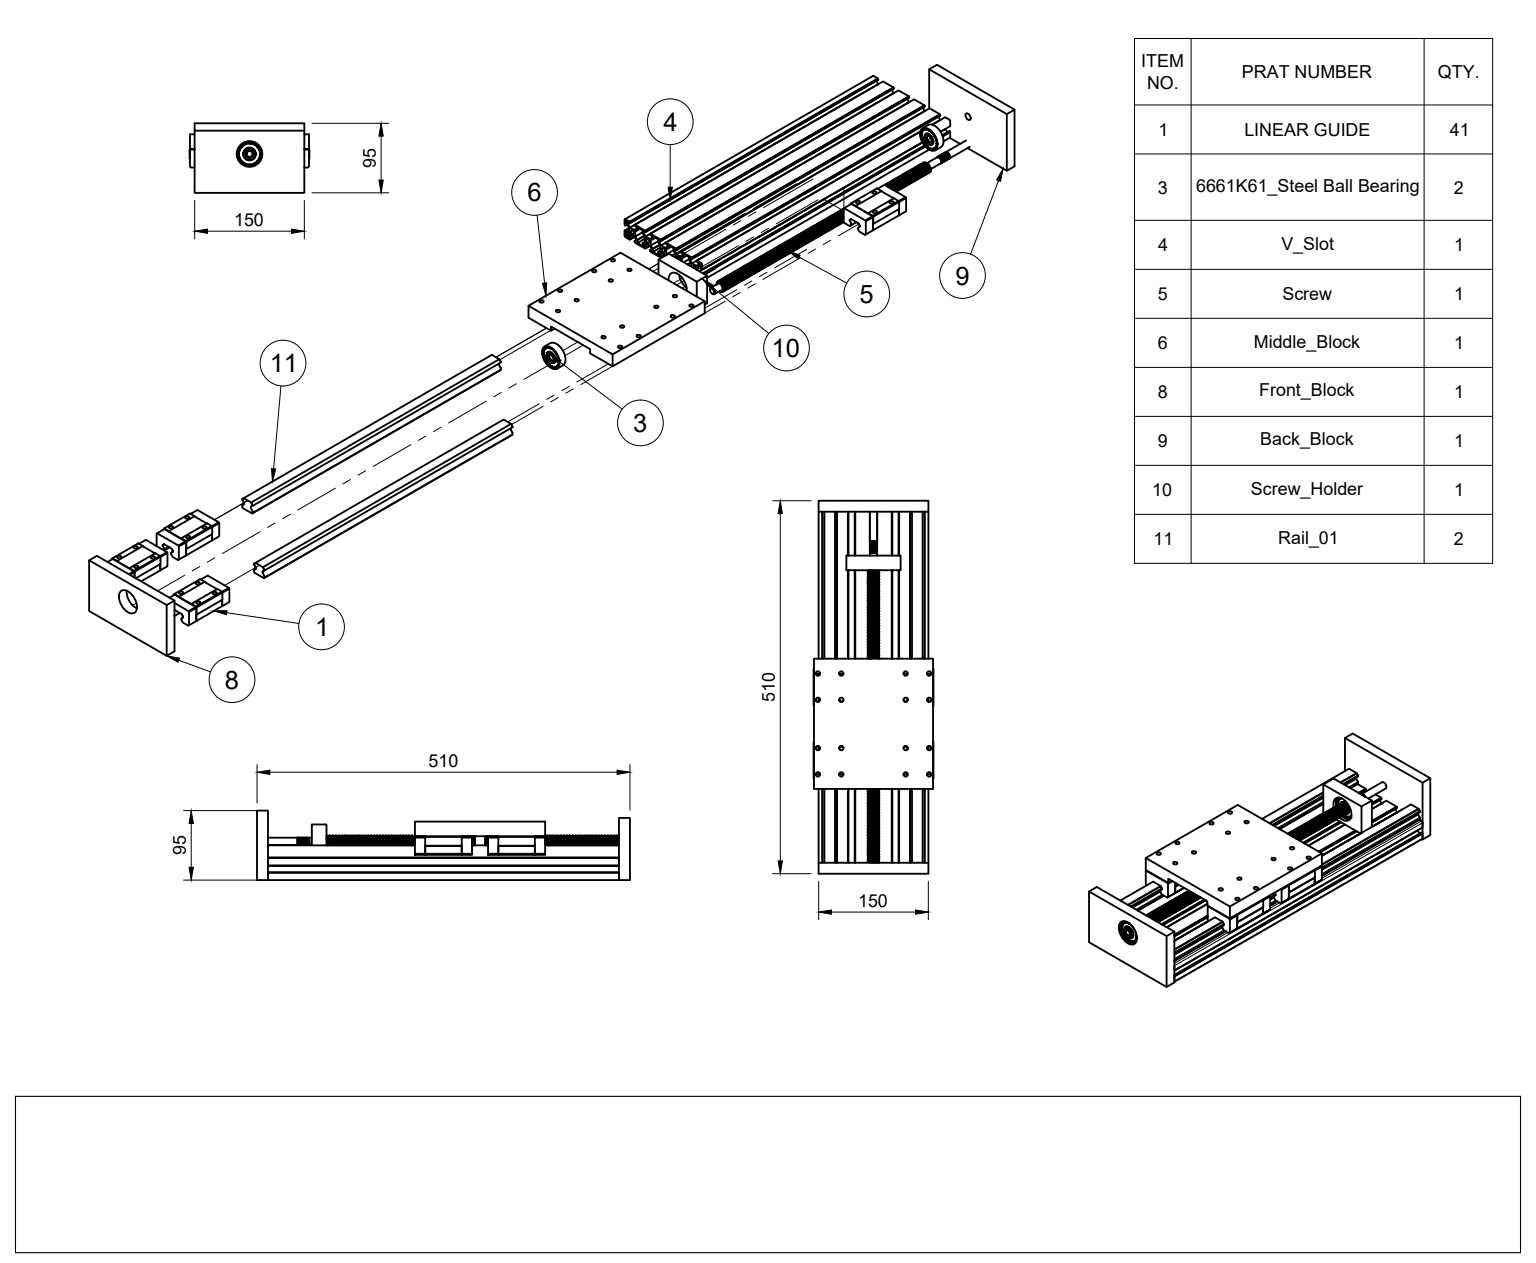
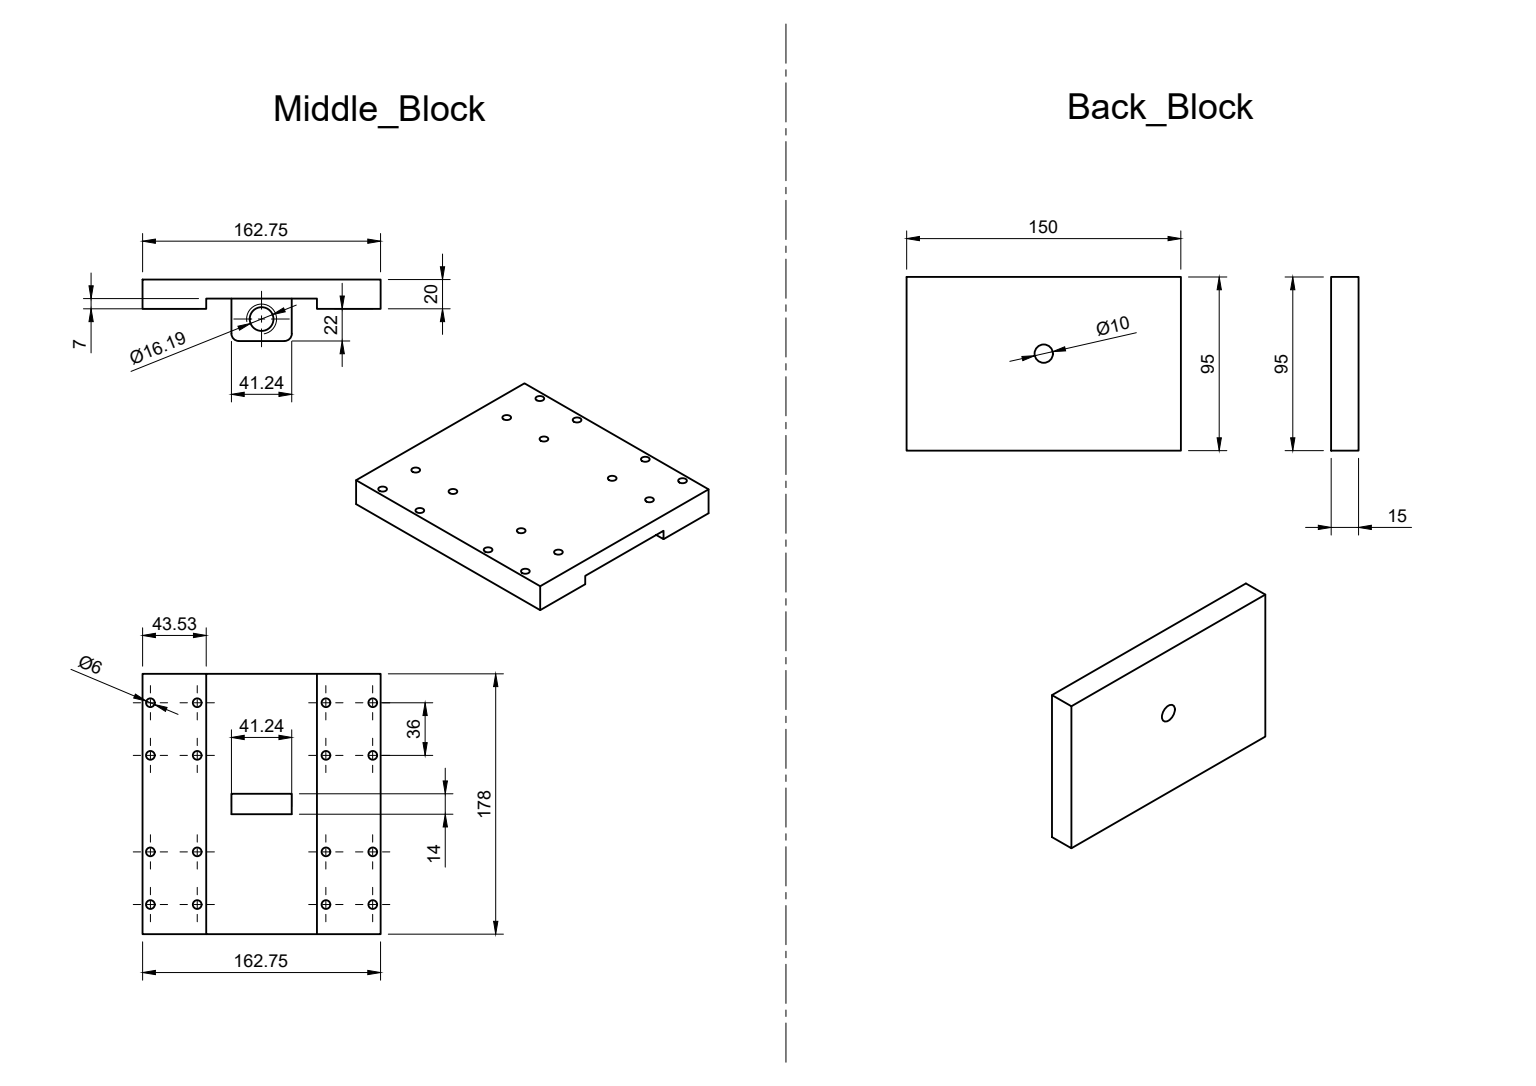
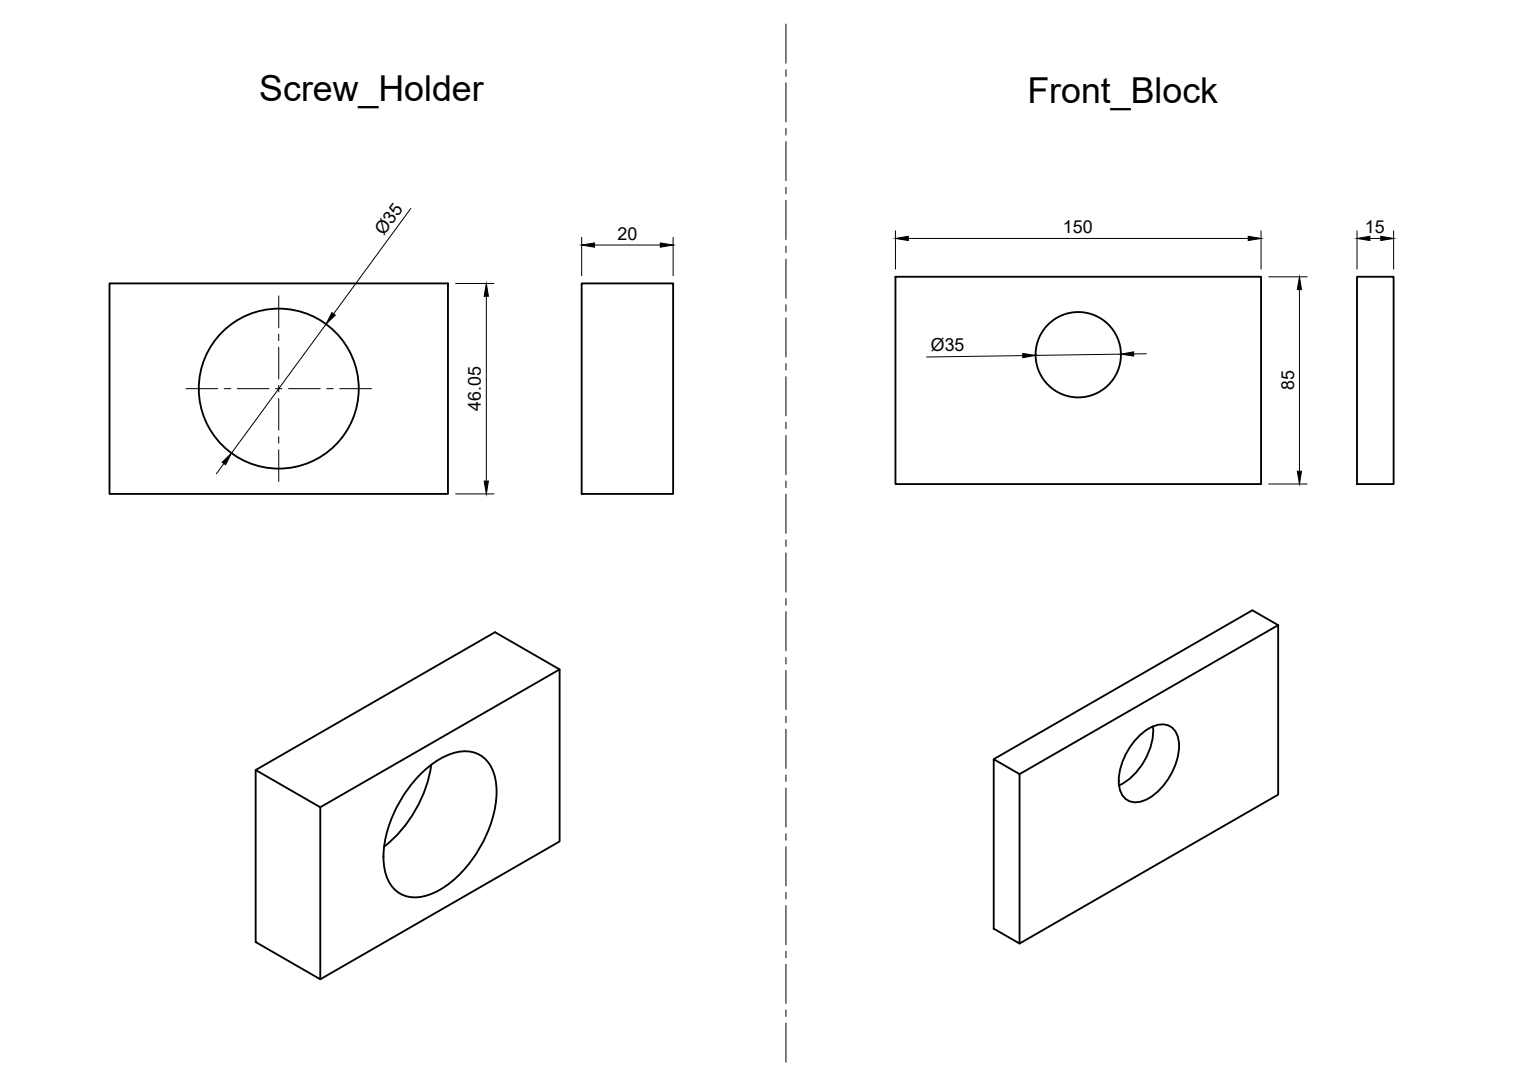
ISO-10303-21;
HEADER;
/* Generated by software containing ST-Developer
 * from STEP Tools, Inc. (www.steptools.com) 
 */

FILE_DESCRIPTION(
/* description */ (''),
/* implementation_level */ '2;1');

FILE_NAME(
/* name */ 'MAS-268',
/* time_stamp */ '2026-10-19T01:17:59+06:00',
/* author */ (''),
/* organization */ (''),
/* preprocessor_version */ 'ST-DEVELOPER v20.2',
/* originating_system */ 'Autodesk Translation Framework v15.15.0.0',
/* authorisation */ '');

FILE_SCHEMA (('AUTOMOTIVE_DESIGN { 1 0 10303 214 3 1 1 }'));
ENDSEC;

DATA;
#10=MECHANICAL_DESIGN_GEOMETRIC_PRESENTATION_REPRESENTATION('',(#729,#730,
#731,#732,#733,#734,#735,#736,#737,#738,#739,#740,#741,#742,#743,#744,#745,
#746,#747,#748,#749,#750,#751,#752,#753,#754),#48369);
#11=ITEM_DEFINED_TRANSFORMATION($,$,#20492,#21912);
#12=ITEM_DEFINED_TRANSFORMATION($,$,#20727,#21913);
#13=ITEM_DEFINED_TRANSFORMATION($,$,#20257,#21914);
#14=ITEM_DEFINED_TRANSFORMATION($,$,#20257,#21915);
#15=ITEM_DEFINED_TRANSFORMATION($,$,#20492,#21916);
#16=ITEM_DEFINED_TRANSFORMATION($,$,#20727,#21917);
#17=ITEM_DEFINED_TRANSFORMATION($,$,#21080,#21918);
#18=ITEM_DEFINED_TRANSFORMATION($,$,#21410,#21919);
#19=ITEM_DEFINED_TRANSFORMATION($,$,#21663,#21920);
#20=ITEM_DEFINED_TRANSFORMATION($,$,#21736,#21921);
#21=ITEM_DEFINED_TRANSFORMATION($,$,#21809,#21922);
#22=ITEM_DEFINED_TRANSFORMATION($,$,#21819,#21923);
#23=ITEM_DEFINED_TRANSFORMATION($,$,#21829,#21924);
#24=ITEM_DEFINED_TRANSFORMATION($,$,#21839,#21925);
#25=(
REPRESENTATION_RELATIONSHIP($,$,#48414,#48412)
REPRESENTATION_RELATIONSHIP_WITH_TRANSFORMATION(#11)
SHAPE_REPRESENTATION_RELATIONSHIP()
);
#26=(
REPRESENTATION_RELATIONSHIP($,$,#48415,#48412)
REPRESENTATION_RELATIONSHIP_WITH_TRANSFORMATION(#12)
SHAPE_REPRESENTATION_RELATIONSHIP()
);
#27=(
REPRESENTATION_RELATIONSHIP($,$,#48413,#48412)
REPRESENTATION_RELATIONSHIP_WITH_TRANSFORMATION(#13)
SHAPE_REPRESENTATION_RELATIONSHIP()
);
#28=(
REPRESENTATION_RELATIONSHIP($,$,#48413,#48412)
REPRESENTATION_RELATIONSHIP_WITH_TRANSFORMATION(#14)
SHAPE_REPRESENTATION_RELATIONSHIP()
);
#29=(
REPRESENTATION_RELATIONSHIP($,$,#48414,#48412)
REPRESENTATION_RELATIONSHIP_WITH_TRANSFORMATION(#15)
SHAPE_REPRESENTATION_RELATIONSHIP()
);
#30=(
REPRESENTATION_RELATIONSHIP($,$,#48415,#48412)
REPRESENTATION_RELATIONSHIP_WITH_TRANSFORMATION(#16)
SHAPE_REPRESENTATION_RELATIONSHIP()
);
#31=(
REPRESENTATION_RELATIONSHIP($,$,#48416,#48412)
REPRESENTATION_RELATIONSHIP_WITH_TRANSFORMATION(#17)
SHAPE_REPRESENTATION_RELATIONSHIP()
);
#32=(
REPRESENTATION_RELATIONSHIP($,$,#48417,#48412)
REPRESENTATION_RELATIONSHIP_WITH_TRANSFORMATION(#18)
SHAPE_REPRESENTATION_RELATIONSHIP()
);
#33=(
REPRESENTATION_RELATIONSHIP($,$,#48418,#48412)
REPRESENTATION_RELATIONSHIP_WITH_TRANSFORMATION(#19)
SHAPE_REPRESENTATION_RELATIONSHIP()
);
#34=(
REPRESENTATION_RELATIONSHIP($,$,#48419,#48412)
REPRESENTATION_RELATIONSHIP_WITH_TRANSFORMATION(#20)
SHAPE_REPRESENTATION_RELATIONSHIP()
);
#35=(
REPRESENTATION_RELATIONSHIP($,$,#48420,#48412)
REPRESENTATION_RELATIONSHIP_WITH_TRANSFORMATION(#21)
SHAPE_REPRESENTATION_RELATIONSHIP()
);
#36=(
REPRESENTATION_RELATIONSHIP($,$,#48421,#48412)
REPRESENTATION_RELATIONSHIP_WITH_TRANSFORMATION(#22)
SHAPE_REPRESENTATION_RELATIONSHIP()
);
#37=(
REPRESENTATION_RELATIONSHIP($,$,#48422,#48412)
REPRESENTATION_RELATIONSHIP_WITH_TRANSFORMATION(#23)
SHAPE_REPRESENTATION_RELATIONSHIP()
);
#38=(
REPRESENTATION_RELATIONSHIP($,$,#48423,#48412)
REPRESENTATION_RELATIONSHIP_WITH_TRANSFORMATION(#24)
SHAPE_REPRESENTATION_RELATIONSHIP()
);
#39=CONTEXT_DEPENDENT_SHAPE_REPRESENTATION(#25,#48398);
#40=CONTEXT_DEPENDENT_SHAPE_REPRESENTATION(#26,#48399);
#41=CONTEXT_DEPENDENT_SHAPE_REPRESENTATION(#27,#48400);
#42=CONTEXT_DEPENDENT_SHAPE_REPRESENTATION(#28,#48401);
#43=CONTEXT_DEPENDENT_SHAPE_REPRESENTATION(#29,#48402);
#44=CONTEXT_DEPENDENT_SHAPE_REPRESENTATION(#30,#48403);
#45=CONTEXT_DEPENDENT_SHAPE_REPRESENTATION(#31,#48404);
#46=CONTEXT_DEPENDENT_SHAPE_REPRESENTATION(#32,#48405);
#47=CONTEXT_DEPENDENT_SHAPE_REPRESENTATION(#33,#48406);
#48=CONTEXT_DEPENDENT_SHAPE_REPRESENTATION(#34,#48407);
#49=CONTEXT_DEPENDENT_SHAPE_REPRESENTATION(#35,#48408);
#50=CONTEXT_DEPENDENT_SHAPE_REPRESENTATION(#36,#48409);
#51=CONTEXT_DEPENDENT_SHAPE_REPRESENTATION(#37,#48410);
#52=CONTEXT_DEPENDENT_SHAPE_REPRESENTATION(#38,#48411);
#53=NEXT_ASSEMBLY_USAGE_OCCURRENCE('LINEAR GUIDE:1','LINEAR GUIDE:1',
'LINEAR GUIDE:1',#48425,#48427,'LINEAR GUIDE:1');
#54=NEXT_ASSEMBLY_USAGE_OCCURRENCE('6661K61_Steel Ball Bearing:1',
'6661K61_Steel Ball Bearing:1','6661K61_Steel Ball Bearing:1',#48425,#48428,
'6661K61_Steel Ball Bearing:1');
#55=NEXT_ASSEMBLY_USAGE_OCCURRENCE('LINEAR GUIDE(Mirror):1',
'LINEAR GUIDE(Mirror):1','LINEAR GUIDE(Mirror):1',#48425,#48426,
'LINEAR GUIDE(Mirror):1');
#56=NEXT_ASSEMBLY_USAGE_OCCURRENCE('LINEAR GUIDE(Mirror):2',
'LINEAR GUIDE(Mirror):2','LINEAR GUIDE(Mirror):2',#48425,#48426,
'LINEAR GUIDE(Mirror):2');
#57=NEXT_ASSEMBLY_USAGE_OCCURRENCE('LINEAR GUIDE:2','LINEAR GUIDE:2',
'LINEAR GUIDE:2',#48425,#48427,'LINEAR GUIDE:2');
#58=NEXT_ASSEMBLY_USAGE_OCCURRENCE('6661K61_Steel Ball Bearing:2',
'6661K61_Steel Ball Bearing:2','6661K61_Steel Ball Bearing:2',#48425,#48428,
'6661K61_Steel Ball Bearing:2');
#59=NEXT_ASSEMBLY_USAGE_OCCURRENCE('V_Slot:1','V_Slot:1','V_Slot:1',#48425,
#48429,'V_Slot:1');
#60=NEXT_ASSEMBLY_USAGE_OCCURRENCE('Screw:1','Screw:1','Screw:1',#48425,
#48430,'Screw:1');
#61=NEXT_ASSEMBLY_USAGE_OCCURRENCE('Middle_Block:1','Middle_Block:1',
'Middle_Block:1',#48425,#48431,'Middle_Block:1');
#62=NEXT_ASSEMBLY_USAGE_OCCURRENCE('Rail_02:1','Rail_02:1','Rail_02:1',
#48425,#48432,'Rail_02:1');
#63=NEXT_ASSEMBLY_USAGE_OCCURRENCE('Front_Block:1','Front_Block:1',
'Front_Block:1',#48425,#48433,'Front_Block:1');
#64=NEXT_ASSEMBLY_USAGE_OCCURRENCE('Back_Block:1','Back_Block:1',
'Back_Block:1',#48425,#48434,'Back_Block:1');
#65=NEXT_ASSEMBLY_USAGE_OCCURRENCE('Screw_Holder:1','Screw_Holder:1',
'Screw_Holder:1',#48425,#48435,'Screw_Holder:1');
#66=NEXT_ASSEMBLY_USAGE_OCCURRENCE('Rail_01:1','Rail_01:1','Rail_01:1',
#48425,#48436,'Rail_01:1');
#67=B_SPLINE_SURFACE_WITH_KNOTS('',3,3,((#40580,#40581,#40582,#40583,#40584,
#40585,#40586,#40587,#40588,#40589,#40590,#40591,#40592,#40593,#40594,#40595,
#40596,#40597,#40598,#40599,#40600,#40601,#40602,#40603,#40604,#40605,#40606,
#40607,#40608,#40609,#40610,#40611,#40612,#40613,#40614,#40615,#40616,#40617,
#40618,#40619,#40620,#40621,#40622,#40623,#40624,#40625,#40626,#40627,#40628,
#40629,#40630,#40631,#40632,#40633,#40634,#40635,#40636,#40637,#40638,#40639,
#40640,#40641,#40642,#40643,#40644,#40645,#40646,#40647,#40648,#40649,#40650,
#40651,#40652,#40653,#40654,#40655,#40656,#40657,#40658,#40659,#40660,#40661,
#40662,#40663,#40664,#40665,#40666,#40667,#40668,#40669,#40670,#40671,#40672,
#40673,#40674,#40675,#40676,#40677,#40678,#40679,#40680,#40681,#40682,#40683,
#40684,#40685,#40686,#40687,#40688,#40689,#40690,#40691,#40692,#40693,#40694,
#40695,#40696,#40697,#40698,#40699,#40700,#40701,#40702,#40703,#40704,#40705,
#40706,#40707,#40708,#40709,#40710,#40711,#40712,#40713,#40714,#40715,#40716,
#40717,#40718,#40719,#40720,#40721,#40722,#40723,#40724,#40725,#40726,#40727,
#40728,#40729,#40730,#40731,#40732,#40733,#40734,#40735,#40736,#40737,#40738,
#40739,#40740,#40741,#40742,#40743,#40744,#40745,#40746,#40747,#40748,#40749,
#40750,#40751,#40752,#40753,#40754,#40755,#40756,#40757,#40758,#40759,#40760,
#40761,#40762,#40763,#40764,#40765,#40766,#40767,#40768,#40769,#40770,#40771,
#40772,#40773,#40774,#40775,#40776,#40777,#40778,#40779,#40780,#40781,#40782,
#40783,#40784,#40785,#40786,#40787,#40788,#40789,#40790,#40791,#40792,#40793,
#40794,#40795,#40796,#40797,#40798,#40799,#40800,#40801,#40802,#40803,#40804,
#40805,#40806,#40807,#40808,#40809,#40810,#40811,#40812,#40813,#40814,#40815,
#40816,#40817,#40818,#40819,#40820,#40821,#40822,#40823,#40824,#40825,#40826,
#40827,#40828,#40829,#40830,#40831,#40832,#40833,#40834,#40835,#40836,#40837,
#40838,#40839,#40840,#40841,#40842,#40843,#40844,#40845,#40846,#40847,#40848,
#40849,#40850,#40851,#40852,#40853,#40854,#40855,#40856,#40857,#40858,#40859,
#40860,#40861,#40862,#40863,#40864,#40865,#40866,#40867,#40868,#40869,#40870,
#40871,#40872,#40873,#40874,#40875,#40876,#40877,#40878,#40879,#40880,#40881,
#40882,#40883,#40884,#40885,#40886,#40887,#40888,#40889,#40890,#40891,#40892,
#40893,#40894,#40895,#40896,#40897,#40898,#40899,#40900,#40901,#40902,#40903,
#40904,#40905,#40906,#40907,#40908,#40909,#40910,#40911,#40912,#40913,#40914,
#40915,#40916,#40917,#40918,#40919,#40920,#40921,#40922,#40923,#40924,#40925,
#40926,#40927,#40928,#40929,#40930,#40931,#40932,#40933,#40934,#40935,#40936,
#40937,#40938,#40939,#40940,#40941,#40942,#40943,#40944,#40945,#40946,#40947,
#40948,#40949,#40950,#40951,#40952,#40953,#40954,#40955,#40956,#40957,#40958,
#40959,#40960,#40961,#40962,#40963,#40964,#40965,#40966,#40967,#40968,#40969,
#40970,#40971,#40972,#40973,#40974,#40975,#40976,#40977,#40978,#40979,#40980,
#40981,#40982,#40983,#40984,#40985,#40986,#40987,#40988,#40989,#40990,#40991,
#40992,#40993,#40994,#40995,#40996,#40997,#40998,#40999,#41000,#41001,#41002,
#41003,#41004,#41005,#41006,#41007,#41008,#41009,#41010,#41011,#41012,#41013,
#41014,#41015,#41016,#41017,#41018,#41019,#41020,#41021,#41022,#41023,#41024,
#41025,#41026,#41027,#41028,#41029,#41030,#41031,#41032,#41033,#41034,#41035,
#41036,#41037,#41038,#41039,#41040,#41041,#41042,#41043,#41044,#41045,#41046,
#41047,#41048,#41049,#41050,#41051,#41052,#41053,#41054,#41055,#41056,#41057,
#41058,#41059,#41060,#41061,#41062,#41063,#41064,#41065,#41066,#41067,#41068,
#41069,#41070,#41071,#41072,#41073,#41074,#41075,#41076,#41077,#41078,#41079,
#41080,#41081,#41082,#41083,#41084,#41085,#41086,#41087,#41088,#41089,#41090,
#41091,#41092,#41093,#41094,#41095,#41096,#41097,#41098,#41099,#41100,#41101,
#41102,#41103,#41104,#41105,#41106,#41107,#41108,#41109,#41110,#41111,#41112,
#41113,#41114,#41115,#41116,#41117,#41118,#41119,#41120,#41121,#41122,#41123,
#41124,#41125,#41126,#41127,#41128,#41129,#41130,#41131,#41132,#41133,#41134,
#41135,#41136,#41137,#41138,#41139,#41140,#41141,#41142,#41143,#41144,#41145,
#41146,#41147,#41148,#41149,#41150,#41151,#41152,#41153,#41154,#41155,#41156,
#41157,#41158,#41159,#41160,#41161,#41162,#41163,#41164,#41165,#41166,#41167,
#41168,#41169,#41170,#41171,#41172,#41173,#41174,#41175,#41176,#41177,#41178,
#41179,#41180,#41181,#41182,#41183,#41184,#41185,#41186,#41187,#41188,#41189,
#41190,#41191,#41192,#41193,#41194,#41195,#41196,#41197,#41198,#41199,#41200,
#41201,#41202,#41203,#41204,#41205,#41206,#41207,#41208,#41209,#41210,#41211,
#41212,#41213,#41214,#41215,#41216,#41217,#41218,#41219,#41220,#41221,#41222,
#41223,#41224,#41225,#41226,#41227,#41228,#41229,#41230,#41231,#41232,#41233,
#41234,#41235,#41236,#41237,#41238,#41239,#41240,#41241,#41242,#41243,#41244,
#41245,#41246,#41247,#41248,#41249,#41250,#41251,#41252,#41253,#41254,#41255,
#41256,#41257,#41258,#41259,#41260,#41261,#41262,#41263,#41264,#41265,#41266,
#41267,#41268,#41269,#41270,#41271,#41272,#41273,#41274,#41275,#41276,#41277,
#41278,#41279,#41280,#41281,#41282,#41283,#41284,#41285,#41286,#41287,#41288,
#41289,#41290,#41291,#41292,#41293,#41294,#41295,#41296,#41297,#41298,#41299,
#41300,#41301,#41302,#41303,#41304),(#41305,#41306,#41307,#41308,#41309,
#41310,#41311,#41312,#41313,#41314,#41315,#41316,#41317,#41318,#41319,#41320,
#41321,#41322,#41323,#41324,#41325,#41326,#41327,#41328,#41329,#41330,#41331,
#41332,#41333,#41334,#41335,#41336,#41337,#41338,#41339,#41340,#41341,#41342,
#41343,#41344,#41345,#41346,#41347,#41348,#41349,#41350,#41351,#41352,#41353,
#41354,#41355,#41356,#41357,#41358,#41359,#41360,#41361,#41362,#41363,#41364,
#41365,#41366,#41367,#41368,#41369,#41370,#41371,#41372,#41373,#41374,#41375,
#41376,#41377,#41378,#41379,#41380,#41381,#41382,#41383,#41384,#41385,#41386,
#41387,#41388,#41389,#41390,#41391,#41392,#41393,#41394,#41395,#41396,#41397,
#41398,#41399,#41400,#41401,#41402,#41403,#41404,#41405,#41406,#41407,#41408,
#41409,#41410,#41411,#41412,#41413,#41414,#41415,#41416,#41417,#41418,#41419,
#41420,#41421,#41422,#41423,#41424,#41425,#41426,#41427,#41428,#41429,#41430,
#41431,#41432,#41433,#41434,#41435,#41436,#41437,#41438,#41439,#41440,#41441,
#41442,#41443,#41444,#41445,#41446,#41447,#41448,#41449,#41450,#41451,#41452,
#41453,#41454,#41455,#41456,#41457,#41458,#41459,#41460,#41461,#41462,#41463,
#41464,#41465,#41466,#41467,#41468,#41469,#41470,#41471,#41472,#41473,#41474,
#41475,#41476,#41477,#41478,#41479,#41480,#41481,#41482,#41483,#41484,#41485,
#41486,#41487,#41488,#41489,#41490,#41491,#41492,#41493,#41494,#41495,#41496,
#41497,#41498,#41499,#41500,#41501,#41502,#41503,#41504,#41505,#41506,#41507,
#41508,#41509,#41510,#41511,#41512,#41513,#41514,#41515,#41516,#41517,#41518,
#41519,#41520,#41521,#41522,#41523,#41524,#41525,#41526,#41527,#41528,#41529,
#41530,#41531,#41532,#41533,#41534,#41535,#41536,#41537,#41538,#41539,#41540,
#41541,#41542,#41543,#41544,#41545,#41546,#41547,#41548,#41549,#41550,#41551,
#41552,#41553,#41554,#41555,#41556,#41557,#41558,#41559,#41560,#41561,#41562,
#41563,#41564,#41565,#41566,#41567,#41568,#41569,#41570,#41571,#41572,#41573,
#41574,#41575,#41576,#41577,#41578,#41579,#41580,#41581,#41582,#41583,#41584,
#41585,#41586,#41587,#41588,#41589,#41590,#41591,#41592,#41593,#41594,#41595,
#41596,#41597,#41598,#41599,#41600,#41601,#41602,#41603,#41604,#41605,#41606,
#41607,#41608,#41609,#41610,#41611,#41612,#41613,#41614,#41615,#41616,#41617,
#41618,#41619,#41620,#41621,#41622,#41623,#41624,#41625,#41626,#41627,#41628,
#41629,#41630,#41631,#41632,#41633,#41634,#41635,#41636,#41637,#41638,#41639,
#41640,#41641,#41642,#41643,#41644,#41645,#41646,#41647,#41648,#41649,#41650,
#41651,#41652,#41653,#41654,#41655,#41656,#41657,#41658,#41659,#41660,#41661,
#41662,#41663,#41664,#41665,#41666,#41667,#41668,#41669,#41670,#41671,#41672,
#41673,#41674,#41675,#41676,#41677,#41678,#41679,#41680,#41681,#41682,#41683,
#41684,#41685,#41686,#41687,#41688,#41689,#41690,#41691,#41692,#41693,#41694,
#41695,#41696,#41697,#41698,#41699,#41700,#41701,#41702,#41703,#41704,#41705,
#41706,#41707,#41708,#41709,#41710,#41711,#41712,#41713,#41714,#41715,#41716,
#41717,#41718,#41719,#41720,#41721,#41722,#41723,#41724,#41725,#41726,#41727,
#41728,#41729,#41730,#41731,#41732,#41733,#41734,#41735,#41736,#41737,#41738,
#41739,#41740,#41741,#41742,#41743,#41744,#41745,#41746,#41747,#41748,#41749,
#41750,#41751,#41752,#41753,#41754,#41755,#41756,#41757,#41758,#41759,#41760,
#41761,#41762,#41763,#41764,#41765,#41766,#41767,#41768,#41769,#41770,#41771,
#41772,#41773,#41774,#41775,#41776,#41777,#41778,#41779,#41780,#41781,#41782,
#41783,#41784,#41785,#41786,#41787,#41788,#41789,#41790,#41791,#41792,#41793,
#41794,#41795,#41796,#41797,#41798,#41799,#41800,#41801,#41802,#41803,#41804,
#41805,#41806,#41807,#41808,#41809,#41810,#41811,#41812,#41813,#41814,#41815,
#41816,#41817,#41818,#41819,#41820,#41821,#41822,#41823,#41824,#41825,#41826,
#41827,#41828,#41829,#41830,#41831,#41832,#41833,#41834,#41835,#41836,#41837,
#41838,#41839,#41840,#41841,#41842,#41843,#41844,#41845,#41846,#41847,#41848,
#41849,#41850,#41851,#41852,#41853,#41854,#41855,#41856,#41857,#41858,#41859,
#41860,#41861,#41862,#41863,#41864,#41865,#41866,#41867,#41868,#41869,#41870,
#41871,#41872,#41873,#41874,#41875,#41876,#41877,#41878,#41879,#41880,#41881,
#41882,#41883,#41884,#41885,#41886,#41887,#41888,#41889,#41890,#41891,#41892,
#41893,#41894,#41895,#41896,#41897,#41898,#41899,#41900,#41901,#41902,#41903,
#41904,#41905,#41906,#41907,#41908,#41909,#41910,#41911,#41912,#41913,#41914,
#41915,#41916,#41917,#41918,#41919,#41920,#41921,#41922,#41923,#41924,#41925,
#41926,#41927,#41928,#41929,#41930,#41931,#41932,#41933,#41934,#41935,#41936,
#41937,#41938,#41939,#41940,#41941,#41942,#41943,#41944,#41945,#41946,#41947,
#41948,#41949,#41950,#41951,#41952,#41953,#41954,#41955,#41956,#41957,#41958,
#41959,#41960,#41961,#41962,#41963,#41964,#41965,#41966,#41967,#41968,#41969,
#41970,#41971,#41972,#41973,#41974,#41975,#41976,#41977,#41978,#41979,#41980,
#41981,#41982,#41983,#41984,#41985,#41986,#41987,#41988,#41989,#41990,#41991,
#41992,#41993,#41994,#41995,#41996,#41997,#41998,#41999,#42000,#42001,#42002,
#42003,#42004,#42005,#42006,#42007,#42008,#42009,#42010,#42011,#42012,#42013,
#42014,#42015,#42016,#42017,#42018,#42019,#42020,#42021,#42022,#42023,#42024,
#42025,#42026,#42027,#42028,#42029),(#42030,#42031,#42032,#42033,#42034,
#42035,#42036,#42037,#42038,#42039,#42040,#42041,#42042,#42043,#42044,#42045,
#42046,#42047,#42048,#42049,#42050,#42051,#42052,#42053,#42054,#42055,#42056,
#42057,#42058,#42059,#42060,#42061,#42062,#42063,#42064,#42065,#42066,#42067,
#42068,#42069,#42070,#42071,#42072,#42073,#42074,#42075,#42076,#42077,#42078,
#42079,#42080,#42081,#42082,#42083,#42084,#42085,#42086,#42087,#42088,#42089,
#42090,#42091,#42092,#42093,#42094,#42095,#42096,#42097,#42098,#42099,#42100,
#42101,#42102,#42103,#42104,#42105,#42106,#42107,#42108,#42109,#42110,#42111,
#42112,#42113,#42114,#42115,#42116,#42117,#42118,#42119,#42120,#42121,#42122,
#42123,#42124,#42125,#42126,#42127,#42128,#42129,#42130,#42131,#42132,#42133,
#42134,#42135,#42136,#42137,#42138,#42139,#42140,#42141,#42142,#42143,#42144,
#42145,#42146,#42147,#42148,#42149,#42150,#42151,#42152,#42153,#42154,#42155,
#42156,#42157,#42158,#42159,#42160,#42161,#42162,#42163,#42164,#42165,#42166,
#42167,#42168,#42169,#42170,#42171,#42172,#42173,#42174,#42175,#42176,#42177,
#42178,#42179,#42180,#42181,#42182,#42183,#42184,#42185,#42186,#42187,#42188,
#42189,#42190,#42191,#42192,#42193,#42194,#42195,#42196,#42197,#42198,#42199,
#42200,#42201,#42202,#42203,#42204,#42205,#42206,#42207,#42208,#42209,#42210,
#42211,#42212,#42213,#42214,#42215,#42216,#42217,#42218,#42219,#42220,#42221,
#42222,#42223,#42224,#42225,#42226,#42227,#42228,#42229,#42230,#42231,#42232,
#42233,#42234,#42235,#42236,#42237,#42238,#42239,#42240,#42241,#42242,#42243,
#42244,#42245,#42246,#42247,#42248,#42249,#42250,#42251,#42252,#42253,#42254,
#42255,#42256,#42257,#42258,#42259,#42260,#42261,#42262,#42263,#42264,#42265,
#42266,#42267,#42268,#42269,#42270,#42271,#42272,#42273,#42274,#42275,#42276,
#42277,#42278,#42279,#42280,#42281,#42282,#42283,#42284,#42285,#42286,#42287,
#42288,#42289,#42290,#42291,#42292,#42293,#42294,#42295,#42296,#42297,#42298,
#42299,#42300,#42301,#42302,#42303,#42304,#42305,#42306,#42307,#42308,#42309,
#42310,#42311,#42312,#42313,#42314,#42315,#42316,#42317,#42318,#42319,#42320,
#42321,#42322,#42323,#42324,#42325,#42326,#42327,#42328,#42329,#42330,#42331,
#42332,#42333,#42334,#42335,#42336,#42337,#42338,#42339,#42340,#42341,#42342,
#42343,#42344,#42345,#42346,#42347,#42348,#42349,#42350,#42351,#42352,#42353,
#42354,#42355,#42356,#42357,#42358,#42359,#42360,#42361,#42362,#42363,#42364,
#42365,#42366,#42367,#42368,#42369,#42370,#42371,#42372,#42373,#42374,#42375,
#42376,#42377,#42378,#42379,#42380,#42381,#42382,#42383,#42384,#42385,#42386,
#42387,#42388,#42389,#42390,#42391,#42392,#42393,#42394,#42395,#42396,#42397,
#42398,#42399,#42400,#42401,#42402,#42403,#42404,#42405,#42406,#42407,#42408,
#42409,#42410,#42411,#42412,#42413,#42414,#42415,#42416,#42417,#42418,#42419,
#42420,#42421,#42422,#42423,#42424,#42425,#42426,#42427,#42428,#42429,#42430,
#42431,#42432,#42433,#42434,#42435,#42436,#42437,#42438,#42439,#42440,#42441,
#42442,#42443,#42444,#42445,#42446,#42447,#42448,#42449,#42450,#42451,#42452,
#42453,#42454,#42455,#42456,#42457,#42458,#42459,#42460,#42461,#42462,#42463,
#42464,#42465,#42466,#42467,#42468,#42469,#42470,#42471,#42472,#42473,#42474,
#42475,#42476,#42477,#42478,#42479,#42480,#42481,#42482,#42483,#42484,#42485,
#42486,#42487,#42488,#42489,#42490,#42491,#42492,#42493,#42494,#42495,#42496,
#42497,#42498,#42499,#42500,#42501,#42502,#42503,#42504,#42505,#42506,#42507,
#42508,#42509,#42510,#42511,#42512,#42513,#42514,#42515,#42516,#42517,#42518,
#42519,#42520,#42521,#42522,#42523,#42524,#42525,#42526,#42527,#42528,#42529,
#42530,#42531,#42532,#42533,#42534,#42535,#42536,#42537,#42538,#42539,#42540,
#42541,#42542,#42543,#42544,#42545,#42546,#42547,#42548,#42549,#42550,#42551,
#42552,#42553,#42554,#42555,#42556,#42557,#42558,#42559,#42560,#42561,#42562,
#42563,#42564,#42565,#42566,#42567,#42568,#42569,#42570,#42571,#42572,#42573,
#42574,#42575,#42576,#42577,#42578,#42579,#42580,#42581,#42582,#42583,#42584,
#42585,#42586,#42587,#42588,#42589,#42590,#42591,#42592,#42593,#42594,#42595,
#42596,#42597,#42598,#42599,#42600,#42601,#42602,#42603,#42604,#42605,#42606,
#42607,#42608,#42609,#42610,#42611,#42612,#42613,#42614,#42615,#42616,#42617,
#42618,#42619,#42620,#42621,#42622,#42623,#42624,#42625,#42626,#42627,#42628,
#42629,#42630,#42631,#42632,#42633,#42634,#42635,#42636,#42637,#42638,#42639,
#42640,#42641,#42642,#42643,#42644,#42645,#42646,#42647,#42648,#42649,#42650,
#42651,#42652,#42653,#42654,#42655,#42656,#42657,#42658,#42659,#42660,#42661,
#42662,#42663,#42664,#42665,#42666,#42667,#42668,#42669,#42670,#42671,#42672,
#42673,#42674,#42675,#42676,#42677,#42678,#42679,#42680,#42681,#42682,#42683,
#42684,#42685,#42686,#42687,#42688,#42689,#42690,#42691,#42692,#42693,#42694,
#42695,#42696,#42697,#42698,#42699,#42700,#42701,#42702,#42703,#42704,#42705,
#42706,#42707,#42708,#42709,#42710,#42711,#42712,#42713,#42714,#42715,#42716,
#42717,#42718,#42719,#42720,#42721,#42722,#42723,#42724,#42725,#42726,#42727,
#42728,#42729,#42730,#42731,#42732,#42733,#42734,#42735,#42736,#42737,#42738,
#42739,#42740,#42741,#42742,#42743,#42744,#42745,#42746,#42747,#42748,#42749,
#42750,#42751,#42752,#42753,#42754),(#42755,#42756,#42757,#42758,#42759,
#42760,#42761,#42762,#42763,#42764,#42765,#42766,#42767,#42768,#42769,#42770,
#42771,#42772,#42773,#42774,#42775,#42776,#42777,#42778,#42779,#42780,#42781,
#42782,#42783,#42784,#42785,#42786,#42787,#42788,#42789,#42790,#42791,#42792,
#42793,#42794,#42795,#42796,#42797,#42798,#42799,#42800,#42801,#42802,#42803,
#42804,#42805,#42806,#42807,#42808,#42809,#42810,#42811,#42812,#42813,#42814,
#42815,#42816,#42817,#42818,#42819,#42820,#42821,#42822,#42823,#42824,#42825,
#42826,#42827,#42828,#42829,#42830,#42831,#42832,#42833,#42834,#42835,#42836,
#42837,#42838,#42839,#42840,#42841,#42842,#42843,#42844,#42845,#42846,#42847,
#42848,#42849,#42850,#42851,#42852,#42853,#42854,#42855,#42856,#42857,#42858,
#42859,#42860,#42861,#42862,#42863,#42864,#42865,#42866,#42867,#42868,#42869,
#42870,#42871,#42872,#42873,#42874,#42875,#42876,#42877,#42878,#42879,#42880,
#42881,#42882,#42883,#42884,#42885,#42886,#42887,#42888,#42889,#42890,#42891,
#42892,#42893,#42894,#42895,#42896,#42897,#42898,#42899,#42900,#42901,#42902,
#42903,#42904,#42905,#42906,#42907,#42908,#42909,#42910,#42911,#42912,#42913,
#42914,#42915,#42916,#42917,#42918,#42919,#42920,#42921,#42922,#42923,#42924,
#42925,#42926,#42927,#42928,#42929,#42930,#42931,#42932,#42933,#42934,#42935,
#42936,#42937,#42938,#42939,#42940,#42941,#42942,#42943,#42944,#42945,#42946,
#42947,#42948,#42949,#42950,#42951,#42952,#42953,#42954,#42955,#42956,#42957,
#42958,#42959,#42960,#42961,#42962,#42963,#42964,#42965,#42966,#42967,#42968,
#42969,#42970,#42971,#42972,#42973,#42974,#42975,#42976,#42977,#42978,#42979,
#42980,#42981,#42982,#42983,#42984,#42985,#42986,#42987,#42988,#42989,#42990,
#42991,#42992,#42993,#42994,#42995,#42996,#42997,#42998,#42999,#43000,#43001,
#43002,#43003,#43004,#43005,#43006,#43007,#43008,#43009,#43010,#43011,#43012,
#43013,#43014,#43015,#43016,#43017,#43018,#43019,#43020,#43021,#43022,#43023,
#43024,#43025,#43026,#43027,#43028,#43029,#43030,#43031,#43032,#43033,#43034,
#43035,#43036,#43037,#43038,#43039,#43040,#43041,#43042,#43043,#43044,#43045,
#43046,#43047,#43048,#43049,#43050,#43051,#43052,#43053,#43054,#43055,#43056,
#43057,#43058,#43059,#43060,#43061,#43062,#43063,#43064,#43065,#43066,#43067,
#43068,#43069,#43070,#43071,#43072,#43073,#43074,#43075,#43076,#43077,#43078,
#43079,#43080,#43081,#43082,#43083,#43084,#43085,#43086,#43087,#43088,#43089,
#43090,#43091,#43092,#43093,#43094,#43095,#43096,#43097,#43098,#43099,#43100,
#43101,#43102,#43103,#43104,#43105,#43106,#43107,#43108,#43109,#43110,#43111,
#43112,#43113,#43114,#43115,#43116,#43117,#43118,#43119,#43120,#43121,#43122,
#43123,#43124,#43125,#43126,#43127,#43128,#43129,#43130,#43131,#43132,#43133,
#43134,#43135,#43136,#43137,#43138,#43139,#43140,#43141,#43142,#43143,#43144,
#43145,#43146,#43147,#43148,#43149,#43150,#43151,#43152,#43153,#43154,#43155,
#43156,#43157,#43158,#43159,#43160,#43161,#43162,#43163,#43164,#43165,#43166,
#43167,#43168,#43169,#43170,#43171,#43172,#43173,#43174,#43175,#43176,#43177,
#43178,#43179,#43180,#43181,#43182,#43183,#43184,#43185,#43186,#43187,#43188,
#43189,#43190,#43191,#43192,#43193,#43194,#43195,#43196,#43197,#43198,#43199,
#43200,#43201,#43202,#43203,#43204,#43205,#43206,#43207,#43208,#43209,#43210,
#43211,#43212,#43213,#43214,#43215,#43216,#43217,#43218,#43219,#43220,#43221,
#43222,#43223,#43224,#43225,#43226,#43227,#43228,#43229,#43230,#43231,#43232,
#43233,#43234,#43235,#43236,#43237,#43238,#43239,#43240,#43241,#43242,#43243,
#43244,#43245,#43246,#43247,#43248,#43249,#43250,#43251,#43252,#43253,#43254,
#43255,#43256,#43257,#43258,#43259,#43260,#43261,#43262,#43263,#43264,#43265,
#43266,#43267,#43268,#43269,#43270,#43271,#43272,#43273,#43274,#43275,#43276,
#43277,#43278,#43279,#43280,#43281,#43282,#43283,#43284,#43285,#43286,#43287,
#43288,#43289,#43290,#43291,#43292,#43293,#43294,#43295,#43296,#43297,#43298,
#43299,#43300,#43301,#43302,#43303,#43304,#43305,#43306,#43307,#43308,#43309,
#43310,#43311,#43312,#43313,#43314,#43315,#43316,#43317,#43318,#43319,#43320,
#43321,#43322,#43323,#43324,#43325,#43326,#43327,#43328,#43329,#43330,#43331,
#43332,#43333,#43334,#43335,#43336,#43337,#43338,#43339,#43340,#43341,#43342,
#43343,#43344,#43345,#43346,#43347,#43348,#43349,#43350,#43351,#43352,#43353,
#43354,#43355,#43356,#43357,#43358,#43359,#43360,#43361,#43362,#43363,#43364,
#43365,#43366,#43367,#43368,#43369,#43370,#43371,#43372,#43373,#43374,#43375,
#43376,#43377,#43378,#43379,#43380,#43381,#43382,#43383,#43384,#43385,#43386,
#43387,#43388,#43389,#43390,#43391,#43392,#43393,#43394,#43395,#43396,#43397,
#43398,#43399,#43400,#43401,#43402,#43403,#43404,#43405,#43406,#43407,#43408,
#43409,#43410,#43411,#43412,#43413,#43414,#43415,#43416,#43417,#43418,#43419,
#43420,#43421,#43422,#43423,#43424,#43425,#43426,#43427,#43428,#43429,#43430,
#43431,#43432,#43433,#43434,#43435,#43436,#43437,#43438,#43439,#43440,#43441,
#43442,#43443,#43444,#43445,#43446,#43447,#43448,#43449,#43450,#43451,#43452,
#43453,#43454,#43455,#43456,#43457,#43458,#43459,#43460,#43461,#43462,#43463,
#43464,#43465,#43466,#43467,#43468,#43469,#43470,#43471,#43472,#43473,#43474,
#43475,#43476,#43477,#43478,#43479)),.UNSPECIFIED.,.F.,.F.,.F.,(4,4),(4,
1,1,1,1,1,1,1,1,1,1,1,1,1,1,1,1,1,1,1,1,1,1,1,1,1,1,1,1,1,1,1,1,1,1,1,1,
1,1,1,1,1,1,1,1,1,1,1,1,1,1,1,1,1,1,1,1,1,1,1,1,1,1,1,1,1,1,1,1,1,1,1,1,
1,1,1,1,1,1,1,1,1,1,1,1,1,1,1,1,1,1,1,1,1,1,1,1,1,1,1,1,1,1,1,1,1,1,1,1,
1,1,1,1,1,1,1,1,1,1,1,1,1,1,1,1,1,1,1,1,1,1,1,1,1,1,1,1,1,1,1,1,1,1,1,1,
1,1,1,1,1,1,1,1,1,1,1,1,1,1,1,1,1,1,1,1,1,1,1,1,1,1,1,1,1,1,1,1,1,1,1,1,
1,1,1,1,1,1,1,1,1,1,1,1,1,1,1,1,1,1,1,1,1,1,1,1,1,1,1,1,1,1,1,1,1,1,1,1,
1,1,1,1,1,1,1,1,1,1,1,1,1,1,1,1,1,1,1,1,1,1,1,1,1,1,1,1,1,1,1,1,1,1,1,1,
1,1,1,1,1,1,1,1,1,1,1,1,1,1,1,1,1,1,1,1,1,1,1,1,1,1,1,1,1,1,1,1,1,1,1,1,
1,1,1,1,1,1,1,1,1,1,1,1,1,1,1,1,1,1,1,1,1,1,1,1,1,1,1,1,1,1,1,1,1,1,1,1,
1,1,1,1,1,1,1,1,1,1,1,1,1,1,1,1,1,1,1,1,1,1,1,1,1,1,1,1,1,1,1,1,1,1,1,1,
1,1,1,1,1,1,1,1,1,1,1,1,1,1,1,1,1,1,1,1,1,1,1,1,1,1,1,1,1,1,1,1,1,1,1,1,
1,1,1,1,1,1,1,1,1,1,1,1,1,1,1,1,1,1,1,1,1,1,1,1,1,1,1,1,1,1,1,1,1,1,1,1,
1,1,1,1,1,1,1,1,1,1,1,1,1,1,1,1,1,1,1,1,1,1,1,1,1,1,1,1,1,1,1,1,1,1,1,1,
1,1,1,1,1,1,1,1,1,1,1,1,1,1,1,1,1,1,1,1,1,1,1,1,1,1,1,1,1,1,1,1,1,1,1,1,
1,1,1,1,1,1,1,1,1,1,1,1,1,1,1,1,1,1,1,1,1,1,1,1,1,1,1,1,1,1,1,1,1,1,1,1,
1,1,1,1,1,1,1,1,1,1,1,1,1,1,1,1,1,1,1,1,1,1,1,1,1,1,1,1,1,1,1,1,1,1,1,1,
1,1,1,1,1,1,1,1,1,1,1,1,1,1,1,1,1,1,1,1,1,1,1,1,1,1,1,1,1,1,1,1,1,1,1,1,
1,1,1,1,1,1,1,1,1,1,1,1,1,1,1,1,1,1,1,1,1,1,1,1,1,1,1,1,1,1,1,1,1,1,1,1,
1,1,1,1,1,1,1,1,1,1,1,1,1,1,1,1,1,1,1,1,1,1,1,1,1,1,1,1,1,1,1,1,1,1,1,1,
1,1,1,1,1,1,1,1,1,1,1,1,1,1,1,1,1,1,1,1,1,1,1,1,1,1,1,1,1,1,1,1,1,1,1,1,
1,4),(0.,0.23619826056056),(12.0433050839651,12.5431859047334,13.0430667255018,
14.0428283670385,15.0425900085752,16.0423516501119,17.0421132916487,18.0418749331854,
18.5417557539537,19.0416365747221,20.0413982162588,21.0411598577955,22.0409214993322,
23.040683140869,24.0404447824057,25.0402064239424,25.5400872447107,26.0399680654791,
27.0397297070158,28.0394913485525,29.0392529900893,30.039014631626,31.0387762731627,
32.0385379146994,32.5384187354678,33.0382995562361,34.0380611977728,35.0378228393096,
36.0375844808463,37.037346122383,38.0371077639197,39.0368694054564,39.5367502262248,
40.0366310469931,41.0363926885299,42.0361543300666,43.0359159716033,44.03567761314,
45.0354392546767,46.0352008962134,46.5350817169818,47.0349625377502,48.0347241792869,
49.0344858208236,50.0342474623603,51.034009103897,52.0337707454337,53.0335323869705,
53.5334132077388,54.0332940285072,55.0330556700439,56.0328173115806,57.0325789531173,
58.0323405946541,59.0321022361908,60.0318638777275,60.5317446984958,61.0316255192642,
62.0313871608009,63.0311488023376,64.0309104438743,65.0306720854111,66.0304337269478,
67.0301953684845,67.5300761892529,68.0299570100212,69.0297186515579,70.0294802930947,
71.0292419346314,72.0290035761681,73.0287652177048,74.0285268592415,74.5284076800099,
75.0282885007782,76.028050142315,77.0278117838517,78.0275734253884,79.0273350669251,
80.0270967084618,81.0268583499985,81.5267391707669,82.0266199915352,83.026381633072,
84.0261432746087,85.0259049161454,86.0256665576821,87.0254281992188,88.0251898407555,
88.5250706615239,89.0249514822923,90.024713123829,91.0244747653657,92.0242364069024,
93.0239980484391,94.0237596899758,95.0235213315126,95.5234021522809,96.0232829730493,
97.023044614586,98.0228062561227,99.0225678976594,100.022329539196,101.022091180733,
102.02185282227,102.521733643038,103.021614463806,104.021376105343,105.02113774688,
106.020899388416,107.020661029953,108.02042267149,109.020184313027,109.520065133795,
110.019945954563,111.0197075961,112.019469237637,113.019230879173,114.01899252071,
115.018754162247,116.018515803784,116.518396624552,117.01827744532,118.018039086857,
119.017800728394,120.01756236993,121.017324011467,122.017085653004,123.016847294541,
123.516728115309,124.016608936077,125.016370577614,126.016132219151,127.015893860688,
128.015655502224,129.015417143761,130.015178785298,130.515059606066,131.014940426834,
132.014702068371,133.014463709908,134.014225351445,135.013986992981,136.013748634518,
137.013510276055,137.513391096823,138.013271917591,139.013033559128,140.012795200665,
141.012556842202,142.012318483738,143.012080125275,144.011841766812,144.51172258758,
145.011603408348,146.011365049885,147.011126691422,148.010888332959,149.010649974495,
150.010411616032,151.010173257569,151.510054078337,152.009934899105,153.009696540642,
154.009458182179,155.009219823716,156.008981465252,157.008743106789,158.008504748326,
158.508385569094,159.008266389862,160.008028031399,161.007789672936,162.007551314473,
163.007312956009,164.007074597546,165.006836239083,165.506717059851,166.006597880619,
167.006359522156,168.006121163693,169.00588280523,170.005644446766,171.005406088303,
172.00516772984,172.505048550608,173.004929371376,174.004691012913,175.00445265445,
176.004214295987,177.003975937523,178.00373757906,179.003499220597,179.503380041365,
180.003260862133,181.00302250367,182.002784145207,183.002545786744,184.00230742828,
185.002069069817,186.001830711354,186.501711532122,187.001592352891,188.001353994427,
189.001115635964,190.000877277501,191.000638919037,192.000400560574,193.000162202111,
193.500043022879,193.999923843648,194.999685485184,195.999447126721,196.999208768258,
197.998970409794,198.998732051331,199.998493692868,200.498374513636,200.998255334405,
201.998016975941,202.997778617478,203.997540259015,204.997301900551,205.997063542088,
206.996825183625,207.496706004393,207.996586825162,208.996348466698,209.996110108235,
210.995871749772,211.995633391308,212.995395032845,213.995156674382,214.49503749515,
214.994918315919,215.994679957455,216.994441598992,217.994203240529,218.993964882065,
219.993726523602,220.993488165139,221.493368985907,221.993249806676,222.993011448212,
223.992773089749,224.992534731286,225.992296372822,226.992058014359,227.991819655896,
228.491700476664,228.991581297433,229.991342938969,230.991104580506,231.990866222043,
232.99062786358,233.990389505116,234.990151146653,235.490031967421,235.98991278819,
236.989674429726,237.989436071263,238.9891977128,239.988959354337,240.988720995873,
241.98848263741,242.488363458178,242.988244278947,243.988005920483,244.98776756202,
245.987529203557,246.987290845094,247.98705248663,248.986814128167,249.486694948935,
249.986575769704,250.98633741124,251.986099052777,252.985860694314,253.985622335851,
254.985383977387,255.985145618924,256.485026439692,256.984907260461,257.984668901997,
258.984430543534,259.984192185071,260.983953826608,261.983715468144,262.983477109681,
263.483357930449,263.983238751218,264.983000392754,265.982762034291,266.982523675828,
267.982285317365,268.982046958901,269.981808600438,270.481689421206,270.981570241975,
271.981331883511,272.981093525048,273.980855166585,274.980616808122,275.980378449658,
276.980140091195,277.480020911963,277.979901732732,278.979663374269,279.979425015805,
280.979186657342,281.978948298879,282.978709940415,283.978471581952,284.47835240272,
284.978233223489,285.977994865025,286.977756506562,287.977518148099,288.977279789636,
289.977041431172,290.976803072709,291.476683893477,291.976564714246,292.976326355783,
293.976087997319,294.975849638856,295.975611280393,296.975372921929,297.975134563466,
298.475015384234,298.974896205003,299.97465784654,300.974419488076,301.974181129613,
302.97394277115,303.973704412686,304.973466054223,305.473346874992,305.97322769576,
306.972989337297,307.972750978833,308.97251262037,309.972274261907,310.972035903443,
311.97179754498,312.471678365749,312.971559186517,313.971320828054,314.97108246959,
315.970844111127,316.970605752664,317.9703673942,318.970129035737,319.470009856505,
319.969890677274,320.969652318811,321.969413960347,322.969175601884,323.968937243421,
324.968698884957,325.968460526494,326.468341347263,326.968222168031,327.967983809568,
328.967745451104,329.967507092641,330.967268734178,331.967030375715,332.966792017251,
333.966553658788,334.966315300325,335.466196121093,335.966076941861,336.965838583398,
337.965600224935,338.965361866472,339.965123508008,340.964885149545,341.964646791082,
342.46452761185,342.964408432618,343.964170074155,344.963931715692,345.963693357229,
346.963454998765,347.963216640302,348.962978281839,349.462859102607,349.962739923375,
350.962501564912,351.962263206449,352.962024847986,353.961786489522,354.961548131059,
355.961309772596,356.461190593364,356.961071414132,357.960833055669,358.960594697206,
359.960356338743,360.960117980279,361.959879621816,362.959641263353,363.459522084121,
363.959402904889,364.959164546426,365.958926187963,366.9586878295,367.958449471036,
368.958211112573,369.95797275411,370.457853574878,370.957734395646,371.957496037183,
372.95725767872,373.957019320257,374.956780961793,375.95654260333,376.956304244867,
377.456185065635,377.956065886403,378.95582752794,379.955589169477,380.955350811014,
381.95511245255,382.954874094087,383.954635735624,384.454516556392,384.95439737716,
385.954159018697,386.953920660234,387.953682301771,388.953443943307,389.953205584844,
390.952967226381,391.452848047149,391.952728867918,392.952490509454,393.952252150991,
394.952013792528,395.951775434064,396.951537075601,397.951298717138,398.451179537906,
398.951060358675,399.950822000211,400.950583641748,401.950345283285,402.950106924821,
403.949868566358,404.949630207895,405.449511028663,405.949391849432,406.949153490968,
407.948915132505,408.948676774042,409.948438415578,410.948200057115,411.947961698652,
412.44784251942,412.947723340189,413.947484981725,414.947246623262,415.947008264799,
416.946769906335,417.946531547872,418.946293189409,419.446174010177,419.946054830946,
420.945816472482,421.945578114019,422.945339755556,423.945101397092,424.944863038629,
425.944624680166,426.444505500934,426.944386321703,427.944147963239,428.943909604776,
429.943671246313,430.943432887849,431.943194529386,432.942956170923,433.442836991691,
433.94271781246,434.942479453996,435.942241095533,436.94200273707,437.941764378606,
438.941526020143,439.94128766168,440.441168482448,440.941049303217,441.940810944753,
442.94057258629,443.940334227827,444.940095869364,445.9398575109,446.939619152437,
447.439499973205,447.939380793974,448.93914243551,449.938904077047,450.938665718584,
451.93842736012,452.938189001657,453.937950643194,454.437831463962,454.937712284731,
455.937473926267,456.937235567804,457.936997209341,458.936758850878,459.936520492414,
460.936282133951,461.436162954719,461.936043775488,462.935805417024,463.935567058561,
464.935328700098,465.935090341635,466.934851983171,467.934613624708,468.434494445476,
468.934375266245,469.934136907781,470.933898549318,471.933660190855,472.933421832392,
473.933183473928,474.932945115465,475.432825936233,475.932706757002,476.932468398538,
477.932230040075,478.931991681612,479.931753323149,480.931514964685,481.931276606222,
482.43115742699,482.931038247759,483.930799889295,484.930561530832,485.930323172369,
486.930084813906,487.929846455442,488.929608096979,489.429488917747,489.929369738516,
490.929131380052,491.928893021589,492.928654663126,493.928416304663,494.928177946199,
495.927939587736,496.427820408504,496.927701229273,497.92746287081,498.927224512346,
499.926986153883,500.92674779542,501.926509436956,502.926271078493,503.426151899261,
503.92603272003,504.925794361566,505.925556003103,506.92531764464,507.925079286177,
508.924840927713,509.92460256925,510.424483390018,510.924364210787,511.924125852324,
512.92388749386,513.923649135397,514.923410776934,515.92317241847,516.922934060007,
517.422814880775,517.922695701544,518.922457343081,519.922218984617,520.921980626154,
521.921742267691,522.921503909227,523.921265550764,524.421146371532,524.921027192301,
525.920788833837,526.920550475374,527.920312116911,528.920073758448,529.919835399984,
530.919597041521,531.419477862289,531.919358683058,532.919120324594,533.918881966131,
534.918643607668,535.918405249205,536.918166890741,537.917928532278,538.417809353046,
538.917690173815,539.917451815352,540.917213456888,541.916975098425,542.916736739962,
543.916498381498,544.916260023035,545.416140843804,545.916021664572,546.915783306109,
547.915544947645,548.915306589182,549.915068230719,550.914829872255,551.914591513792,
552.414472334561,552.914353155329,553.914114796866,554.913876438402,555.913638079939,
556.913399721476,557.913161363012,558.912923004549,559.412803825317,559.912684646086,
560.912446287623,561.912207929159,562.911969570696,563.911731212233,564.911492853769,
565.911254495306,566.411135316074,566.911016136843,567.91077777838,568.910539419916,
569.910301061453,570.91006270299,571.909824344526,572.909585986063,573.409466806832,
573.9093476276,574.909109269137,575.908870910673,576.90863255221,577.908394193747,
578.908155835284,579.90791747682,580.407798297589,580.907679118357,581.907440759894,
582.90720240143,583.906964042967,584.906725684504,585.906487326041,586.906248967577,
587.406129788346,587.906010609114,588.905772250651,589.905533892187,590.905295533724,
591.905057175261,592.904818816798,593.904580458334,594.404461279103,594.904342099871,
595.904103741408,596.903865382944,597.903627024481,598.903388666018,599.903150307555,
600.902911949091,601.40279276986,601.902673590628,602.902435232165,603.902196873701,
604.901958515238,605.901720156775,606.901481798312,607.901243439848,608.401124260617,
608.901005081385,609.900766722922,610.900528364458,611.900290005995,612.900051647532,
613.899813289069,614.899574930605,615.399455751374,615.899336572142,616.899098213679,
617.898859855216,618.898621496752,619.898383138289,620.898144779826,621.897906421362,
622.397787242131,622.897668062899,623.897429704436,624.897191345972,625.896952987509,
626.896714629046,627.896476270583,628.896237912119,629.396118732888,629.895999553656,
630.895761195193,631.895522836729,632.895284478266,633.895046119803,634.89480776134,
635.894569402876,636.394450223645,636.894331044413,637.89409268595,638.893854327487,
639.893615969023,640.89337761056,641.893139252097,642.393020072865,642.892900893633),
 .UNSPECIFIED.);
#68=B_SPLINE_SURFACE_WITH_KNOTS('',3,3,((#43587,#43588,#43589,#43590,#43591,
#43592,#43593,#43594,#43595,#43596,#43597,#43598,#43599,#43600,#43601,#43602,
#43603,#43604,#43605,#43606,#43607,#43608,#43609,#43610,#43611,#43612,#43613,
#43614,#43615,#43616,#43617,#43618,#43619,#43620,#43621,#43622,#43623,#43624,
#43625,#43626,#43627,#43628,#43629,#43630,#43631,#43632,#43633,#43634,#43635,
#43636,#43637,#43638,#43639,#43640,#43641,#43642,#43643,#43644,#43645,#43646,
#43647,#43648,#43649,#43650,#43651,#43652,#43653,#43654,#43655,#43656,#43657,
#43658,#43659,#43660,#43661,#43662,#43663,#43664,#43665,#43666,#43667,#43668,
#43669,#43670,#43671,#43672,#43673,#43674,#43675,#43676,#43677,#43678,#43679,
#43680,#43681,#43682,#43683,#43684,#43685,#43686,#43687,#43688,#43689,#43690,
#43691,#43692,#43693,#43694,#43695,#43696,#43697,#43698,#43699,#43700,#43701,
#43702,#43703,#43704,#43705,#43706,#43707,#43708,#43709,#43710,#43711,#43712,
#43713),(#43714,#43715,#43716,#43717,#43718,#43719,#43720,#43721,#43722,
#43723,#43724,#43725,#43726,#43727,#43728,#43729,#43730,#43731,#43732,#43733,
#43734,#43735,#43736,#43737,#43738,#43739,#43740,#43741,#43742,#43743,#43744,
#43745,#43746,#43747,#43748,#43749,#43750,#43751,#43752,#43753,#43754,#43755,
#43756,#43757,#43758,#43759,#43760,#43761,#43762,#43763,#43764,#43765,#43766,
#43767,#43768,#43769,#43770,#43771,#43772,#43773,#43774,#43775,#43776,#43777,
#43778,#43779,#43780,#43781,#43782,#43783,#43784,#43785,#43786,#43787,#43788,
#43789,#43790,#43791,#43792,#43793,#43794,#43795,#43796,#43797,#43798,#43799,
#43800,#43801,#43802,#43803,#43804,#43805,#43806,#43807,#43808,#43809,#43810,
#43811,#43812,#43813,#43814,#43815,#43816,#43817,#43818,#43819,#43820,#43821,
#43822,#43823,#43824,#43825,#43826,#43827,#43828,#43829,#43830,#43831,#43832,
#43833,#43834,#43835,#43836,#43837,#43838,#43839,#43840),(#43841,#43842,
#43843,#43844,#43845,#43846,#43847,#43848,#43849,#43850,#43851,#43852,#43853,
#43854,#43855,#43856,#43857,#43858,#43859,#43860,#43861,#43862,#43863,#43864,
#43865,#43866,#43867,#43868,#43869,#43870,#43871,#43872,#43873,#43874,#43875,
#43876,#43877,#43878,#43879,#43880,#43881,#43882,#43883,#43884,#43885,#43886,
#43887,#43888,#43889,#43890,#43891,#43892,#43893,#43894,#43895,#43896,#43897,
#43898,#43899,#43900,#43901,#43902,#43903,#43904,#43905,#43906,#43907,#43908,
#43909,#43910,#43911,#43912,#43913,#43914,#43915,#43916,#43917,#43918,#43919,
#43920,#43921,#43922,#43923,#43924,#43925,#43926,#43927,#43928,#43929,#43930,
#43931,#43932,#43933,#43934,#43935,#43936,#43937,#43938,#43939,#43940,#43941,
#43942,#43943,#43944,#43945,#43946,#43947,#43948,#43949,#43950,#43951,#43952,
#43953,#43954,#43955,#43956,#43957,#43958,#43959,#43960,#43961,#43962,#43963,
#43964,#43965,#43966,#43967),(#43968,#43969,#43970,#43971,#43972,#43973,
#43974,#43975,#43976,#43977,#43978,#43979,#43980,#43981,#43982,#43983,#43984,
#43985,#43986,#43987,#43988,#43989,#43990,#43991,#43992,#43993,#43994,#43995,
#43996,#43997,#43998,#43999,#44000,#44001,#44002,#44003,#44004,#44005,#44006,
#44007,#44008,#44009,#44010,#44011,#44012,#44013,#44014,#44015,#44016,#44017,
#44018,#44019,#44020,#44021,#44022,#44023,#44024,#44025,#44026,#44027,#44028,
#44029,#44030,#44031,#44032,#44033,#44034,#44035,#44036,#44037,#44038,#44039,
#44040,#44041,#44042,#44043,#44044,#44045,#44046,#44047,#44048,#44049,#44050,
#44051,#44052,#44053,#44054,#44055,#44056,#44057,#44058,#44059,#44060,#44061,
#44062,#44063,#44064,#44065,#44066,#44067,#44068,#44069,#44070,#44071,#44072,
#44073,#44074,#44075,#44076,#44077,#44078,#44079,#44080,#44081,#44082,#44083,
#44084,#44085,#44086,#44087,#44088,#44089,#44090,#44091,#44092,#44093,#44094)),
 .UNSPECIFIED.,.F.,.F.,.F.,(4,4),(4,1,1,1,1,1,1,1,1,1,1,1,1,1,1,1,1,1,1,
1,1,1,1,1,1,1,1,1,1,1,1,1,1,1,1,1,1,1,1,1,1,1,1,1,1,1,1,1,1,1,1,1,1,1,1,
1,1,1,1,1,1,1,1,1,1,1,1,1,1,1,1,1,1,1,1,1,1,1,1,1,1,1,1,1,1,1,1,1,1,1,1,
1,1,1,1,1,1,1,1,1,1,1,1,1,1,1,1,1,1,1,1,1,1,1,1,1,1,1,1,1,1,1,1,1,4),(-0.0117202104645729,
2.30765714068266E-14),(13.9661186601203,14.4600465471847,14.9539744342492,
15.4479023213137,15.9418302083782,16.4357580954427,16.9296859825072,17.4236138695716,
17.9175417566361,18.4114696437006,18.9053975307651,19.3993254178296,19.893253304894,
20.3871811919585,20.881109079023,21.3750369660875,21.868964853152,22.3628927402165,
22.8568206272809,23.3507485143454,23.8446764014099,24.3386042884744,24.8325321755389,
25.3264600626033,25.8203879496678,26.3143158367323,26.8082437237968,27.3021716108613,
27.7960994979258,28.2900273849902,28.7839552720547,29.2778831591192,29.7718110461837,
30.2657389332482,30.7596668203126,31.2535947073771,31.7475225944416,32.2414504815061,
32.7353783685706,33.2293062556351,33.7232341426995,34.217162029764,34.7110899168285,
35.205017803893,35.6989456909575,36.1928735780219,36.6868014650864,37.1807293521509,
37.6746572392154,38.1685851262799,38.6625130133444,39.1564409004088,39.6503687874733,
40.1442966745378,40.6382245616023,41.1321524486668,41.6260803357312,42.1200082227957,
42.6139361098602,43.1078639969247,43.6017918839892,44.0957197710537,44.5896476581181,
45.0835755451826,45.5775034322471,46.0714313193116,46.5653592063761,47.0592870934405,
47.553214980505,48.0471428675695,48.541070754634,49.0349986416985,49.528926528763,
50.0228544158274,50.5167823028919,51.0107101899564,51.5046380770209,51.9985659640854,
52.4924938511499,52.9864217382143,53.4803496252788,53.9742775123433,54.4682053994078,
54.9621332864723,55.4560611735367,55.9499890606012,56.4439169476657,56.9378448347302,
57.4317727217947,57.9257006088591,58.4196284959236,58.9135563829881,59.4074842700526,
59.9014121571171,60.3953400441816,60.889267931246,61.3831958183105,61.877123705375,
62.3710515924395,62.864979479504,63.3589073665685,63.8528352536329,64.3467631406974,
64.8406910277619,65.3346189148264,65.8285468018909,66.3224746889554,66.8164025760198,
67.3103304630843,67.8042583501488,68.2981862372133,68.7921141242778,69.2860420113422,
69.7799698984067,70.2738977854712,70.7678256725357,71.2617535596002,71.7556814466647,
72.2496093337291,72.7435372207936,73.2374651078581,73.7313929949226,74.2253208819871,
74.7192487690515,75.213176656116),.UNSPECIFIED.);
#69=B_SPLINE_SURFACE_WITH_KNOTS('',3,3,((#44151,#44152,#44153,#44154,#44155,
#44156,#44157,#44158,#44159,#44160,#44161,#44162,#44163,#44164,#44165,#44166,
#44167,#44168,#44169,#44170,#44171,#44172,#44173,#44174,#44175,#44176,#44177,
#44178,#44179,#44180,#44181,#44182,#44183,#44184,#44185,#44186,#44187,#44188,
#44189,#44190,#44191,#44192,#44193,#44194,#44195,#44196,#44197,#44198,#44199,
#44200,#44201,#44202,#44203,#44204,#44205,#44206,#44207,#44208,#44209,#44210,
#44211,#44212,#44213,#44214,#44215,#44216,#44217,#44218,#44219,#44220,#44221,
#44222,#44223,#44224,#44225,#44226,#44227,#44228,#44229,#44230,#44231,#44232,
#44233,#44234,#44235,#44236,#44237,#44238,#44239,#44240,#44241,#44242,#44243,
#44244,#44245,#44246,#44247,#44248,#44249,#44250,#44251,#44252,#44253,#44254,
#44255,#44256,#44257,#44258,#44259,#44260,#44261,#44262,#44263,#44264,#44265,
#44266,#44267,#44268,#44269,#44270,#44271,#44272,#44273,#44274,#44275,#44276,
#44277),(#44278,#44279,#44280,#44281,#44282,#44283,#44284,#44285,#44286,
#44287,#44288,#44289,#44290,#44291,#44292,#44293,#44294,#44295,#44296,#44297,
#44298,#44299,#44300,#44301,#44302,#44303,#44304,#44305,#44306,#44307,#44308,
#44309,#44310,#44311,#44312,#44313,#44314,#44315,#44316,#44317,#44318,#44319,
#44320,#44321,#44322,#44323,#44324,#44325,#44326,#44327,#44328,#44329,#44330,
#44331,#44332,#44333,#44334,#44335,#44336,#44337,#44338,#44339,#44340,#44341,
#44342,#44343,#44344,#44345,#44346,#44347,#44348,#44349,#44350,#44351,#44352,
#44353,#44354,#44355,#44356,#44357,#44358,#44359,#44360,#44361,#44362,#44363,
#44364,#44365,#44366,#44367,#44368,#44369,#44370,#44371,#44372,#44373,#44374,
#44375,#44376,#44377,#44378,#44379,#44380,#44381,#44382,#44383,#44384,#44385,
#44386,#44387,#44388,#44389,#44390,#44391,#44392,#44393,#44394,#44395,#44396,
#44397,#44398,#44399,#44400,#44401,#44402,#44403,#44404),(#44405,#44406,
#44407,#44408,#44409,#44410,#44411,#44412,#44413,#44414,#44415,#44416,#44417,
#44418,#44419,#44420,#44421,#44422,#44423,#44424,#44425,#44426,#44427,#44428,
#44429,#44430,#44431,#44432,#44433,#44434,#44435,#44436,#44437,#44438,#44439,
#44440,#44441,#44442,#44443,#44444,#44445,#44446,#44447,#44448,#44449,#44450,
#44451,#44452,#44453,#44454,#44455,#44456,#44457,#44458,#44459,#44460,#44461,
#44462,#44463,#44464,#44465,#44466,#44467,#44468,#44469,#44470,#44471,#44472,
#44473,#44474,#44475,#44476,#44477,#44478,#44479,#44480,#44481,#44482,#44483,
#44484,#44485,#44486,#44487,#44488,#44489,#44490,#44491,#44492,#44493,#44494,
#44495,#44496,#44497,#44498,#44499,#44500,#44501,#44502,#44503,#44504,#44505,
#44506,#44507,#44508,#44509,#44510,#44511,#44512,#44513,#44514,#44515,#44516,
#44517,#44518,#44519,#44520,#44521,#44522,#44523,#44524,#44525,#44526,#44527,
#44528,#44529,#44530,#44531),(#44532,#44533,#44534,#44535,#44536,#44537,
#44538,#44539,#44540,#44541,#44542,#44543,#44544,#44545,#44546,#44547,#44548,
#44549,#44550,#44551,#44552,#44553,#44554,#44555,#44556,#44557,#44558,#44559,
#44560,#44561,#44562,#44563,#44564,#44565,#44566,#44567,#44568,#44569,#44570,
#44571,#44572,#44573,#44574,#44575,#44576,#44577,#44578,#44579,#44580,#44581,
#44582,#44583,#44584,#44585,#44586,#44587,#44588,#44589,#44590,#44591,#44592,
#44593,#44594,#44595,#44596,#44597,#44598,#44599,#44600,#44601,#44602,#44603,
#44604,#44605,#44606,#44607,#44608,#44609,#44610,#44611,#44612,#44613,#44614,
#44615,#44616,#44617,#44618,#44619,#44620,#44621,#44622,#44623,#44624,#44625,
#44626,#44627,#44628,#44629,#44630,#44631,#44632,#44633,#44634,#44635,#44636,
#44637,#44638,#44639,#44640,#44641,#44642,#44643,#44644,#44645,#44646,#44647,
#44648,#44649,#44650,#44651,#44652,#44653,#44654,#44655,#44656,#44657,#44658)),
 .UNSPECIFIED.,.F.,.F.,.F.,(4,4),(4,1,1,1,1,1,1,1,1,1,1,1,1,1,1,1,1,1,1,
1,1,1,1,1,1,1,1,1,1,1,1,1,1,1,1,1,1,1,1,1,1,1,1,1,1,1,1,1,1,1,1,1,1,1,1,
1,1,1,1,1,1,1,1,1,1,1,1,1,1,1,1,1,1,1,1,1,1,1,1,1,1,1,1,1,1,1,1,1,1,1,1,
1,1,1,1,1,1,1,1,1,1,1,1,1,1,1,1,1,1,1,1,1,1,1,1,1,1,1,1,1,1,1,1,1,4),(0.115296848757141,
0.127017059221739),(14.9954123969612,15.4893404554446,15.9832685139281,
16.4771965724115,16.9711246308949,17.4650526893783,17.9589807478618,18.4529088063452,
18.9468368648286,19.440764923312,19.9346929817954,20.4286210402789,20.9225490987623,
21.4164771572457,21.9104052157291,22.4043332742125,22.898261332696,23.3921893911794,
23.8861174496628,24.3800455081462,24.8739735666297,25.3679016251131,25.8618296835965,
26.3557577420799,26.8496858005633,27.3436138590468,27.8375419175302,28.3314699760136,
28.825398034497,29.3193260929804,29.8132541514639,30.3071822099473,30.8011102684307,
31.2950383269141,31.7889663853976,32.282894443881,32.7768225023644,33.2707505608478,
33.7646786193312,34.2586066778147,34.7525347362981,35.2464627947815,35.7403908532649,
36.2343189117483,36.7282469702318,37.2221750287152,37.7161030871986,38.210031145682,
38.7039592041655,39.1978872626489,39.6918153211323,40.1857433796157,40.6796714380991,
41.1735994965826,41.667527555066,42.1614556135494,42.6553836720328,43.1493117305162,
43.6432397889997,44.1371678474831,44.6310959059665,45.1250239644499,45.6189520229333,
46.1128800814168,46.6068081399002,47.1007361983836,47.594664256867,48.0885923153505,
48.5825203738339,49.0764484323173,49.5703764908007,50.0643045492841,50.5582326077676,
51.052160666251,51.5460887247344,52.0400167832178,52.5339448417012,53.0278729001847,
53.5218009586681,54.0157290171515,54.5096570756349,55.0035851341184,55.4975131926018,
55.9914412510852,56.4853693095686,56.979297368052,57.4732254265355,57.9671534850189,
58.4610815435023,58.9550096019857,59.4489376604691,59.9428657189526,60.436793777436,
60.9307218359194,61.4246498944028,61.9185779528863,62.4125060113697,62.9064340698531,
63.4003621283365,63.8942901868199,64.3882182453034,64.8821463037868,65.3760743622702,
65.8700024207536,66.363930479237,66.8578585377205,67.3517865962039,67.8457146546873,
68.3396427131707,68.8335707716542,69.3274988301376,69.821426888621,70.3153549471044,
70.8092830055878,71.3032110640713,71.7971391225547,72.2910671810381,72.7849952395215,
73.2789232980049,73.7728513564884,74.2667794149718,74.7607074734552,75.2546355319386,
75.748563590422,76.2424916489055),.UNSPECIFIED.);
#70=B_SPLINE_SURFACE_WITH_KNOTS('',3,3,((#44719,#44720,#44721,#44722,#44723,
#44724,#44725,#44726,#44727,#44728,#44729,#44730,#44731,#44732,#44733,#44734,
#44735,#44736,#44737,#44738,#44739,#44740,#44741,#44742,#44743,#44744,#44745,
#44746,#44747,#44748,#44749,#44750,#44751,#44752,#44753,#44754,#44755,#44756,
#44757,#44758,#44759,#44760,#44761,#44762,#44763,#44764,#44765,#44766,#44767,
#44768,#44769,#44770,#44771,#44772,#44773,#44774,#44775,#44776,#44777,#44778,
#44779,#44780,#44781,#44782,#44783,#44784,#44785,#44786,#44787,#44788,#44789,
#44790,#44791,#44792,#44793,#44794,#44795,#44796,#44797,#44798,#44799,#44800,
#44801,#44802,#44803,#44804,#44805,#44806,#44807,#44808,#44809,#44810,#44811,
#44812,#44813,#44814,#44815,#44816,#44817,#44818,#44819,#44820,#44821,#44822,
#44823,#44824,#44825,#44826,#44827,#44828,#44829,#44830,#44831,#44832,#44833,
#44834,#44835,#44836,#44837,#44838,#44839,#44840,#44841,#44842,#44843,#44844,
#44845,#44846,#44847,#44848,#44849,#44850,#44851,#44852,#44853,#44854,#44855,
#44856,#44857,#44858,#44859,#44860,#44861,#44862,#44863,#44864,#44865,#44866,
#44867,#44868,#44869,#44870,#44871,#44872,#44873,#44874,#44875,#44876,#44877,
#44878,#44879,#44880,#44881,#44882,#44883,#44884,#44885,#44886,#44887,#44888,
#44889,#44890,#44891,#44892,#44893,#44894,#44895,#44896,#44897,#44898,#44899,
#44900,#44901,#44902,#44903,#44904,#44905,#44906,#44907,#44908,#44909,#44910,
#44911,#44912,#44913,#44914,#44915,#44916,#44917,#44918,#44919,#44920,#44921,
#44922,#44923,#44924,#44925,#44926,#44927,#44928,#44929,#44930,#44931,#44932,
#44933,#44934,#44935,#44936,#44937,#44938,#44939,#44940,#44941,#44942,#44943,
#44944,#44945,#44946,#44947,#44948,#44949,#44950,#44951,#44952,#44953,#44954,
#44955,#44956,#44957,#44958,#44959,#44960,#44961,#44962,#44963,#44964,#44965,
#44966,#44967,#44968,#44969,#44970,#44971,#44972,#44973,#44974,#44975,#44976,
#44977,#44978,#44979,#44980,#44981,#44982,#44983,#44984,#44985,#44986,#44987,
#44988,#44989,#44990,#44991,#44992,#44993,#44994,#44995,#44996,#44997,#44998,
#44999,#45000,#45001,#45002,#45003,#45004,#45005,#45006,#45007,#45008,#45009,
#45010,#45011,#45012,#45013,#45014,#45015,#45016,#45017,#45018,#45019,#45020,
#45021,#45022,#45023,#45024,#45025,#45026,#45027,#45028,#45029,#45030,#45031,
#45032,#45033,#45034,#45035,#45036,#45037,#45038,#45039,#45040,#45041,#45042,
#45043,#45044,#45045,#45046,#45047,#45048,#45049,#45050,#45051,#45052,#45053,
#45054,#45055,#45056,#45057,#45058,#45059,#45060,#45061,#45062,#45063,#45064,
#45065,#45066,#45067,#45068,#45069,#45070,#45071,#45072,#45073,#45074,#45075,
#45076,#45077,#45078,#45079,#45080,#45081,#45082,#45083,#45084,#45085,#45086,
#45087,#45088,#45089,#45090,#45091,#45092,#45093,#45094,#45095,#45096,#45097,
#45098,#45099,#45100,#45101,#45102,#45103,#45104,#45105,#45106,#45107,#45108,
#45109,#45110,#45111,#45112,#45113,#45114,#45115,#45116,#45117,#45118,#45119,
#45120,#45121,#45122,#45123,#45124,#45125,#45126,#45127,#45128,#45129,#45130,
#45131,#45132,#45133,#45134,#45135,#45136,#45137,#45138,#45139,#45140,#45141,
#45142,#45143,#45144,#45145,#45146,#45147,#45148,#45149,#45150,#45151,#45152,
#45153,#45154,#45155,#45156,#45157,#45158,#45159,#45160,#45161,#45162,#45163,
#45164,#45165,#45166,#45167,#45168,#45169,#45170,#45171,#45172,#45173,#45174,
#45175,#45176,#45177,#45178,#45179,#45180,#45181,#45182,#45183,#45184,#45185,
#45186,#45187,#45188,#45189,#45190,#45191,#45192,#45193,#45194,#45195,#45196,
#45197,#45198,#45199,#45200,#45201,#45202,#45203,#45204,#45205,#45206,#45207,
#45208,#45209,#45210,#45211,#45212,#45213,#45214,#45215,#45216,#45217,#45218,
#45219,#45220,#45221,#45222,#45223,#45224,#45225,#45226,#45227,#45228,#45229,
#45230,#45231,#45232,#45233,#45234,#45235,#45236,#45237,#45238,#45239,#45240,
#45241,#45242,#45243,#45244,#45245,#45246,#45247,#45248,#45249,#45250,#45251,
#45252,#45253,#45254,#45255,#45256,#45257,#45258,#45259,#45260,#45261,#45262,
#45263,#45264,#45265,#45266,#45267,#45268,#45269,#45270,#45271,#45272,#45273,
#45274,#45275,#45276,#45277,#45278,#45279,#45280,#45281,#45282,#45283,#45284,
#45285,#45286,#45287,#45288,#45289,#45290,#45291,#45292,#45293,#45294,#45295,
#45296,#45297,#45298,#45299,#45300,#45301,#45302,#45303,#45304,#45305,#45306,
#45307,#45308,#45309,#45310,#45311,#45312,#45313,#45314,#45315,#45316,#45317,
#45318,#45319,#45320,#45321,#45322,#45323,#45324,#45325,#45326,#45327,#45328,
#45329,#45330,#45331,#45332,#45333,#45334,#45335,#45336,#45337,#45338,#45339,
#45340,#45341,#45342,#45343,#45344,#45345,#45346,#45347,#45348,#45349,#45350,
#45351,#45352,#45353,#45354,#45355,#45356,#45357,#45358,#45359,#45360,#45361,
#45362,#45363,#45364,#45365,#45366,#45367,#45368,#45369,#45370,#45371,#45372,
#45373,#45374,#45375,#45376,#45377,#45378,#45379,#45380,#45381,#45382,#45383,
#45384,#45385,#45386,#45387,#45388,#45389,#45390,#45391,#45392,#45393,#45394,
#45395,#45396,#45397,#45398,#45399,#45400,#45401,#45402,#45403,#45404,#45405,
#45406,#45407,#45408,#45409,#45410,#45411,#45412,#45413,#45414,#45415,#45416,
#45417,#45418,#45419,#45420,#45421,#45422,#45423,#45424,#45425,#45426,#45427,
#45428,#45429,#45430,#45431,#45432,#45433,#45434,#45435,#45436,#45437,#45438,
#45439,#45440,#45441,#45442,#45443),(#45444,#45445,#45446,#45447,#45448,
#45449,#45450,#45451,#45452,#45453,#45454,#45455,#45456,#45457,#45458,#45459,
#45460,#45461,#45462,#45463,#45464,#45465,#45466,#45467,#45468,#45469,#45470,
#45471,#45472,#45473,#45474,#45475,#45476,#45477,#45478,#45479,#45480,#45481,
#45482,#45483,#45484,#45485,#45486,#45487,#45488,#45489,#45490,#45491,#45492,
#45493,#45494,#45495,#45496,#45497,#45498,#45499,#45500,#45501,#45502,#45503,
#45504,#45505,#45506,#45507,#45508,#45509,#45510,#45511,#45512,#45513,#45514,
#45515,#45516,#45517,#45518,#45519,#45520,#45521,#45522,#45523,#45524,#45525,
#45526,#45527,#45528,#45529,#45530,#45531,#45532,#45533,#45534,#45535,#45536,
#45537,#45538,#45539,#45540,#45541,#45542,#45543,#45544,#45545,#45546,#45547,
#45548,#45549,#45550,#45551,#45552,#45553,#45554,#45555,#45556,#45557,#45558,
#45559,#45560,#45561,#45562,#45563,#45564,#45565,#45566,#45567,#45568,#45569,
#45570,#45571,#45572,#45573,#45574,#45575,#45576,#45577,#45578,#45579,#45580,
#45581,#45582,#45583,#45584,#45585,#45586,#45587,#45588,#45589,#45590,#45591,
#45592,#45593,#45594,#45595,#45596,#45597,#45598,#45599,#45600,#45601,#45602,
#45603,#45604,#45605,#45606,#45607,#45608,#45609,#45610,#45611,#45612,#45613,
#45614,#45615,#45616,#45617,#45618,#45619,#45620,#45621,#45622,#45623,#45624,
#45625,#45626,#45627,#45628,#45629,#45630,#45631,#45632,#45633,#45634,#45635,
#45636,#45637,#45638,#45639,#45640,#45641,#45642,#45643,#45644,#45645,#45646,
#45647,#45648,#45649,#45650,#45651,#45652,#45653,#45654,#45655,#45656,#45657,
#45658,#45659,#45660,#45661,#45662,#45663,#45664,#45665,#45666,#45667,#45668,
#45669,#45670,#45671,#45672,#45673,#45674,#45675,#45676,#45677,#45678,#45679,
#45680,#45681,#45682,#45683,#45684,#45685,#45686,#45687,#45688,#45689,#45690,
#45691,#45692,#45693,#45694,#45695,#45696,#45697,#45698,#45699,#45700,#45701,
#45702,#45703,#45704,#45705,#45706,#45707,#45708,#45709,#45710,#45711,#45712,
#45713,#45714,#45715,#45716,#45717,#45718,#45719,#45720,#45721,#45722,#45723,
#45724,#45725,#45726,#45727,#45728,#45729,#45730,#45731,#45732,#45733,#45734,
#45735,#45736,#45737,#45738,#45739,#45740,#45741,#45742,#45743,#45744,#45745,
#45746,#45747,#45748,#45749,#45750,#45751,#45752,#45753,#45754,#45755,#45756,
#45757,#45758,#45759,#45760,#45761,#45762,#45763,#45764,#45765,#45766,#45767,
#45768,#45769,#45770,#45771,#45772,#45773,#45774,#45775,#45776,#45777,#45778,
#45779,#45780,#45781,#45782,#45783,#45784,#45785,#45786,#45787,#45788,#45789,
#45790,#45791,#45792,#45793,#45794,#45795,#45796,#45797,#45798,#45799,#45800,
#45801,#45802,#45803,#45804,#45805,#45806,#45807,#45808,#45809,#45810,#45811,
#45812,#45813,#45814,#45815,#45816,#45817,#45818,#45819,#45820,#45821,#45822,
#45823,#45824,#45825,#45826,#45827,#45828,#45829,#45830,#45831,#45832,#45833,
#45834,#45835,#45836,#45837,#45838,#45839,#45840,#45841,#45842,#45843,#45844,
#45845,#45846,#45847,#45848,#45849,#45850,#45851,#45852,#45853,#45854,#45855,
#45856,#45857,#45858,#45859,#45860,#45861,#45862,#45863,#45864,#45865,#45866,
#45867,#45868,#45869,#45870,#45871,#45872,#45873,#45874,#45875,#45876,#45877,
#45878,#45879,#45880,#45881,#45882,#45883,#45884,#45885,#45886,#45887,#45888,
#45889,#45890,#45891,#45892,#45893,#45894,#45895,#45896,#45897,#45898,#45899,
#45900,#45901,#45902,#45903,#45904,#45905,#45906,#45907,#45908,#45909,#45910,
#45911,#45912,#45913,#45914,#45915,#45916,#45917,#45918,#45919,#45920,#45921,
#45922,#45923,#45924,#45925,#45926,#45927,#45928,#45929,#45930,#45931,#45932,
#45933,#45934,#45935,#45936,#45937,#45938,#45939,#45940,#45941,#45942,#45943,
#45944,#45945,#45946,#45947,#45948,#45949,#45950,#45951,#45952,#45953,#45954,
#45955,#45956,#45957,#45958,#45959,#45960,#45961,#45962,#45963,#45964,#45965,
#45966,#45967,#45968,#45969,#45970,#45971,#45972,#45973,#45974,#45975,#45976,
#45977,#45978,#45979,#45980,#45981,#45982,#45983,#45984,#45985,#45986,#45987,
#45988,#45989,#45990,#45991,#45992,#45993,#45994,#45995,#45996,#45997,#45998,
#45999,#46000,#46001,#46002,#46003,#46004,#46005,#46006,#46007,#46008,#46009,
#46010,#46011,#46012,#46013,#46014,#46015,#46016,#46017,#46018,#46019,#46020,
#46021,#46022,#46023,#46024,#46025,#46026,#46027,#46028,#46029,#46030,#46031,
#46032,#46033,#46034,#46035,#46036,#46037,#46038,#46039,#46040,#46041,#46042,
#46043,#46044,#46045,#46046,#46047,#46048,#46049,#46050,#46051,#46052,#46053,
#46054,#46055,#46056,#46057,#46058,#46059,#46060,#46061,#46062,#46063,#46064,
#46065,#46066,#46067,#46068,#46069,#46070,#46071,#46072,#46073,#46074,#46075,
#46076,#46077,#46078,#46079,#46080,#46081,#46082,#46083,#46084,#46085,#46086,
#46087,#46088,#46089,#46090,#46091,#46092,#46093,#46094,#46095,#46096,#46097,
#46098,#46099,#46100,#46101,#46102,#46103,#46104,#46105,#46106,#46107,#46108,
#46109,#46110,#46111,#46112,#46113,#46114,#46115,#46116,#46117,#46118,#46119,
#46120,#46121,#46122,#46123,#46124,#46125,#46126,#46127,#46128,#46129,#46130,
#46131,#46132,#46133,#46134,#46135,#46136,#46137,#46138,#46139,#46140,#46141,
#46142,#46143,#46144,#46145,#46146,#46147,#46148,#46149,#46150,#46151,#46152,
#46153,#46154,#46155,#46156,#46157,#46158,#46159,#46160,#46161,#46162,#46163,
#46164,#46165,#46166,#46167,#46168),(#46169,#46170,#46171,#46172,#46173,
#46174,#46175,#46176,#46177,#46178,#46179,#46180,#46181,#46182,#46183,#46184,
#46185,#46186,#46187,#46188,#46189,#46190,#46191,#46192,#46193,#46194,#46195,
#46196,#46197,#46198,#46199,#46200,#46201,#46202,#46203,#46204,#46205,#46206,
#46207,#46208,#46209,#46210,#46211,#46212,#46213,#46214,#46215,#46216,#46217,
#46218,#46219,#46220,#46221,#46222,#46223,#46224,#46225,#46226,#46227,#46228,
#46229,#46230,#46231,#46232,#46233,#46234,#46235,#46236,#46237,#46238,#46239,
#46240,#46241,#46242,#46243,#46244,#46245,#46246,#46247,#46248,#46249,#46250,
#46251,#46252,#46253,#46254,#46255,#46256,#46257,#46258,#46259,#46260,#46261,
#46262,#46263,#46264,#46265,#46266,#46267,#46268,#46269,#46270,#46271,#46272,
#46273,#46274,#46275,#46276,#46277,#46278,#46279,#46280,#46281,#46282,#46283,
#46284,#46285,#46286,#46287,#46288,#46289,#46290,#46291,#46292,#46293,#46294,
#46295,#46296,#46297,#46298,#46299,#46300,#46301,#46302,#46303,#46304,#46305,
#46306,#46307,#46308,#46309,#46310,#46311,#46312,#46313,#46314,#46315,#46316,
#46317,#46318,#46319,#46320,#46321,#46322,#46323,#46324,#46325,#46326,#46327,
#46328,#46329,#46330,#46331,#46332,#46333,#46334,#46335,#46336,#46337,#46338,
#46339,#46340,#46341,#46342,#46343,#46344,#46345,#46346,#46347,#46348,#46349,
#46350,#46351,#46352,#46353,#46354,#46355,#46356,#46357,#46358,#46359,#46360,
#46361,#46362,#46363,#46364,#46365,#46366,#46367,#46368,#46369,#46370,#46371,
#46372,#46373,#46374,#46375,#46376,#46377,#46378,#46379,#46380,#46381,#46382,
#46383,#46384,#46385,#46386,#46387,#46388,#46389,#46390,#46391,#46392,#46393,
#46394,#46395,#46396,#46397,#46398,#46399,#46400,#46401,#46402,#46403,#46404,
#46405,#46406,#46407,#46408,#46409,#46410,#46411,#46412,#46413,#46414,#46415,
#46416,#46417,#46418,#46419,#46420,#46421,#46422,#46423,#46424,#46425,#46426,
#46427,#46428,#46429,#46430,#46431,#46432,#46433,#46434,#46435,#46436,#46437,
#46438,#46439,#46440,#46441,#46442,#46443,#46444,#46445,#46446,#46447,#46448,
#46449,#46450,#46451,#46452,#46453,#46454,#46455,#46456,#46457,#46458,#46459,
#46460,#46461,#46462,#46463,#46464,#46465,#46466,#46467,#46468,#46469,#46470,
#46471,#46472,#46473,#46474,#46475,#46476,#46477,#46478,#46479,#46480,#46481,
#46482,#46483,#46484,#46485,#46486,#46487,#46488,#46489,#46490,#46491,#46492,
#46493,#46494,#46495,#46496,#46497,#46498,#46499,#46500,#46501,#46502,#46503,
#46504,#46505,#46506,#46507,#46508,#46509,#46510,#46511,#46512,#46513,#46514,
#46515,#46516,#46517,#46518,#46519,#46520,#46521,#46522,#46523,#46524,#46525,
#46526,#46527,#46528,#46529,#46530,#46531,#46532,#46533,#46534,#46535,#46536,
#46537,#46538,#46539,#46540,#46541,#46542,#46543,#46544,#46545,#46546,#46547,
#46548,#46549,#46550,#46551,#46552,#46553,#46554,#46555,#46556,#46557,#46558,
#46559,#46560,#46561,#46562,#46563,#46564,#46565,#46566,#46567,#46568,#46569,
#46570,#46571,#46572,#46573,#46574,#46575,#46576,#46577,#46578,#46579,#46580,
#46581,#46582,#46583,#46584,#46585,#46586,#46587,#46588,#46589,#46590,#46591,
#46592,#46593,#46594,#46595,#46596,#46597,#46598,#46599,#46600,#46601,#46602,
#46603,#46604,#46605,#46606,#46607,#46608,#46609,#46610,#46611,#46612,#46613,
#46614,#46615,#46616,#46617,#46618,#46619,#46620,#46621,#46622,#46623,#46624,
#46625,#46626,#46627,#46628,#46629,#46630,#46631,#46632,#46633,#46634,#46635,
#46636,#46637,#46638,#46639,#46640,#46641,#46642,#46643,#46644,#46645,#46646,
#46647,#46648,#46649,#46650,#46651,#46652,#46653,#46654,#46655,#46656,#46657,
#46658,#46659,#46660,#46661,#46662,#46663,#46664,#46665,#46666,#46667,#46668,
#46669,#46670,#46671,#46672,#46673,#46674,#46675,#46676,#46677,#46678,#46679,
#46680,#46681,#46682,#46683,#46684,#46685,#46686,#46687,#46688,#46689,#46690,
#46691,#46692,#46693,#46694,#46695,#46696,#46697,#46698,#46699,#46700,#46701,
#46702,#46703,#46704,#46705,#46706,#46707,#46708,#46709,#46710,#46711,#46712,
#46713,#46714,#46715,#46716,#46717,#46718,#46719,#46720,#46721,#46722,#46723,
#46724,#46725,#46726,#46727,#46728,#46729,#46730,#46731,#46732,#46733,#46734,
#46735,#46736,#46737,#46738,#46739,#46740,#46741,#46742,#46743,#46744,#46745,
#46746,#46747,#46748,#46749,#46750,#46751,#46752,#46753,#46754,#46755,#46756,
#46757,#46758,#46759,#46760,#46761,#46762,#46763,#46764,#46765,#46766,#46767,
#46768,#46769,#46770,#46771,#46772,#46773,#46774,#46775,#46776,#46777,#46778,
#46779,#46780,#46781,#46782,#46783,#46784,#46785,#46786,#46787,#46788,#46789,
#46790,#46791,#46792,#46793,#46794,#46795,#46796,#46797,#46798,#46799,#46800,
#46801,#46802,#46803,#46804,#46805,#46806,#46807,#46808,#46809,#46810,#46811,
#46812,#46813,#46814,#46815,#46816,#46817,#46818,#46819,#46820,#46821,#46822,
#46823,#46824,#46825,#46826,#46827,#46828,#46829,#46830,#46831,#46832,#46833,
#46834,#46835,#46836,#46837,#46838,#46839,#46840,#46841,#46842,#46843,#46844,
#46845,#46846,#46847,#46848,#46849,#46850,#46851,#46852,#46853,#46854,#46855,
#46856,#46857,#46858,#46859,#46860,#46861,#46862,#46863,#46864,#46865,#46866,
#46867,#46868,#46869,#46870,#46871,#46872,#46873,#46874,#46875,#46876,#46877,
#46878,#46879,#46880,#46881,#46882,#46883,#46884,#46885,#46886,#46887,#46888,
#46889,#46890,#46891,#46892,#46893),(#46894,#46895,#46896,#46897,#46898,
#46899,#46900,#46901,#46902,#46903,#46904,#46905,#46906,#46907,#46908,#46909,
#46910,#46911,#46912,#46913,#46914,#46915,#46916,#46917,#46918,#46919,#46920,
#46921,#46922,#46923,#46924,#46925,#46926,#46927,#46928,#46929,#46930,#46931,
#46932,#46933,#46934,#46935,#46936,#46937,#46938,#46939,#46940,#46941,#46942,
#46943,#46944,#46945,#46946,#46947,#46948,#46949,#46950,#46951,#46952,#46953,
#46954,#46955,#46956,#46957,#46958,#46959,#46960,#46961,#46962,#46963,#46964,
#46965,#46966,#46967,#46968,#46969,#46970,#46971,#46972,#46973,#46974,#46975,
#46976,#46977,#46978,#46979,#46980,#46981,#46982,#46983,#46984,#46985,#46986,
#46987,#46988,#46989,#46990,#46991,#46992,#46993,#46994,#46995,#46996,#46997,
#46998,#46999,#47000,#47001,#47002,#47003,#47004,#47005,#47006,#47007,#47008,
#47009,#47010,#47011,#47012,#47013,#47014,#47015,#47016,#47017,#47018,#47019,
#47020,#47021,#47022,#47023,#47024,#47025,#47026,#47027,#47028,#47029,#47030,
#47031,#47032,#47033,#47034,#47035,#47036,#47037,#47038,#47039,#47040,#47041,
#47042,#47043,#47044,#47045,#47046,#47047,#47048,#47049,#47050,#47051,#47052,
#47053,#47054,#47055,#47056,#47057,#47058,#47059,#47060,#47061,#47062,#47063,
#47064,#47065,#47066,#47067,#47068,#47069,#47070,#47071,#47072,#47073,#47074,
#47075,#47076,#47077,#47078,#47079,#47080,#47081,#47082,#47083,#47084,#47085,
#47086,#47087,#47088,#47089,#47090,#47091,#47092,#47093,#47094,#47095,#47096,
#47097,#47098,#47099,#47100,#47101,#47102,#47103,#47104,#47105,#47106,#47107,
#47108,#47109,#47110,#47111,#47112,#47113,#47114,#47115,#47116,#47117,#47118,
#47119,#47120,#47121,#47122,#47123,#47124,#47125,#47126,#47127,#47128,#47129,
#47130,#47131,#47132,#47133,#47134,#47135,#47136,#47137,#47138,#47139,#47140,
#47141,#47142,#47143,#47144,#47145,#47146,#47147,#47148,#47149,#47150,#47151,
#47152,#47153,#47154,#47155,#47156,#47157,#47158,#47159,#47160,#47161,#47162,
#47163,#47164,#47165,#47166,#47167,#47168,#47169,#47170,#47171,#47172,#47173,
#47174,#47175,#47176,#47177,#47178,#47179,#47180,#47181,#47182,#47183,#47184,
#47185,#47186,#47187,#47188,#47189,#47190,#47191,#47192,#47193,#47194,#47195,
#47196,#47197,#47198,#47199,#47200,#47201,#47202,#47203,#47204,#47205,#47206,
#47207,#47208,#47209,#47210,#47211,#47212,#47213,#47214,#47215,#47216,#47217,
#47218,#47219,#47220,#47221,#47222,#47223,#47224,#47225,#47226,#47227,#47228,
#47229,#47230,#47231,#47232,#47233,#47234,#47235,#47236,#47237,#47238,#47239,
#47240,#47241,#47242,#47243,#47244,#47245,#47246,#47247,#47248,#47249,#47250,
#47251,#47252,#47253,#47254,#47255,#47256,#47257,#47258,#47259,#47260,#47261,
#47262,#47263,#47264,#47265,#47266,#47267,#47268,#47269,#47270,#47271,#47272,
#47273,#47274,#47275,#47276,#47277,#47278,#47279,#47280,#47281,#47282,#47283,
#47284,#47285,#47286,#47287,#47288,#47289,#47290,#47291,#47292,#47293,#47294,
#47295,#47296,#47297,#47298,#47299,#47300,#47301,#47302,#47303,#47304,#47305,
#47306,#47307,#47308,#47309,#47310,#47311,#47312,#47313,#47314,#47315,#47316,
#47317,#47318,#47319,#47320,#47321,#47322,#47323,#47324,#47325,#47326,#47327,
#47328,#47329,#47330,#47331,#47332,#47333,#47334,#47335,#47336,#47337,#47338,
#47339,#47340,#47341,#47342,#47343,#47344,#47345,#47346,#47347,#47348,#47349,
#47350,#47351,#47352,#47353,#47354,#47355,#47356,#47357,#47358,#47359,#47360,
#47361,#47362,#47363,#47364,#47365,#47366,#47367,#47368,#47369,#47370,#47371,
#47372,#47373,#47374,#47375,#47376,#47377,#47378,#47379,#47380,#47381,#47382,
#47383,#47384,#47385,#47386,#47387,#47388,#47389,#47390,#47391,#47392,#47393,
#47394,#47395,#47396,#47397,#47398,#47399,#47400,#47401,#47402,#47403,#47404,
#47405,#47406,#47407,#47408,#47409,#47410,#47411,#47412,#47413,#47414,#47415,
#47416,#47417,#47418,#47419,#47420,#47421,#47422,#47423,#47424,#47425,#47426,
#47427,#47428,#47429,#47430,#47431,#47432,#47433,#47434,#47435,#47436,#47437,
#47438,#47439,#47440,#47441,#47442,#47443,#47444,#47445,#47446,#47447,#47448,
#47449,#47450,#47451,#47452,#47453,#47454,#47455,#47456,#47457,#47458,#47459,
#47460,#47461,#47462,#47463,#47464,#47465,#47466,#47467,#47468,#47469,#47470,
#47471,#47472,#47473,#47474,#47475,#47476,#47477,#47478,#47479,#47480,#47481,
#47482,#47483,#47484,#47485,#47486,#47487,#47488,#47489,#47490,#47491,#47492,
#47493,#47494,#47495,#47496,#47497,#47498,#47499,#47500,#47501,#47502,#47503,
#47504,#47505,#47506,#47507,#47508,#47509,#47510,#47511,#47512,#47513,#47514,
#47515,#47516,#47517,#47518,#47519,#47520,#47521,#47522,#47523,#47524,#47525,
#47526,#47527,#47528,#47529,#47530,#47531,#47532,#47533,#47534,#47535,#47536,
#47537,#47538,#47539,#47540,#47541,#47542,#47543,#47544,#47545,#47546,#47547,
#47548,#47549,#47550,#47551,#47552,#47553,#47554,#47555,#47556,#47557,#47558,
#47559,#47560,#47561,#47562,#47563,#47564,#47565,#47566,#47567,#47568,#47569,
#47570,#47571,#47572,#47573,#47574,#47575,#47576,#47577,#47578,#47579,#47580,
#47581,#47582,#47583,#47584,#47585,#47586,#47587,#47588,#47589,#47590,#47591,
#47592,#47593,#47594,#47595,#47596,#47597,#47598,#47599,#47600,#47601,#47602,
#47603,#47604,#47605,#47606,#47607,#47608,#47609,#47610,#47611,#47612,#47613,
#47614,#47615,#47616,#47617,#47618)),.UNSPECIFIED.,.F.,.F.,.F.,(4,4),(4,
1,1,1,1,1,1,1,1,1,1,1,1,1,1,1,1,1,1,1,1,1,1,1,1,1,1,1,1,1,1,1,1,1,1,1,1,
1,1,1,1,1,1,1,1,1,1,1,1,1,1,1,1,1,1,1,1,1,1,1,1,1,1,1,1,1,1,1,1,1,1,1,1,
1,1,1,1,1,1,1,1,1,1,1,1,1,1,1,1,1,1,1,1,1,1,1,1,1,1,1,1,1,1,1,1,1,1,1,1,
1,1,1,1,1,1,1,1,1,1,1,1,1,1,1,1,1,1,1,1,1,1,1,1,1,1,1,1,1,1,1,1,1,1,1,1,
1,1,1,1,1,1,1,1,1,1,1,1,1,1,1,1,1,1,1,1,1,1,1,1,1,1,1,1,1,1,1,1,1,1,1,1,
1,1,1,1,1,1,1,1,1,1,1,1,1,1,1,1,1,1,1,1,1,1,1,1,1,1,1,1,1,1,1,1,1,1,1,1,
1,1,1,1,1,1,1,1,1,1,1,1,1,1,1,1,1,1,1,1,1,1,1,1,1,1,1,1,1,1,1,1,1,1,1,1,
1,1,1,1,1,1,1,1,1,1,1,1,1,1,1,1,1,1,1,1,1,1,1,1,1,1,1,1,1,1,1,1,1,1,1,1,
1,1,1,1,1,1,1,1,1,1,1,1,1,1,1,1,1,1,1,1,1,1,1,1,1,1,1,1,1,1,1,1,1,1,1,1,
1,1,1,1,1,1,1,1,1,1,1,1,1,1,1,1,1,1,1,1,1,1,1,1,1,1,1,1,1,1,1,1,1,1,1,1,
1,1,1,1,1,1,1,1,1,1,1,1,1,1,1,1,1,1,1,1,1,1,1,1,1,1,1,1,1,1,1,1,1,1,1,1,
1,1,1,1,1,1,1,1,1,1,1,1,1,1,1,1,1,1,1,1,1,1,1,1,1,1,1,1,1,1,1,1,1,1,1,1,
1,1,1,1,1,1,1,1,1,1,1,1,1,1,1,1,1,1,1,1,1,1,1,1,1,1,1,1,1,1,1,1,1,1,1,1,
1,1,1,1,1,1,1,1,1,1,1,1,1,1,1,1,1,1,1,1,1,1,1,1,1,1,1,1,1,1,1,1,1,1,1,1,
1,1,1,1,1,1,1,1,1,1,1,1,1,1,1,1,1,1,1,1,1,1,1,1,1,1,1,1,1,1,1,1,1,1,1,1,
1,1,1,1,1,1,1,1,1,1,1,1,1,1,1,1,1,1,1,1,1,1,1,1,1,1,1,1,1,1,1,1,1,1,1,1,
1,1,1,1,1,1,1,1,1,1,1,1,1,1,1,1,1,1,1,1,1,1,1,1,1,1,1,1,1,1,1,1,1,1,1,1,
1,1,1,1,1,1,1,1,1,1,1,1,1,1,1,1,1,1,1,1,1,1,1,1,1,1,1,1,1,1,1,1,1,1,1,1,
1,1,1,1,1,1,1,1,1,1,1,1,1,1,1,1,1,1,1,1,1,1,1,1,1,1,1,1,1,1,1,1,1,1,1,1,
1,1,1,1,1,1,1,1,1,1,1,1,1,1,1,1,1,1,1,1,1,1,1,1,1,1,1,1,1,1,1,1,1,1,1,1,
1,4),(0.,0.23619826056056),(8.98757472625123,9.48745554701959,9.98733636778795,
10.9870980093247,11.9868596508614,12.9866212923981,13.9863829339348,14.9861445754715,
15.4860253962399,15.9859062170083,16.985667858545,17.9854295000817,18.9851911416184,
19.9849527831551,20.9847144246918,21.9844760662286,22.4843568869969,22.9842377077653,
23.983999349302,24.9837609908387,25.9835226323754,26.9832842739122,27.9830459154489,
28.9828075569856,29.4826883777539,29.9825691985223,30.982330840059,31.9820924815957,
32.9818541231325,33.9816157646692,34.9813774062059,35.9811390477426,36.481019868511,
36.9809006892793,37.980662330816,38.9804239723528,39.9801856138895,40.9799472554262,
41.9797088969629,42.9794705384996,43.479351359268,43.9792321800364,44.9789938215731,
45.9787554631098,46.9785171046465,47.9782787461832,48.9780403877199,49.9778020292567,
50.477682850025,50.9775636707934,51.9773253123301,52.9770869538668,53.9768485954035,
54.9766102369402,55.976371878477,56.9761335200137,57.476014340782,57.9758951615504,
58.9756568030871,59.9754184446238,60.9751800861606,61.9749417276973,62.974703369234,
63.9744650107707,64.4743458315391,64.9742266523074,65.9739882938441,66.9737499353809,
67.9735115769176,68.9732732184543,69.973034859991,70.9727965015277,71.4726773222961,
71.9725581430645,72.9723197846012,73.9720814261379,74.9718430676746,75.9716047092113,
76.971366350748,77.9711279922848,78.4710088130531,78.9708896338215,79.9706512753582,
80.9704129168949,81.9701745584316,82.9699361999684,83.9696978415051,84.9694594830418,
85.4693403038102,85.9692211245785,86.9689827661152,87.9687444076519,88.9685060491887,
89.9682676907254,90.9680293322621,91.9677909737988,92.4676717945672,92.9675526153355,
93.9673142568722,94.967075898409,95.9668375399457,96.9665991814824,97.9663608230191,
98.9661224645558,99.4660032853242,99.9658841060926,100.965645747629,101.965407389166,
102.965169030703,103.964930672239,104.964692313776,105.964453955313,106.464334776081,
106.96421559685,107.963977238386,108.963738879923,109.96350052146,110.963262162996,
111.963023804533,112.96278544607,113.462666266838,113.962547087607,114.962308729143,
115.96207037068,116.961832012217,117.961593653753,118.96135529529,119.961116936827,
120.460997757595,120.960878578364,121.9606402199,122.960401861437,123.960163502974,
124.95992514451,125.959686786047,126.959448427584,127.459329248352,127.959210069121,
128.958971710657,129.958733352194,130.958494993731,131.958256635268,132.958018276804,
133.957779918341,134.457660739109,134.957541559878,135.957303201414,136.957064842951,
137.956826484488,138.956588126025,139.956349767561,140.956111409098,141.455992229866,
141.955873050635,142.955634692171,143.955396333708,144.955157975245,145.954919616782,
146.954681258318,147.954442899855,148.454323720623,148.954204541392,149.953966182928,
150.953727824465,151.953489466002,152.953251107539,153.953012749075,154.952774390612,
155.45265521138,155.952536032149,156.952297673685,157.952059315222,158.951820956759,
159.951582598296,160.951344239832,161.951105881369,162.450986702137,162.950867522906,
163.950629164442,164.950390805979,165.950152447516,166.949914089053,167.949675730589,
168.949437372126,169.449318192894,169.949199013663,170.9489606552,171.948722296736,
172.948483938273,173.94824557981,174.948007221346,175.947768862883,176.447649683651,
176.94753050442,177.947292145957,178.947053787493,179.94681542903,180.946577070567,
181.946338712103,182.94610035364,183.445981174408,183.945861995177,184.945623636714,
185.94538527825,186.945146919787,187.944908561324,188.94467020286,189.944431844397,
190.444312665166,190.944193485934,191.943955127471,192.943716769007,193.943478410544,
194.943240052081,195.943001693617,196.942763335154,197.442644155923,197.942524976691,
198.942286618228,199.942048259764,200.941809901301,201.941571542838,202.941333184374,
203.941094825911,204.44097564668,204.940856467448,205.940618108985,206.940379750521,
207.940141392058,208.939903033595,209.939664675131,210.939426316668,211.439307137437,
211.939187958205,212.938949599742,213.938711241278,214.938472882815,215.938234524352,
216.937996165889,217.937757807425,218.437638628194,218.937519448962,219.937281090499,
220.937042732035,221.936804373572,222.936566015109,223.936327656646,224.936089298182,
225.435970118951,225.935850939719,226.935612581256,227.935374222792,228.935135864329,
229.934897505866,230.934659147403,231.934420788939,232.434301609708,232.934182430476,
233.933944072013,234.933705713549,235.933467355086,236.933228996623,237.93299063816,
238.932752279696,239.432633100465,239.932513921233,240.93227556277,241.932037204306,
242.931798845843,243.93156048738,244.931322128917,245.931083770453,246.430964591222,
246.93084541199,247.930607053527,248.930368695063,249.9301303366,250.929891978137,
251.929653619674,252.92941526121,253.429296081979,253.929176902747,254.928938544284,
255.928700185821,256.928461827357,257.928223468894,258.927985110431,259.927746751967,
260.427627572736,260.927508393504,261.927270035041,262.927031676578,263.926793318114,
264.926554959651,265.926316601188,266.926078242724,267.425959063493,267.925839884261,
268.925601525798,269.925363167335,270.925124808871,271.924886450408,272.924648091945,
273.924409733481,274.42429055425,274.924171375018,275.923933016555,276.923694658092,
277.923456299628,278.923217941165,279.922979582702,280.922741224238,281.422622045007,
281.922502865775,282.922264507312,283.922026148849,284.921787790385,285.921549431922,
286.921311073459,287.921072714995,288.420953535764,288.920834356532,289.920595998069,
290.920357639606,291.920119281142,292.919880922679,293.919642564216,294.919404205753,
295.419285026521,295.919165847289,296.918927488826,297.918689130363,298.918450771899,
299.918212413436,300.917974054973,301.91773569651,302.417616517278,302.917497338046,
303.917258979583,304.91702062112,305.916782262656,306.916543904193,307.91630554573,
308.916067187267,309.415948008035,309.915828828803,310.91559047034,311.915352111877,
312.915113753413,313.91487539495,314.914637036487,315.914398678024,316.414279498792,
316.91416031956,317.913921961097,318.913683602634,319.91344524417,320.913206885707,
321.912968527244,322.912730168781,323.412610989549,323.912491810317,324.912253451854,
325.912015093391,326.911776734928,327.911538376464,328.911300018001,329.911061659538,
330.910823301074,331.910584942611,332.410465763379,332.910346584148,333.910108225684,
334.909869867221,335.909631508758,336.909393150295,337.909154791831,338.908916433368,
339.408797254136,339.908678074905,340.908439716442,341.908201357978,342.907962999515,
343.907724641052,344.907486282588,345.907247924125,346.407128744893,346.907009565662,
347.906771207199,348.906532848735,349.906294490272,350.906056131809,351.905817773345,
352.905579414882,353.40546023565,353.905341056419,354.905102697956,355.904864339492,
356.904625981029,357.904387622566,358.904149264102,359.903910905639,360.403791726408,
360.903672547176,361.903434188713,362.903195830249,363.902957471786,364.902719113323,
365.902480754859,366.902242396396,367.402123217165,367.902004037933,368.90176567947,
369.901527321006,370.901288962543,371.90105060408,372.900812245617,373.900573887153,
374.400454707922,374.90033552869,375.900097170227,376.899858811763,377.8996204533,
378.899382094837,379.899143736374,380.89890537791,381.398786198679,381.898667019447,
382.898428660984,383.89819030252,384.897951944057,385.897713585594,386.897475227131,
387.897236868667,388.397117689436,388.896998510204,389.896760151741,390.896521793277,
391.896283434814,392.896045076351,393.895806717888,394.895568359424,395.395449180193,
395.895330000961,396.895091642498,397.894853284034,398.894614925571,399.894376567108,
400.894138208645,401.893899850181,402.39378067095,402.893661491718,403.893423133255,
404.893184774791,405.892946416328,406.892708057865,407.892469699402,408.892231340938,
409.392112161707,409.891992982475,410.891754624012,411.891516265548,412.891277907085,
413.891039548622,414.890801190159,415.890562831695,416.390443652464,416.890324473232,
417.890086114769,418.889847756306,419.889609397842,420.889371039379,421.889132680916,
422.888894322452,423.388775143221,423.888655963989,424.888417605526,425.888179247063,
426.887940888599,427.887702530136,428.887464171673,429.887225813209,430.387106633978,
430.886987454746,431.886749096283,432.88651073782,433.886272379356,434.886034020893,
435.88579566243,436.885557303966,437.385438124735,437.885318945503,438.88508058704,
439.884842228577,440.884603870113,441.88436551165,442.884127153187,443.883888794723,
444.383769615492,444.88365043626,445.883412077797,446.883173719334,447.88293536087,
448.882697002407,449.882458643944,450.882220285481,451.382101106249,451.881981927017,
452.881743568554,453.881505210091,454.881266851627,455.881028493164,456.880790134701,
457.880551776237,458.380432597006,458.880313417774,459.880075059311,460.879836700848,
461.879598342384,462.879359983921,463.879121625458,464.878883266995,465.378764087763,
465.878644908531,466.878406550068,467.878168191605,468.877929833141,469.877691474678,
470.877453116215,471.877214757752,472.37709557852,472.876976399288,473.876738040825,
474.876499682362,475.876261323898,476.876022965435,477.875784606972,478.875546248509,
479.375427069277,479.875307890045,480.875069531582,481.874831173119,482.874592814655,
483.874354456192,484.874116097729,485.873877739266,486.373758560034,486.873639380802,
487.873401022339,488.873162663876,489.872924305412,490.872685946949,491.872447588486,
492.872209230023,493.372090050791,493.871970871559,494.871732513096,495.871494154633,
496.87125579617,497.871017437706,498.870779079243,499.87054072078,500.370421541548,
500.870302362316,501.870064003853,502.86982564539,503.869587286927,504.869348928463,
505.86911057,506.868872211537,507.368753032305,507.868633853073,508.86839549461,
509.868157136147,510.867918777684,511.86768041922,512.867442060757,513.867203702294,
514.367084523062,514.86696534383,515.866726985367,516.866488626904,517.866250268441,
518.866011909977,519.865773551514,520.865535193051,521.365416013819,521.865296834587,
522.865058476124,523.864820117661,524.864581759198,525.864343400734,526.864105042271,
527.863866683808,528.363747504576,528.863628325344,529.863389966881,530.863151608418,
531.862913249955,532.862674891491,533.862436533028,534.862198174565,535.362078995333,
535.861959816101,536.861721457638,537.861483099175,538.861244740712,539.861006382248,
540.860768023785,541.860529665322,542.36041048609,542.860291306858,543.860052948395,
544.859814589932,545.859576231469,546.859337873005,547.859099514542,548.858861156079,
549.358741976847,549.858622797615,550.858384439152,551.858146080689,552.857907722226,
553.857669363762,554.857431005299,555.857192646836,556.357073467604,556.856954288373,
557.856715929909,558.856477571446,559.856239212983,560.856000854519,561.855762496056,
562.855524137593,563.355404958361,563.85528577913,564.855047420666,565.854809062203,
566.85457070374,567.854332345276,568.854093986813,569.85385562835,570.353736449118,
570.853617269887,571.853378911423,572.85314055296,573.852902194497,574.852663836033,
575.85242547757,576.852187119107,577.352067939875,577.851948760644,578.85171040218,
579.851472043717,580.851233685254,581.85099532679,582.850756968327,583.850518609864,
584.350399430632,584.850280251401,585.850041892937,586.849803534474,587.849565176011,
588.849326817548,589.849088459084,590.848850100621,591.348730921389,591.848611742158,
592.848373383694,593.848135025231,594.847896666768,595.847658308305,596.847419949841,
597.847181591378,598.347062412146,598.846943232915,599.846704874451,600.846466515988,
601.846228157525,602.845989799061,603.845751440598,604.845513082135,605.345393902903,
605.845274723672,606.845036365208,607.844798006745,608.844559648282,609.844321289819,
610.844082931355,611.843844572892,612.34372539366,612.843606214429,613.843367855965,
614.843129497502,615.842891139039,616.842652780576,617.842414422112,618.842176063649,
619.342056884417,619.841937705186,620.841699346722,621.841460988259,622.841222629796,
623.840984271333,624.840745912869,625.840507554406,626.340388375174,626.840269195943,
627.84003083748,628.839792479016,629.839554120553,630.83931576209,631.839077403626,
632.838839045163,633.338719865931,633.8386006867,634.838362328236,635.838123969773,
636.83788561131,637.837647252847,638.837408894383,639.337289715152,639.83717053592),
 .UNSPECIFIED.);
#71=B_SPLINE_CURVE_WITH_KNOTS('',3,(#30996,#30997,#30998,#30999,#31000,
#31001,#31002,#31003,#31004,#31005,#31006,#31007,#31008),.UNSPECIFIED.,
 .F.,.F.,(4,3,3,3,4),(-3.66465818398557,-2.83011024963485,-1.99556231528413,
-1.16101438093341,-0.960268764914558),.UNSPECIFIED.);
#72=B_SPLINE_CURVE_WITH_KNOTS('',3,(#31011,#31012,#31013,#31014),
 .UNSPECIFIED.,.F.,.F.,(4,4),(0.,0.437203234522177),.UNSPECIFIED.);
#73=B_SPLINE_CURVE_WITH_KNOTS('',3,(#31019,#31020,#31021,#31022,#31023,
#31024,#31025,#31026,#31027,#31028,#31029,#31030,#31031,#31032,#31033,#31034,
#31035,#31036,#31037,#31038,#31039,#31040,#31041,#31042,#31043),
 .UNSPECIFIED.,.F.,.F.,(4,3,3,3,3,3,3,3,4),(-9.94784349116513,-8.99785477383045,
-7.99809313229373,-6.99833149075702,-6.49845066998866,-5.9985698492203,
-4.99880820768358,-3.99904656614687,-3.66465818398557),.UNSPECIFIED.);
#74=B_SPLINE_CURVE_WITH_KNOTS('',3,(#31044,#31045,#31046,#31047,#31048,
#31049,#31050,#31051,#31052,#31053,#31054,#31055,#31056,#31057,#31058,#31059,
#31060,#31061,#31062,#31063,#31064,#31065,#31066,#31067,#31068),
 .UNSPECIFIED.,.F.,.F.,(4,3,3,3,3,3,3,3,4),(0.437203234522177,1.27175116887288,
2.10629910322359,2.9408470375743,3.775394971925,4.60994290627571,5.44449084062642,
6.27903877497713,6.72038854170174),.UNSPECIFIED.);
#75=B_SPLINE_CURVE_WITH_KNOTS('',3,(#31073,#31074,#31075,#31076,#31077,
#31078,#31079,#31080,#31081,#31082,#31083,#31084,#31085,#31086,#31087,#31088,
#31089,#31090,#31091,#31092,#31093,#31094,#31095,#31096,#31097,#31098,#31099,
#31100),.UNSPECIFIED.,.F.,.F.,(4,3,3,3,3,3,3,3,3,4),(-16.2310287983448,
-15.9961862645875,-14.9964246230508,-13.996662981514,-13.4967821607457,
-12.9969013399773,-11.9971396984406,-10.9973780569039,-9.99761641536717,
-9.94784349116513),.UNSPECIFIED.);
#76=B_SPLINE_CURVE_WITH_KNOTS('',3,(#31101,#31102,#31103,#31104,#31105,
#31106,#31107,#31108,#31109,#31110,#31111,#31112,#31113,#31114,#31115,#31116,
#31117,#31118,#31119,#31120,#31121,#31122,#31123,#31124,#31125),
 .UNSPECIFIED.,.F.,.F.,(4,3,3,3,3,3,3,3,4),(6.72038854170174,6.99833149075699,
7.99809313229371,8.99785477383043,9.99761641536715,10.9973780569039,11.9971396984406,
12.9969013399773,13.0035738488813),.UNSPECIFIED.);
#77=B_SPLINE_CURVE_WITH_KNOTS('',3,(#31130,#31131,#31132,#31133,#31134,
#31135,#31136,#31137,#31138,#31139,#31140,#31141,#31142,#31143,#31144,#31145,
#31146,#31147,#31148,#31149,#31150,#31151,#31152,#31153,#31154),
 .UNSPECIFIED.,.F.,.F.,(4,3,3,3,3,3,3,3,4),(-22.5142141055244,-21.6796661711737,
-20.845118236823,-20.0105703024723,-19.1760223681216,-18.3414744337709,
-17.5069264994202,-16.6723785650695,-16.2310287983448),.UNSPECIFIED.);
#78=B_SPLINE_CURVE_WITH_KNOTS('',3,(#31155,#31156,#31157,#31158,#31159,
#31160,#31161,#31162,#31163,#31164,#31165,#31166,#31167,#31168,#31169,#31170,
#31171,#31172,#31173,#31174,#31175,#31176,#31177,#31178,#31179),
 .UNSPECIFIED.,.F.,.F.,(4,3,3,3,3,3,3,3,4),(13.0035738488813,13.4967821607457,
13.996662981514,14.9964246230507,15.9961862645875,16.9959479061242,17.9957095476609,
18.9954711891976,19.286759156061),.UNSPECIFIED.);
#79=B_SPLINE_CURVE_WITH_KNOTS('',3,(#31184,#31185,#31186,#31187,#31188,
#31189,#31190,#31191,#31192,#31193,#31194,#31195,#31196,#31197,#31198,#31199,
#31200,#31201,#31202,#31203,#31204,#31205,#31206,#31207,#31208),
 .UNSPECIFIED.,.F.,.F.,(4,3,3,3,3,3,3,3,4),(-28.7973994127039,-27.9628514783532,
-27.1283035440025,-26.2937556096518,-25.459207675301,-24.6246597409503,
-23.7901118065996,-22.9555638722489,-22.5142141055244),.UNSPECIFIED.);
#80=B_SPLINE_CURVE_WITH_KNOTS('',3,(#31209,#31210,#31211,#31212,#31213,
#31214,#31215,#31216,#31217,#31218,#31219,#31220,#31221,#31222,#31223,#31224,
#31225,#31226,#31227,#31228,#31229,#31230,#31231,#31232,#31233),
 .UNSPECIFIED.,.F.,.F.,(4,3,3,3,3,3,3,3,4),(19.286759156061,20.1213070904117,
20.9558550247624,21.7904029591131,22.6249508934638,23.4594988278145,24.2940467621652,
25.1285946965159,25.5699444632405),.UNSPECIFIED.);
#81=B_SPLINE_CURVE_WITH_KNOTS('',3,(#31238,#31239,#31240,#31241,#31242,
#31243,#31244,#31245,#31246,#31247,#31248,#31249,#31250,#31251,#31252,#31253,
#31254,#31255,#31256,#31257,#31258,#31259,#31260,#31261,#31262),
 .UNSPECIFIED.,.F.,.F.,(4,3,3,3,3,3,3,3,4),(-35.0805847198835,-34.2460367855328,
-33.4114888511821,-32.5769409168313,-31.7423929824806,-30.9078450481299,
-30.0732971137792,-29.2387491794285,-28.7973994127039),.UNSPECIFIED.);
#82=B_SPLINE_CURVE_WITH_KNOTS('',3,(#31263,#31264,#31265,#31266,#31267,
#31268,#31269,#31270,#31271,#31272,#31273,#31274,#31275,#31276,#31277,#31278,
#31279,#31280,#31281,#31282,#31283,#31284,#31285,#31286,#31287),
 .UNSPECIFIED.,.F.,.F.,(4,3,3,3,3,3,3,3,4),(25.5699444632405,25.9938026799547,
26.9935643214914,27.4934451422597,27.9933259630281,28.9930876045648,29.9928492461015,
30.9926108876382,31.8531297704201),.UNSPECIFIED.);
#83=B_SPLINE_CURVE_WITH_KNOTS('',3,(#31292,#31293,#31294,#31295,#31296,
#31297,#31298,#31299,#31300,#31301,#31302,#31303,#31304,#31305,#31306,#31307,
#31308,#31309,#31310,#31311,#31312,#31313),.UNSPECIFIED.,.F.,.F.,(4,3,3,
3,3,3,3,4),(-41.3637700270631,-40.9902273030054,-39.9904656614687,-38.990704019932,
-37.9909423783952,-36.9911807368585,-35.9914190953218,-35.0805847198835),
 .UNSPECIFIED.);
#84=B_SPLINE_CURVE_WITH_KNOTS('',3,(#31314,#31315,#31316,#31317,#31318,
#31319,#31320,#31321,#31322,#31323,#31324,#31325,#31326,#31327,#31328,#31329,
#31330,#31331,#31332,#31333,#31334,#31335,#31336,#31337,#31338),
 .UNSPECIFIED.,.F.,.F.,(4,3,3,3,3,3,3,3,4),(31.8531297704201,32.6876777047708,
33.5222256391215,34.3567735734723,35.191321507823,36.0258694421737,36.8604173765244,
37.6949653108752,38.1363150775997),.UNSPECIFIED.);
#85=B_SPLINE_CURVE_WITH_KNOTS('',3,(#31343,#31344,#31345,#31346,#31347,
#31348,#31349,#31350,#31351,#31352,#31353,#31354,#31355,#31356,#31357,#31358,
#31359,#31360,#31361,#31362,#31363,#31364,#31365,#31366,#31367),
 .UNSPECIFIED.,.F.,.F.,(4,3,3,3,3,3,3,3,4),(-47.6469553342427,-46.812407399892,
-45.9778594655413,-45.1433115311906,-44.3087635968399,-43.4742156624892,
-42.6396677281384,-41.8051197937877,-41.3637700270631),.UNSPECIFIED.);
#86=B_SPLINE_CURVE_WITH_KNOTS('',3,(#31368,#31369,#31370,#31371,#31372,
#31373,#31374,#31375,#31376,#31377,#31378,#31379,#31380,#31381,#31382,#31383,
#31384,#31385,#31386,#31387,#31388,#31389,#31390,#31391,#31392),
 .UNSPECIFIED.,.F.,.F.,(4,3,3,3,3,3,3,3,4),(38.1363150775997,38.990704019932,
39.9904656614687,40.9902273030054,41.4901081237738,41.9899889445422,42.9897505860789,
43.9895122276156,44.4195003847792),.UNSPECIFIED.);
#87=B_SPLINE_CURVE_WITH_KNOTS('',3,(#31397,#31398,#31399,#31400,#31401,
#31402,#31403,#31404,#31405,#31406,#31407,#31408,#31409,#31410,#31411,#31412,
#31413,#31414,#31415,#31416,#31417,#31418,#31419,#31420,#31421),
 .UNSPECIFIED.,.F.,.F.,(4,3,3,3,3,3,3,3,4),(-53.9301406414223,-52.987367001446,
-51.9876053599093,-50.9878437183726,-49.9880820768358,-48.9883204352991,
-48.4884396145308,-47.9885587937624,-47.6469553342427),.UNSPECIFIED.);
#88=B_SPLINE_CURVE_WITH_KNOTS('',3,(#31422,#31423,#31424,#31425,#31426,
#31427,#31428,#31429,#31430,#31431,#31432,#31433,#31434,#31435,#31436,#31437,
#31438,#31439,#31440,#31441,#31442,#31443,#31444,#31445,#31446),
 .UNSPECIFIED.,.F.,.F.,(4,3,3,3,3,3,3,3,4),(44.4195003847792,45.25404831913,
46.0885962534807,46.9231441878314,47.7576921221821,48.5922400565329,49.4267879908836,
50.2613359252343,50.7026856919589),.UNSPECIFIED.);
#89=B_SPLINE_CURVE_WITH_KNOTS('',3,(#31451,#31452,#31453,#31454,#31455,
#31456,#31457,#31458,#31459,#31460,#31461,#31462,#31463,#31464,#31465,#31466,
#31467,#31468,#31469,#31470,#31471,#31472,#31473,#31474,#31475),
 .UNSPECIFIED.,.F.,.F.,(4,3,3,3,3,3,3,3,4),(-60.2133259486019,-59.3787780142511,
-58.5442300799004,-57.7096821455496,-56.8751342111989,-56.0405862768482,
-55.2060383424974,-54.3714904081467,-53.9301406414223),.UNSPECIFIED.);
#90=B_SPLINE_CURVE_WITH_KNOTS('',3,(#31476,#31477,#31478,#31479,#31480,
#31481,#31482,#31483,#31484,#31485,#31486,#31487,#31488,#31489,#31490,#31491,
#31492,#31493,#31494,#31495,#31496,#31497,#31498,#31499,#31500),
 .UNSPECIFIED.,.F.,.F.,(4,3,3,3,3,3,3,3,4),(50.7026856919589,51.5372336263096,
52.3717815606603,53.206329495011,54.0408774293617,54.8754253637125,55.7099732980632,
56.5445212324139,56.9858709991385),.UNSPECIFIED.);
#91=B_SPLINE_CURVE_WITH_KNOTS('',3,(#31505,#31506,#31507,#31508,#31509,
#31510,#31511,#31512,#31513,#31514,#31515,#31516,#31517,#31518,#31519,#31520,
#31521,#31522,#31523,#31524,#31525,#31526,#31527,#31528,#31529),
 .UNSPECIFIED.,.F.,.F.,(4,3,3,3,3,3,3,3,4),(-66.4965112557814,-65.6619633214307,
-64.82741538708,-63.9928674527293,-63.1583195183786,-62.323771584028,-61.4892236496773,
-60.6546757153266,-60.2133259486019),.UNSPECIFIED.);
#92=B_SPLINE_CURVE_WITH_KNOTS('',3,(#31530,#31531,#31532,#31533,#31534,
#31535,#31536,#31537,#31538,#31539,#31540,#31541,#31542,#31543,#31544,#31545,
#31546,#31547,#31548,#31549,#31550,#31551,#31552,#31553,#31554),
 .UNSPECIFIED.,.F.,.F.,(4,3,3,3,3,3,3,3,4),(56.9858709991385,57.9861752091296,
58.9859368506664,59.9856984922031,60.9854601337398,61.9852217752765,62.4851025960449,
62.9849834168133,63.269056306318),.UNSPECIFIED.);
#93=B_SPLINE_CURVE_WITH_KNOTS('',3,(#31559,#31560,#31561,#31562,#31563,
#31564,#31565,#31566,#31567,#31568,#31569,#31570,#31571,#31572,#31573,#31574,
#31575,#31576,#31577,#31578,#31579,#31580,#31581,#31582,#31583),
 .UNSPECIFIED.,.F.,.F.,(4,3,3,3,3,3,3,3,4),(-72.7796965629611,-71.9828381906436,
-70.9830765491069,-69.9833149075702,-69.4834340868018,-68.9835532660335,
-67.9837916244967,-66.98402998296,-66.4965112557814),.UNSPECIFIED.);
#94=B_SPLINE_CURVE_WITH_KNOTS('',3,(#31584,#31585,#31586,#31587,#31588,
#31589,#31590,#31591,#31592,#31593,#31594,#31595,#31596,#31597,#31598,#31599,
#31600,#31601,#31602,#31603,#31604,#31605,#31606,#31607,#31608),
 .UNSPECIFIED.,.F.,.F.,(4,3,3,3,3,3,3,3,4),(63.269056306318,64.1036042406688,
64.9381521750195,65.7727001093702,66.6072480437209,67.4417959780717,68.2763439124224,
69.1108918467731,69.5522416134976),.UNSPECIFIED.);
#95=B_SPLINE_CURVE_WITH_KNOTS('',3,(#31613,#31614,#31615,#31616,#31617,
#31618,#31619,#31620,#31621,#31622,#31623,#31624,#31625,#31626,#31627,#31628,
#31629,#31630,#31631,#31632,#31633,#31634,#31635,#31636,#31637,#31638,#31639,
#31640),.UNSPECIFIED.,.F.,.F.,(4,3,3,3,3,3,3,3,3,4),(-79.0628818701407,
-78.9811696814006,-77.9814080398639,-76.9816463983272,-76.4817655775588,
-75.9818847567905,-74.9821231152538,-73.982361473717,-72.9825998321803,
-72.7796965629611),.UNSPECIFIED.);
#96=B_SPLINE_CURVE_WITH_KNOTS('',3,(#31641,#31642,#31643,#31644,#31645,
#31646,#31647,#31648,#31649,#31650,#31651,#31652,#31653,#31654,#31655,#31656,
#31657,#31658,#31659,#31660,#31661,#31662),.UNSPECIFIED.,.F.,.F.,(4,3,3,
3,3,3,3,4),(69.5522416134976,69.9833149075702,70.983076549107,71.9828381906437,
72.9825998321804,73.9823614737171,74.9821231152538,75.8354269206773),
 .UNSPECIFIED.);
#97=B_SPLINE_CURVE_WITH_KNOTS('',3,(#31667,#31668,#31669,#31670,#31671,
#31672,#31673,#31674,#31675,#31676,#31677,#31678,#31679,#31680,#31681,#31682,
#31683,#31684,#31685,#31686,#31687,#31688,#31689,#31690,#31691),
 .UNSPECIFIED.,.F.,.F.,(4,3,3,3,3,3,3,3,4),(-85.3460671773202,-84.9797395306209,
-83.9799778890842,-83.4800970683159,-82.9802162475475,-81.9804546060108,
-80.9806929644741,-79.9809313229374,-79.0628818701407),.UNSPECIFIED.);
#98=B_SPLINE_CURVE_WITH_KNOTS('',3,(#31692,#31693,#31694,#31695,#31696,
#31697,#31698,#31699,#31700,#31701,#31702,#31703,#31704,#31705,#31706,#31707,
#31708,#31709,#31710,#31711,#31712,#31713,#31714,#31715,#31716),
 .UNSPECIFIED.,.F.,.F.,(4,3,3,3,3,3,3,3,4),(75.8354269206773,76.669974855028,
77.5045227893787,78.3390707237294,79.1736186580801,80.0081665924308,80.8427145267815,
81.6772624611322,82.1186122278568),.UNSPECIFIED.);
#99=B_SPLINE_CURVE_WITH_KNOTS('',3,(#31721,#31722,#31723,#31724,#31725,
#31726,#31727,#31728,#31729,#31730,#31731,#31732,#31733,#31734,#31735,#31736,
#31737,#31738,#31739,#31740,#31741,#31742,#31743,#31744,#31745),
 .UNSPECIFIED.,.F.,.F.,(4,3,3,3,3,3,3,3,4),(-91.6292524844998,-90.794704550149,
-89.9601566157983,-89.1256086814476,-88.2910607470968,-87.4565128127461,
-86.6219648783954,-85.7874169440446,-85.3460671773202),.UNSPECIFIED.);
#100=B_SPLINE_CURVE_WITH_KNOTS('',3,(#31746,#31747,#31748,#31749,#31750,
#31751,#31752,#31753,#31754,#31755,#31756,#31757,#31758,#31759,#31760,#31761,
#31762,#31763,#31764,#31765,#31766,#31767,#31768,#31769,#31770),
 .UNSPECIFIED.,.F.,.F.,(4,3,3,3,3,3,3,3,4),(82.1186122278568,82.9802162475476,
83.4800970683159,83.9799778890843,84.979739530621,85.9795011721578,86.9792628136945,
87.9790244552312,88.4017975350364),.UNSPECIFIED.);
#101=B_SPLINE_CURVE_WITH_KNOTS('',3,(#31775,#31776,#31777,#31778,#31779,
#31780,#31781,#31782,#31783,#31784,#31785,#31786,#31787,#31788,#31789,#31790,
#31791,#31792,#31793,#31794,#31795,#31796,#31797,#31798,#31799),
 .UNSPECIFIED.,.F.,.F.,(4,3,3,3,3,3,3,3,4),(-97.9124377916795,-97.4767600498299,
-96.9768792290615,-95.9771175875248,-94.9773559459881,-93.9775943044514,
-92.9778326629147,-91.9780710213779,-91.6292524844998),.UNSPECIFIED.);
#102=B_SPLINE_CURVE_WITH_KNOTS('',3,(#31800,#31801,#31802,#31803,#31804,
#31805,#31806,#31807,#31808,#31809,#31810,#31811,#31812,#31813,#31814,#31815,
#31816,#31817,#31818,#31819,#31820,#31821,#31822,#31823,#31824),
 .UNSPECIFIED.,.F.,.F.,(4,3,3,3,3,3,3,3,4),(88.4017975350364,89.2363454693871,
90.0708934037379,90.9054413380886,91.7399892724394,92.5745372067901,93.4090851411408,
94.2436330754916,94.6849828422161),.UNSPECIFIED.);
#103=B_SPLINE_CURVE_WITH_KNOTS('',3,(#31829,#31830,#31831,#31832,#31833,
#31834,#31835,#31836,#31837,#31838,#31839,#31840,#31841,#31842,#31843,#31844,
#31845,#31846,#31847,#31848,#31849,#31850,#31851,#31852,#31853),
 .UNSPECIFIED.,.F.,.F.,(4,3,3,3,3,3,3,3,4),(-104.195623098859,-103.361075164508,
-102.526527230158,-101.691979295807,-100.857431361456,-100.022883427105,
-99.1883354927548,-98.3537875584041,-97.9124377916795),.UNSPECIFIED.);
#104=B_SPLINE_CURVE_WITH_KNOTS('',3,(#31854,#31855,#31856,#31857,#31858,
#31859,#31860,#31861,#31862,#31863,#31864,#31865,#31866,#31867,#31868,#31869,
#31870,#31871,#31872,#31873,#31874,#31875,#31876,#31877,#31878),
 .UNSPECIFIED.,.F.,.F.,(4,3,3,3,3,3,3,3,4),(94.6849828422161,94.9773559459882,
95.9771175875249,96.9768792290616,97.47676004983,97.9766408705983,98.976402512135,
99.9761641536718,100.968168149396),.UNSPECIFIED.);
#105=B_SPLINE_CURVE_WITH_KNOTS('',3,(#31883,#31884,#31885,#31886,#31887,
#31888,#31889,#31890,#31891,#31892,#31893,#31894,#31895,#31896,#31897,#31898,
#31899,#31900,#31901,#31902,#31903,#31904,#31905,#31906,#31907),
 .UNSPECIFIED.,.F.,.F.,(4,3,3,3,3,3,3,3,4),(-110.478808406039,-109.973780569039,
-108.974018927502,-107.974257285965,-106.974495644429,-105.974734002892,
-104.974972361355,-104.475091540587,-104.195623098859),.UNSPECIFIED.);
#106=B_SPLINE_CURVE_WITH_KNOTS('',3,(#31908,#31909,#31910,#31911,#31912,
#31913,#31914,#31915,#31916,#31917,#31918,#31919,#31920,#31921,#31922,#31923,
#31924,#31925,#31926,#31927,#31928,#31929,#31930,#31931,#31932,#31933,#31934,
#31935),.UNSPECIFIED.,.F.,.F.,(4,3,3,3,3,3,3,3,3,4),(100.968168149396,100.975925795209,
101.975687436745,102.975449078282,103.975210719819,104.475091540587,104.974972361355,
105.974734002892,106.974495644429,107.251353456575),.UNSPECIFIED.);
#107=B_SPLINE_CURVE_WITH_KNOTS('',3,(#31940,#31941,#31942,#31943,#31944,
#31945,#31946,#31947,#31948,#31949,#31950,#31951,#31952,#31953,#31954,#31955,
#31956,#31957,#31958,#31959,#31960,#31961,#31962,#31963,#31964),
 .UNSPECIFIED.,.F.,.F.,(4,3,3,3,3,3,3,3,4),(-116.761993713218,-115.927445778868,
-115.092897844517,-114.258349910166,-113.423801975815,-112.589254041465,
-111.754706107114,-110.920158172763,-110.478808406039),.UNSPECIFIED.);
#108=B_SPLINE_CURVE_WITH_KNOTS('',3,(#31965,#31966,#31967,#31968,#31969,
#31970,#31971,#31972,#31973,#31974,#31975,#31976,#31977,#31978,#31979,#31980,
#31981,#31982,#31983,#31984,#31985,#31986,#31987,#31988,#31989),
 .UNSPECIFIED.,.F.,.F.,(4,3,3,3,3,3,3,3,4),(107.251353456575,108.085901390926,
108.920449325277,109.754997259627,110.589545193978,111.424093128329,112.258641062679,
113.09318899703,113.534538763755),.UNSPECIFIED.);
#109=B_SPLINE_CURVE_WITH_KNOTS('',3,(#31994,#31995,#31996,#31997,#31998,
#31999,#32000,#32001,#32002,#32003,#32004,#32005,#32006,#32007,#32008,#32009,
#32010,#32011,#32012,#32013,#32014,#32015,#32016,#32017,#32018),
 .UNSPECIFIED.,.F.,.F.,(4,3,3,3,3,3,3,3,4),(-123.045179020398,-122.210631086047,
-121.376083151696,-120.541535217346,-119.706987282995,-118.872439348644,
-118.037891414293,-117.203343479943,-116.761993713218),.UNSPECIFIED.);
#110=B_SPLINE_CURVE_WITH_KNOTS('',3,(#32019,#32020,#32021,#32022,#32023,
#32024,#32025,#32026,#32027,#32028,#32029,#32030,#32031,#32032,#32033,#32034,
#32035,#32036,#32037,#32038,#32039,#32040,#32041,#32042,#32043),
 .UNSPECIFIED.,.F.,.F.,(4,3,3,3,3,3,3,3,4),(113.534538763755,114.369086698105,
115.203634632456,116.038182566807,116.872730501158,117.707278435508,118.541826369859,
119.37637430421,119.817724070934),.UNSPECIFIED.);
#111=B_SPLINE_CURVE_WITH_KNOTS('',3,(#32048,#32049,#32050,#32051,#32052,
#32053,#32054,#32055,#32056,#32057,#32058,#32059,#32060,#32061,#32062,#32063,
#32064,#32065,#32066,#32067,#32068,#32069,#32070,#32071,#32072),
 .UNSPECIFIED.,.F.,.F.,(4,3,3,3,3,3,3,3,4),(-129.328364327577,-128.969251758236,
-127.9694901167,-126.969728475163,-125.969966833626,-125.470086012858,-124.97020519209,
-123.970443550553,-123.045179020398),.UNSPECIFIED.);
#112=B_SPLINE_CURVE_WITH_KNOTS('',3,(#32073,#32074,#32075,#32076,#32077,
#32078,#32079,#32080,#32081,#32082,#32083,#32084,#32085,#32086,#32087,#32088,
#32089,#32090,#32091,#32092,#32093,#32094,#32095,#32096,#32097),
 .UNSPECIFIED.,.F.,.F.,(4,3,3,3,3,3,3,3,4),(119.817724070934,120.652272005285,
121.486819939636,122.321367873986,123.155915808337,123.990463742688,124.825011677039,
125.659559611389,126.100909378114),.UNSPECIFIED.);
#113=B_SPLINE_CURVE_WITH_KNOTS('',3,(#32102,#32103,#32104,#32105,#32106,
#32107,#32108,#32109,#32110,#32111,#32112,#32113,#32114,#32115,#32116,#32117,
#32118,#32119,#32120,#32121,#32122,#32123,#32124,#32125,#32126),
 .UNSPECIFIED.,.F.,.F.,(4,3,3,3,3,3,3,3,4),(-135.611549634757,-134.967821607457,
-133.96805996592,-132.968298324383,-132.468417503615,-131.968536682847,
-130.96877504131,-129.969013399773,-129.328364327577),.UNSPECIFIED.);
#114=B_SPLINE_CURVE_WITH_KNOTS('',3,(#32127,#32128,#32129,#32130,#32131,
#32132,#32133,#32134,#32135,#32136,#32137,#32138,#32139,#32140,#32141,#32142,
#32143,#32144,#32145,#32146,#32147,#32148),.UNSPECIFIED.,.F.,.F.,(4,3,3,
3,3,3,3,4),(126.100909378114,126.969728475163,127.9694901167,128.969251758237,
129.969013399773,130.96877504131,131.968536682847,132.384094685294),
 .UNSPECIFIED.);
#115=B_SPLINE_CURVE_WITH_KNOTS('',3,(#32153,#32154,#32155,#32156,#32157,
#32158,#32159,#32160,#32161,#32162,#32163,#32164,#32165,#32166,#32167,#32168,
#32169,#32170,#32171,#32172,#32173,#32174,#32175,#32176,#32177),
 .UNSPECIFIED.,.F.,.F.,(4,3,3,3,3,3,3,3,4),(-141.894734941937,-140.966391456677,
-139.96662981514,-139.466748994372,-138.966868173604,-137.967106532067,
-136.96734489053,-135.967583248994,-135.611549634757),.UNSPECIFIED.);
#116=B_SPLINE_CURVE_WITH_KNOTS('',3,(#32178,#32179,#32180,#32181,#32182,
#32183,#32184,#32185,#32186,#32187,#32188,#32189,#32190,#32191,#32192,#32193,
#32194,#32195,#32196,#32197,#32198,#32199,#32200,#32201,#32202),
 .UNSPECIFIED.,.F.,.F.,(4,3,3,3,3,3,3,3,4),(132.384094685294,133.218642619644,
134.053190553995,134.887738488346,135.722286422696,136.556834357047,137.391382291398,
138.225930225748,138.667279992473),.UNSPECIFIED.);
#117=B_SPLINE_CURVE_WITH_KNOTS('',3,(#32207,#32208,#32209,#32210,#32211,
#32212,#32213,#32214,#32215,#32216,#32217,#32218,#32219,#32220,#32221,#32222,
#32223,#32224,#32225,#32226,#32227,#32228,#32229,#32230,#32231),
 .UNSPECIFIED.,.F.,.F.,(4,3,3,3,3,3,3,3,4),(-148.177920249116,-147.343372314765,
-146.508824380415,-145.674276446064,-144.839728511713,-144.005180577363,
-143.170632643012,-142.336084708661,-141.894734941937),.UNSPECIFIED.);
#118=B_SPLINE_CURVE_WITH_KNOTS('',3,(#32232,#32233,#32234,#32235,#32236,
#32237,#32238,#32239,#32240,#32241,#32242,#32243,#32244,#32245,#32246,#32247,
#32248,#32249,#32250,#32251,#32252,#32253,#32254,#32255,#32256),
 .UNSPECIFIED.,.F.,.F.,(4,3,3,3,3,3,3,3,4),(138.667279992473,138.966868173604,
139.466748994372,139.96662981514,140.966391456677,141.966153098214,142.965914739751,
143.965676381287,144.950465299653),.UNSPECIFIED.);
#119=B_SPLINE_CURVE_WITH_KNOTS('',3,(#32261,#32262,#32263,#32264,#32265,
#32266,#32267,#32268,#32269,#32270,#32271,#32272,#32273,#32274,#32275,#32276,
#32277,#32278,#32279,#32280,#32281,#32282,#32283,#32284,#32285),
 .UNSPECIFIED.,.F.,.F.,(4,3,3,3,3,3,3,3,4),(-154.461105556296,-153.626557621945,
-152.792009687594,-151.957461753244,-151.122913818893,-150.288365884542,
-149.453817950192,-148.619270015841,-148.177920249116),.UNSPECIFIED.);
#120=B_SPLINE_CURVE_WITH_KNOTS('',3,(#32286,#32287,#32288,#32289,#32290,
#32291,#32292,#32293,#32294,#32295,#32296,#32297,#32298,#32299,#32300,#32301,
#32302,#32303,#32304,#32305,#32306,#32307,#32308,#32309,#32310),
 .UNSPECIFIED.,.F.,.F.,(4,3,3,3,3,3,3,3,4),(144.950465299653,145.785013234003,
146.619561168354,147.454109102705,148.288657037055,149.123204971406,149.957752905757,
150.792300840108,151.233650606832),.UNSPECIFIED.);
#121=B_SPLINE_CURVE_WITH_KNOTS('',3,(#32315,#32316,#32317,#32318,#32319,
#32320,#32321,#32322,#32323,#32324,#32325,#32326,#32327,#32328,#32329,#32330,
#32331,#32332,#32333,#32334,#32335,#32336,#32337,#32338,#32339),
 .UNSPECIFIED.,.F.,.F.,(4,3,3,3,3,3,3,3,4),(-160.744290863475,-160.461743466643,
-159.961862645875,-158.962101004338,-157.962339362801,-156.962577721265,
-155.962816079728,-154.963054438191,-154.461105556296),.UNSPECIFIED.);
#122=B_SPLINE_CURVE_WITH_KNOTS('',3,(#32340,#32341,#32342,#32343,#32344,
#32345,#32346,#32347,#32348,#32349,#32350,#32351,#32352,#32353,#32354,#32355,
#32356,#32357,#32358,#32359,#32360,#32361,#32362,#32363,#32364),
 .UNSPECIFIED.,.F.,.F.,(4,3,3,3,3,3,3,3,4),(151.233650606832,152.068198541183,
152.902746475534,153.737294409884,154.571842344235,155.406390278586,156.240938212937,
157.075486147287,157.516835914012),.UNSPECIFIED.);
#123=B_SPLINE_CURVE_WITH_KNOTS('',3,(#32369,#32370,#32371,#32372,#32373,
#32374,#32375,#32376,#32377,#32378,#32379,#32380,#32381,#32382,#32383,#32384,
#32385,#32386,#32387,#32388,#32389,#32390,#32391,#32392,#32393),
 .UNSPECIFIED.,.F.,.F.,(4,3,3,3,3,3,3,3,4),(-167.027476170655,-166.192928236304,
-165.358380301953,-164.523832367603,-163.689284433252,-162.854736498901,
-162.02018856455,-161.1856406302,-160.744290863475),.UNSPECIFIED.);
#124=B_SPLINE_CURVE_WITH_KNOTS('',3,(#32394,#32395,#32396,#32397,#32398,
#32399,#32400,#32401,#32402,#32403,#32404,#32405,#32406,#32407,#32408,#32409,
#32410,#32411,#32412,#32413,#32414,#32415,#32416,#32417,#32418),
 .UNSPECIFIED.,.F.,.F.,(4,3,3,3,3,3,3,3,4),(157.516835914012,157.962339362801,
158.962101004338,159.961862645875,160.461743466643,160.961624287412,161.961385928948,
162.961147570485,163.800021221191),.UNSPECIFIED.);
#125=B_SPLINE_CURVE_WITH_KNOTS('',3,(#32423,#32424,#32425,#32426,#32427,
#32428,#32429,#32430,#32431,#32432,#32433,#32434,#32435,#32436,#32437,#32438,
#32439,#32440,#32441,#32442,#32443,#32444,#32445,#32446,#32447),
 .UNSPECIFIED.,.F.,.F.,(4,3,3,3,3,3,3,3,4),(-173.310661477834,-172.958763985852,
-171.959002344315,-170.959240702779,-169.959479061242,-168.959717419705,
-167.959955778168,-167.4600749574,-167.027476170655),.UNSPECIFIED.);
#126=B_SPLINE_CURVE_WITH_KNOTS('',3,(#32448,#32449,#32450,#32451,#32452,
#32453,#32454,#32455,#32456,#32457,#32458,#32459,#32460,#32461,#32462,#32463,
#32464,#32465,#32466,#32467,#32468,#32469,#32470,#32471,#32472,#32473,#32474,
#32475),.UNSPECIFIED.,.F.,.F.,(4,3,3,3,3,3,3,3,3,4),(163.800021221191,163.960909212022,
164.960670853558,165.960432495095,166.960194136632,167.4600749574,167.959955778169,
168.959717419705,169.959479061242,170.083206528371),.UNSPECIFIED.);
#127=B_SPLINE_CURVE_WITH_KNOTS('',3,(#32480,#32481,#32482,#32483,#32484,
#32485,#32486,#32487,#32488,#32489,#32490,#32491,#32492,#32493,#32494,#32495,
#32496,#32497,#32498,#32499,#32500,#32501,#32502,#32503,#32504),
 .UNSPECIFIED.,.F.,.F.,(4,3,3,3,3,3,3,3,4),(-179.593846785014,-178.759298850663,
-177.924750916312,-177.090202981962,-176.255655047611,-175.42110711326,
-174.586559178909,-173.752011244559,-173.310661477834),.UNSPECIFIED.);
#128=B_SPLINE_CURVE_WITH_KNOTS('',3,(#32505,#32506,#32507,#32508,#32509,
#32510,#32511,#32512,#32513,#32514,#32515,#32516,#32517,#32518,#32519,#32520,
#32521,#32522,#32523,#32524,#32525,#32526,#32527,#32528,#32529),
 .UNSPECIFIED.,.F.,.F.,(4,3,3,3,3,3,3,3,4),(170.083206528371,170.959240702779,
171.959002344316,172.958763985852,173.958525627389,174.458406448157,174.958287268926,
175.958048910462,176.366391835551),.UNSPECIFIED.);
#129=B_SPLINE_CURVE_WITH_KNOTS('',3,(#32534,#32535,#32536,#32537,#32538,
#32539,#32540,#32541,#32542,#32543,#32544,#32545,#32546,#32547,#32548,#32549,
#32550,#32551,#32552,#32553,#32554,#32555,#32556,#32557,#32558),
 .UNSPECIFIED.,.F.,.F.,(4,3,3,3,3,3,3,3,4),(-185.877032092193,-184.955903684293,
-183.956142042756,-182.956380401219,-181.956618759682,-181.456737938914,
-180.956857118146,-179.957095476609,-179.593846785014),.UNSPECIFIED.);
#130=B_SPLINE_CURVE_WITH_KNOTS('',3,(#32559,#32560,#32561,#32562,#32563,
#32564,#32565,#32566,#32567,#32568,#32569,#32570,#32571,#32572,#32573,#32574,
#32575,#32576,#32577,#32578,#32579,#32580,#32581,#32582,#32583),
 .UNSPECIFIED.,.F.,.F.,(4,3,3,3,3,3,3,3,4),(176.366391835551,177.200939769901,
178.035487704252,178.870035638603,179.704583572953,180.539131507304,181.373679441655,
182.208227376006,182.64957714273),.UNSPECIFIED.);
#131=B_SPLINE_CURVE_WITH_KNOTS('',3,(#32588,#32589,#32590,#32591,#32592,
#32593,#32594,#32595,#32596,#32597,#32598,#32599,#32600,#32601,#32602,#32603,
#32604,#32605,#32606,#32607,#32608,#32609,#32610,#32611,#32612,#32613,#32614,
#32615),.UNSPECIFIED.,.F.,.F.,(4,3,3,3,3,3,3,3,3,4),(-192.160217399373,
-191.95423517505,-190.954473533513,-189.954711891976,-188.954950250439,
-188.455069429671,-187.955188608903,-186.955426967366,-185.955665325829,
-185.877032092193),.UNSPECIFIED.);
#132=B_SPLINE_CURVE_WITH_KNOTS('',3,(#32616,#32617,#32618,#32619,#32620,
#32621,#32622,#32623,#32624,#32625,#32626,#32627,#32628,#32629,#32630,#32631,
#32632,#32633,#32634,#32635,#32636,#32637,#32638,#32639,#32640),
 .UNSPECIFIED.,.F.,.F.,(4,3,3,3,3,3,3,3,4),(182.64957714273,182.956380401219,
183.956142042756,184.955903684293,185.95566532583,186.955426967366,187.955188608903,
188.455069429671,188.93276244991),.UNSPECIFIED.);
#133=B_SPLINE_CURVE_WITH_KNOTS('',3,(#32645,#32646,#32647,#32648,#32649,
#32650,#32651,#32652,#32653,#32654,#32655,#32656,#32657,#32658,#32659,#32660,
#32661,#32662,#32663,#32664,#32665,#32666,#32667,#32668,#32669),
 .UNSPECIFIED.,.F.,.F.,(4,3,3,3,3,3,3,3,4),(-198.443402706553,-197.95280502427,
-196.953043382733,-195.953281741197,-195.453400920428,-194.95352009966,
-193.953758458123,-192.953996816586,-192.160217399373),.UNSPECIFIED.);
#134=B_SPLINE_CURVE_WITH_KNOTS('',3,(#32670,#32671,#32672,#32673,#32674,
#32675,#32676,#32677,#32678,#32679,#32680,#32681,#32682,#32683,#32684,#32685,
#32686,#32687,#32688,#32689,#32690,#32691,#32692,#32693,#32694),
 .UNSPECIFIED.,.F.,.F.,(4,3,3,3,3,3,3,3,4),(188.93276244991,188.95495025044,
189.954711891976,190.954473533513,191.95423517505,192.953996816587,193.953758458123,
194.95352009966,195.215947757089),.UNSPECIFIED.);
#135=B_SPLINE_CURVE_WITH_KNOTS('',3,(#32699,#32700,#32701,#32702,#32703,
#32704,#32705,#32706,#32707,#32708,#32709,#32710,#32711,#32712,#32713,#32714,
#32715,#32716,#32717,#32718,#32719,#32720,#32721,#32722,#32723),
 .UNSPECIFIED.,.F.,.F.,(4,3,3,3,3,3,3,3,4),(-204.726588013732,-203.892040079381,
-203.057492145031,-202.22294421068,-201.388396276329,-200.553848341979,
-199.719300407628,-198.884752473277,-198.443402706553),.UNSPECIFIED.);
#136=B_SPLINE_CURVE_WITH_KNOTS('',3,(#32724,#32725,#32726,#32727,#32728,
#32729,#32730,#32731,#32732,#32733,#32734,#32735,#32736,#32737,#32738,#32739,
#32740,#32741,#32742,#32743,#32744,#32745,#32746,#32747,#32748),
 .UNSPECIFIED.,.F.,.F.,(4,3,3,3,3,3,3,3,4),(195.215947757089,196.05049569144,
196.885043625791,197.719591560141,198.554139494492,199.388687428843,200.223235363194,
201.057783297544,201.499133064269),.UNSPECIFIED.);
#137=B_SPLINE_CURVE_WITH_KNOTS('',3,(#32753,#32754,#32755,#32756,#32757,
#32758,#32759,#32760,#32761,#32762,#32763,#32764,#32765,#32766,#32767,#32768,
#32769,#32770,#32771,#32772,#32773,#32774,#32775,#32776,#32777),
 .UNSPECIFIED.,.F.,.F.,(4,3,3,3,3,3,3,3,4),(-211.009773320912,-210.175225386561,
-209.34067745221,-208.506129517859,-207.671581583509,-206.837033649158,
-206.002485714807,-205.167937780456,-204.726588013732),.UNSPECIFIED.);
#138=B_SPLINE_CURVE_WITH_KNOTS('',3,(#32778,#32779,#32780,#32781,#32782,
#32783,#32784,#32785,#32786,#32787,#32788,#32789,#32790,#32791,#32792,#32793,
#32794,#32795,#32796,#32797,#32798,#32799,#32800,#32801,#32802),
 .UNSPECIFIED.,.F.,.F.,(4,3,3,3,3,3,3,3,4),(201.499133064269,201.951851590417,
202.451732411185,202.951613231954,203.95137487349,204.951136515027,205.950898156564,
206.950659798101,207.782318371448),.UNSPECIFIED.);
#139=B_SPLINE_CURVE_WITH_KNOTS('',3,(#32807,#32808,#32809,#32810,#32811,
#32812,#32813,#32814,#32815,#32816,#32817,#32818,#32819,#32820,#32821,#32822,
#32823,#32824,#32825,#32826,#32827,#32828,#32829,#32830,#32831),
 .UNSPECIFIED.,.F.,.F.,(4,3,3,3,3,3,3,3,4),(-217.292958628091,-216.948276213468,
-216.448395392699,-215.948514571931,-214.948752930394,-213.948991288857,
-212.949229647321,-211.949468005784,-211.009773320912),.UNSPECIFIED.);
#140=B_SPLINE_CURVE_WITH_KNOTS('',3,(#32832,#32833,#32834,#32835,#32836,
#32837,#32838,#32839,#32840,#32841,#32842,#32843,#32844,#32845,#32846,#32847,
#32848,#32849,#32850,#32851,#32852,#32853,#32854,#32855,#32856),
 .UNSPECIFIED.,.F.,.F.,(4,3,3,3,3,3,3,3,4),(207.782318371448,208.616866305799,
209.45141424015,210.285962174501,211.120510108851,211.955058043202,212.789605977553,
213.624153911904,214.065503678628),.UNSPECIFIED.);
#141=B_SPLINE_CURVE_WITH_KNOTS('',3,(#32861,#32862,#32863,#32864,#32865,
#32866,#32867,#32868,#32869,#32870,#32871,#32872,#32873,#32874,#32875,#32876,
#32877,#32878,#32879,#32880,#32881,#32882,#32883,#32884,#32885),
 .UNSPECIFIED.,.F.,.F.,(4,3,3,3,3,3,3,3,4),(-223.576143935271,-222.74159600092,
-221.907048066569,-221.072500132219,-220.237952197868,-219.403404263517,
-218.568856329166,-217.734308394816,-217.292958628091),.UNSPECIFIED.);
#142=B_SPLINE_CURVE_WITH_KNOTS('',3,(#32886,#32887,#32888,#32889,#32890,
#32891,#32892,#32893,#32894,#32895,#32896,#32897,#32898,#32899,#32900,#32901,
#32902,#32903,#32904,#32905,#32906,#32907,#32908,#32909,#32910),
 .UNSPECIFIED.,.F.,.F.,(4,3,3,3,3,3,3,3,4),(214.065503678628,214.948752930394,
215.948514571931,216.448395392699,216.948276213468,217.948037855004,218.947799496541,
219.947561138078,220.348688985807),.UNSPECIFIED.);
#143=B_SPLINE_CURVE_WITH_KNOTS('',3,(#32915,#32916,#32917,#32918,#32919,
#32920,#32921,#32922,#32923,#32924,#32925,#32926,#32927,#32928,#32929,#32930,
#32931,#32932,#32933,#32934,#32935,#32936),.UNSPECIFIED.,.F.,.F.,(4,3,3,
3,3,3,3,4),(-229.85932924245,-228.945415911908,-227.945654270371,-226.945892628835,
-225.946130987298,-224.946369345761,-223.946607704225,-223.576143935271),
 .UNSPECIFIED.);
#144=B_SPLINE_CURVE_WITH_KNOTS('',3,(#32937,#32938,#32939,#32940,#32941,
#32942,#32943,#32944,#32945,#32946,#32947,#32948,#32949,#32950,#32951,#32952,
#32953,#32954,#32955,#32956,#32957,#32958,#32959,#32960,#32961),
 .UNSPECIFIED.,.F.,.F.,(4,3,3,3,3,3,3,3,4),(220.348688985807,220.947322779615,
221.947084421151,222.946846062688,223.446726883456,223.946607704225,224.946369345762,
225.946130987298,226.631874292987),.UNSPECIFIED.);
#145=B_SPLINE_CURVE_WITH_KNOTS('',3,(#32966,#32967,#32968,#32969,#32970,
#32971,#32972,#32973,#32974,#32975,#32976,#32977,#32978,#32979,#32980,#32981,
#32982,#32983,#32984,#32985,#32986,#32987,#32988,#32989,#32990),
 .UNSPECIFIED.,.F.,.F.,(4,3,3,3,3,3,3,3,4),(-236.14251454963,-235.307966615279,
-234.473418680928,-233.638870746578,-232.804322812227,-231.969774877876,
-231.135226943525,-230.300679009175,-229.85932924245),.UNSPECIFIED.);
#146=B_SPLINE_CURVE_WITH_KNOTS('',3,(#32991,#32992,#32993,#32994,#32995,
#32996,#32997,#32998,#32999,#33000,#33001,#33002,#33003,#33004,#33005,#33006,
#33007,#33008,#33009,#33010,#33011,#33012,#33013,#33014,#33015),
 .UNSPECIFIED.,.F.,.F.,(4,3,3,3,3,3,3,3,4),(226.631874292987,226.945892628835,
227.945654270372,228.945415911908,229.945177553445,230.445058374213,230.944939194982,
231.944700836519,232.915059600167),.UNSPECIFIED.);
#147=B_SPLINE_CURVE_WITH_KNOTS('',3,(#33020,#33021,#33022,#33023,#33024,
#33025,#33026,#33027,#33028,#33029,#33030,#33031,#33032,#33033,#33034,#33035,
#33036,#33037,#33038,#33039,#33040,#33041,#33042,#33043,#33044),
 .UNSPECIFIED.,.F.,.F.,(4,3,3,3,3,3,3,3,4),(-242.42569985681,-241.591151922459,
-240.756603988108,-239.922056053757,-239.087508119407,-238.252960185056,
-237.418412250705,-236.583864316354,-236.14251454963),.UNSPECIFIED.);
#148=B_SPLINE_CURVE_WITH_KNOTS('',3,(#33045,#33046,#33047,#33048,#33049,
#33050,#33051,#33052,#33053,#33054,#33055,#33056,#33057,#33058,#33059,#33060,
#33061,#33062,#33063,#33064,#33065,#33066,#33067,#33068,#33069),
 .UNSPECIFIED.,.F.,.F.,(4,3,3,3,3,3,3,3,4),(232.915059600167,233.749607534517,
234.584155468868,235.418703403219,236.253251337569,237.08779927192,237.922347206271,
238.756895140621,239.198244907346),.UNSPECIFIED.);
#149=B_SPLINE_CURVE_WITH_KNOTS('',3,(#33074,#33075,#33076,#33077,#33078,
#33079,#33080,#33081,#33082,#33083,#33084,#33085,#33086,#33087,#33088,#33089,
#33090,#33091,#33092,#33093,#33094,#33095,#33096,#33097,#33098),
 .UNSPECIFIED.,.F.,.F.,(4,3,3,3,3,3,3,3,4),(-248.708885163989,-247.874337229638,
-247.039789295288,-246.205241360937,-245.370693426586,-244.536145492235,
-243.701597557885,-242.867049623534,-242.42569985681),.UNSPECIFIED.);
#150=B_SPLINE_CURVE_WITH_KNOTS('',3,(#33099,#33100,#33101,#33102,#33103,
#33104,#33105,#33106,#33107,#33108,#33109,#33110,#33111,#33112,#33113,#33114,
#33115,#33116,#33117,#33118,#33119,#33120,#33121,#33122,#33123),
 .UNSPECIFIED.,.F.,.F.,(4,3,3,3,3,3,3,3,4),(239.198244907346,240.032792841697,
240.867340776048,241.701888710398,242.536436644749,243.3709845791,244.20553251345,
245.040080447801,245.481430214526),.UNSPECIFIED.);
#151=B_SPLINE_CURVE_WITH_KNOTS('',3,(#33128,#33129,#33130,#33131,#33132,
#33133,#33134,#33135,#33136,#33137,#33138,#33139,#33140,#33141,#33142,#33143,
#33144,#33145,#33146,#33147,#33148,#33149,#33150,#33151,#33152,#33153,#33154,
#33155),.UNSPECIFIED.,.F.,.F.,(4,3,3,3,3,3,3,3,3,4),(-254.992070471169,
-254.939218591863,-253.939456950326,-252.939695308789,-251.939933667253,
-251.440052846484,-250.940172025716,-249.940410384179,-248.940648742643,
-248.708885163989),.UNSPECIFIED.);
#152=B_SPLINE_CURVE_WITH_KNOTS('',3,(#33156,#33157,#33158,#33159,#33160,
#33161,#33162,#33163,#33164,#33165,#33166,#33167,#33168,#33169,#33170,#33171,
#33172,#33173,#33174,#33175,#33176,#33177,#33178,#33179,#33180),
 .UNSPECIFIED.,.F.,.F.,(4,3,3,3,3,3,3,3,4),(245.481430214526,245.941363818033,
246.941125459569,247.940887101106,248.940648742643,249.940410384179,250.940172025716,
251.440052846485,251.764615521705),.UNSPECIFIED.);
#153=B_SPLINE_CURVE_WITH_KNOTS('',3,(#33185,#33186,#33187,#33188,#33189,
#33190,#33191,#33192,#33193,#33194,#33195,#33196,#33197,#33198,#33199,#33200,
#33201,#33202,#33203,#33204,#33205,#33206,#33207,#33208,#33209),
 .UNSPECIFIED.,.F.,.F.,(4,3,3,3,3,3,3,3,4),(-261.275255778348,-260.937788441083,
-259.938026799546,-258.93826515801,-258.438384337241,-257.938503516473,
-256.938741874936,-255.9389802334,-254.992070471169),.UNSPECIFIED.);
#154=B_SPLINE_CURVE_WITH_KNOTS('',3,(#33210,#33211,#33212,#33213,#33214,
#33215,#33216,#33217,#33218,#33219,#33220,#33221,#33222,#33223,#33224,#33225,
#33226,#33227,#33228,#33229,#33230,#33231,#33232,#33233,#33234),
 .UNSPECIFIED.,.F.,.F.,(4,3,3,3,3,3,3,3,4),(251.764615521705,252.599163456056,
253.433711390407,254.268259324758,255.102807259108,255.937355193459,256.77190312781,
257.606451062161,258.047800828885),.UNSPECIFIED.);
#155=B_SPLINE_CURVE_WITH_KNOTS('',3,(#33239,#33240,#33241,#33242,#33243,
#33244,#33245,#33246,#33247,#33248,#33249,#33250,#33251,#33252,#33253,#33254,
#33255,#33256,#33257,#33258,#33259,#33260,#33261,#33262,#33263),
 .UNSPECIFIED.,.F.,.F.,(4,3,3,3,3,3,3,3,4),(-267.558441085528,-266.723893151177,
-265.889345216826,-265.054797282476,-264.220249348125,-263.385701413774,
-262.551153479423,-261.716605545073,-261.275255778348),.UNSPECIFIED.);
#156=B_SPLINE_CURVE_WITH_KNOTS('',3,(#33264,#33265,#33266,#33267,#33268,
#33269,#33270,#33271,#33272,#33273,#33274,#33275,#33276,#33277,#33278,#33279,
#33280,#33281,#33282,#33283,#33284,#33285,#33286,#33287,#33288),
 .UNSPECIFIED.,.F.,.F.,(4,3,3,3,3,3,3,3,4),(258.047800828885,258.438384337242,
258.93826515801,259.938026799547,260.937788441083,261.93755008262,262.937311724157,
263.937073365694,264.330986136064),.UNSPECIFIED.);
#157=B_SPLINE_CURVE_WITH_KNOTS('',3,(#33293,#33294,#33295,#33296,#33297,
#33298,#33299,#33300,#33301,#33302,#33303,#33304,#33305,#33306,#33307,#33308,
#33309,#33310,#33311,#33312,#33313,#33314,#33315,#33316,#33317),
 .UNSPECIFIED.,.F.,.F.,(4,3,3,3,3,3,3,3,4),(-273.841626392707,-272.934928139524,
-272.435047318755,-271.935166497987,-270.93540485645,-269.935643214914,
-268.935881573377,-267.93611993184,-267.558441085528),.UNSPECIFIED.);
#158=B_SPLINE_CURVE_WITH_KNOTS('',3,(#33318,#33319,#33320,#33321,#33322,
#33323,#33324,#33325,#33326,#33327,#33328,#33329,#33330,#33331,#33332,#33333,
#33334,#33335,#33336,#33337,#33338,#33339,#33340,#33341,#33342),
 .UNSPECIFIED.,.F.,.F.,(4,3,3,3,3,3,3,3,4),(264.330986136064,265.165534070415,
266.000082004766,266.834629939117,267.669177873467,268.503725807818,269.338273742169,
270.17282167652,270.614171443244),.UNSPECIFIED.);
#159=B_SPLINE_CURVE_WITH_KNOTS('',3,(#33347,#33348,#33349,#33350,#33351,
#33352,#33353,#33354,#33355,#33356,#33357,#33358,#33359,#33360,#33361,#33362,
#33363,#33364,#33365,#33366,#33367,#33368,#33369,#33370,#33371),
 .UNSPECIFIED.,.F.,.F.,(4,3,3,3,3,3,3,3,4),(-280.124811699887,-279.290263765536,
-278.455715831186,-277.621167896835,-276.786619962484,-275.952072028133,
-275.117524093783,-274.282976159432,-273.841626392707),.UNSPECIFIED.);
#160=B_SPLINE_CURVE_WITH_KNOTS('',3,(#33372,#33373,#33374,#33375,#33376,
#33377,#33378,#33379,#33380,#33381,#33382,#33383,#33384,#33385,#33386,#33387,
#33388,#33389,#33390,#33391,#33392,#33393,#33394,#33395,#33396),
 .UNSPECIFIED.,.F.,.F.,(4,3,3,3,3,3,3,3,4),(270.614171443244,270.935404856451,
271.935166497987,272.435047318756,272.934928139524,273.934689781061,274.934451422597,
275.934213064134,276.897356750424),.UNSPECIFIED.);
#161=B_SPLINE_CURVE_WITH_KNOTS('',3,(#33401,#33402,#33403,#33404,#33405,
#33406,#33407,#33408,#33409,#33410,#33411,#33412,#33413,#33414,#33415,#33416,
#33417,#33418,#33419,#33420,#33421,#33422),.UNSPECIFIED.,.F.,.F.,(4,3,3,
3,3,3,3,4),(-286.407997007067,-285.931829479501,-284.932067837964,-283.932306196428,
-282.932544554891,-281.932782913354,-280.933021271817,-280.124811699887),
 .UNSPECIFIED.);
#162=B_SPLINE_CURVE_WITH_KNOTS('',3,(#33423,#33424,#33425,#33426,#33427,
#33428,#33429,#33430,#33431,#33432,#33433,#33434,#33435,#33436,#33437,#33438,
#33439,#33440,#33441,#33442,#33443,#33444,#33445,#33446,#33447,#33448,#33449,
#33450),.UNSPECIFIED.,.F.,.F.,(4,3,3,3,3,3,3,3,3,4),(276.897356750424,276.933974705671,
277.933736347208,278.933497988744,279.433378809513,279.933259630281,280.933021271818,
281.932782913354,282.932544554891,283.180542057603),.UNSPECIFIED.);
#163=B_SPLINE_CURVE_WITH_KNOTS('',3,(#33455,#33456,#33457,#33458,#33459,
#33460,#33461,#33462,#33463,#33464,#33465,#33466,#33467,#33468,#33469,#33470,
#33471,#33472,#33473,#33474,#33475,#33476,#33477,#33478,#33479),
 .UNSPECIFIED.,.F.,.F.,(4,3,3,3,3,3,3,3,4),(-292.691182314246,-291.856634379895,
-291.022086445545,-290.187538511194,-289.352990576843,-288.518442642492,
-287.683894708141,-286.849346773791,-286.407997007067),.UNSPECIFIED.);
#164=B_SPLINE_CURVE_WITH_KNOTS('',3,(#33480,#33481,#33482,#33483,#33484,
#33485,#33486,#33487,#33488,#33489,#33490,#33491,#33492,#33493,#33494,#33495,
#33496,#33497,#33498,#33499,#33500,#33501,#33502,#33503,#33504),
 .UNSPECIFIED.,.F.,.F.,(4,3,3,3,3,3,3,3,4),(283.180542057603,283.932306196428,
284.932067837965,285.931829479501,286.43171030027,286.931591121038,287.931352762575,
288.931114404111,289.463727364783),.UNSPECIFIED.);
#165=B_SPLINE_CURVE_WITH_KNOTS('',3,(#33509,#33510,#33511,#33512,#33513,
#33514,#33515,#33516,#33517,#33518,#33519,#33520,#33521,#33522,#33523,#33524,
#33525,#33526,#33527,#33528,#33529,#33530,#33531,#33532,#33533),
 .UNSPECIFIED.,.F.,.F.,(4,3,3,3,3,3,3,3,4),(-298.974367621426,-298.139819687075,
-297.305271752724,-296.470723818374,-295.636175884023,-294.801627949672,
-293.967080015322,-293.132532080971,-292.691182314246),.UNSPECIFIED.);
#166=B_SPLINE_CURVE_WITH_KNOTS('',3,(#33534,#33535,#33536,#33537,#33538,
#33539,#33540,#33541,#33542,#33543,#33544,#33545,#33546,#33547,#33548,#33549,
#33550,#33551,#33552,#33553,#33554,#33555,#33556,#33557,#33558),
 .UNSPECIFIED.,.F.,.F.,(4,3,3,3,3,3,3,3,4),(289.463727364783,290.298275299133,
291.132823233484,291.967371167835,292.801919102186,293.636467036536,294.471014970887,
295.305562905238,295.746912671962),.UNSPECIFIED.);
#167=B_SPLINE_CURVE_WITH_KNOTS('',3,(#33563,#33564,#33565,#33566,#33567,
#33568,#33569,#33570,#33571,#33572,#33573,#33574,#33575,#33576,#33577,#33578,
#33579,#33580,#33581,#33582,#33583,#33584,#33585,#33586,#33587),
 .UNSPECIFIED.,.F.,.F.,(4,3,3,3,3,3,3,3,4),(-305.257552928605,-304.423004994254,
-303.588457059904,-302.753909125553,-301.919361191202,-301.084813256852,
-300.250265322501,-299.41571738815,-298.974367621426),.UNSPECIFIED.);
#168=B_SPLINE_CURVE_WITH_KNOTS('',3,(#33588,#33589,#33590,#33591,#33592,
#33593,#33594,#33595,#33596,#33597,#33598,#33599,#33600,#33601,#33602,#33603,
#33604,#33605,#33606,#33607,#33608,#33609,#33610,#33611,#33612),
 .UNSPECIFIED.,.F.,.F.,(4,3,3,3,3,3,3,3,4),(295.746912671962,296.581460606313,
297.416008540664,298.250556475015,299.085104409365,299.919652343716,300.754200278067,
301.588748212418,302.030097979142),.UNSPECIFIED.);
#169=B_SPLINE_CURVE_WITH_KNOTS('',3,(#33617,#33618,#33619,#33620,#33621,
#33622,#33623,#33624,#33625,#33626,#33627,#33628,#33629,#33630,#33631,#33632,
#33633,#33634,#33635,#33636,#33637,#33638,#33639,#33640,#33641),
 .UNSPECIFIED.,.F.,.F.,(4,3,3,3,3,3,3,3,4),(-311.540738235785,-310.706190301434,
-309.871642367083,-309.037094432733,-308.202546498382,-307.367998564031,
-306.533450629681,-305.69890269533,-305.257552928605),.UNSPECIFIED.);
#170=B_SPLINE_CURVE_WITH_KNOTS('',3,(#33642,#33643,#33644,#33645,#33646,
#33647,#33648,#33649,#33650,#33651,#33652,#33653,#33654,#33655,#33656,#33657,
#33658,#33659,#33660,#33661,#33662,#33663,#33664,#33665,#33666),
 .UNSPECIFIED.,.F.,.F.,(4,3,3,3,3,3,3,3,4),(302.030097979142,302.927777385626,
303.927539027162,304.927300668699,305.927062310236,306.926823951772,307.426704772541,
307.926585593309,308.313283286321),.UNSPECIFIED.);
#171=B_SPLINE_CURVE_WITH_KNOTS('',3,(#33671,#33672,#33673,#33674,#33675,
#33676,#33677,#33678,#33679,#33680,#33681,#33682,#33683,#33684,#33685,#33686,
#33687,#33688,#33689,#33690,#33691,#33692,#33693,#33694,#33695),
 .UNSPECIFIED.,.F.,.F.,(4,3,3,3,3,3,3,3,4),(-317.823923542964,-316.924440367139,
-315.924678725603,-314.924917084066,-314.425036263297,-313.925155442529,
-312.925393800992,-311.925632159456,-311.540738235785),.UNSPECIFIED.);
#172=B_SPLINE_CURVE_WITH_KNOTS('',3,(#33696,#33697,#33698,#33699,#33700,
#33701,#33702,#33703,#33704,#33705,#33706,#33707,#33708,#33709,#33710,#33711,
#33712,#33713,#33714,#33715,#33716,#33717,#33718,#33719,#33720),
 .UNSPECIFIED.,.F.,.F.,(4,3,3,3,3,3,3,3,4),(308.313283286321,309.147831220672,
309.982379155023,310.816927089373,311.651475023724,312.486022958075,313.320570892425,
314.155118826776,314.596468593501),.UNSPECIFIED.);
#173=B_SPLINE_CURVE_WITH_KNOTS('',3,(#33725,#33726,#33727,#33728,#33729,
#33730,#33731,#33732,#33733,#33734,#33735,#33736,#33737,#33738,#33739,#33740,
#33741,#33742,#33743,#33744,#33745,#33746,#33747,#33748,#33749),
 .UNSPECIFIED.,.F.,.F.,(4,3,3,3,3,3,3,3,4),(-324.107108850144,-323.272560915793,
-322.438012981442,-321.603465047092,-320.768917112741,-319.93436917839,
-319.09982124404,-318.265273309689,-317.823923542964),.UNSPECIFIED.);
#174=B_SPLINE_CURVE_WITH_KNOTS('',3,(#33750,#33751,#33752,#33753,#33754,
#33755,#33756,#33757,#33758,#33759,#33760,#33761,#33762,#33763,#33764,#33765,
#33766,#33767,#33768,#33769,#33770,#33771),.UNSPECIFIED.,.F.,.F.,(4,3,3,
3,3,3,3,4),(314.596468593501,314.924917084066,315.924678725603,316.92444036714,
317.924202008676,318.923963650213,319.92372529175,320.87965390068),
 .UNSPECIFIED.);
#175=B_SPLINE_CURVE_WITH_KNOTS('',3,(#33776,#33777,#33778,#33779,#33780,
#33781,#33782,#33783,#33784,#33785,#33786,#33787,#33788,#33789,#33790,#33791,
#33792,#33793,#33794,#33795,#33796,#33797),.UNSPECIFIED.,.F.,.F.,(4,3,3,
3,3,3,3,4),(-330.390294157323,-329.921341707117,-328.92158006558,-327.921818424043,
-326.922056782507,-325.92229514097,-324.922533499433,-324.107108850144),
 .UNSPECIFIED.);
#176=B_SPLINE_CURVE_WITH_KNOTS('',3,(#33798,#33799,#33800,#33801,#33802,
#33803,#33804,#33805,#33806,#33807,#33808,#33809,#33810,#33811,#33812,#33813,
#33814,#33815,#33816,#33817,#33818,#33819,#33820,#33821,#33822,#33823,#33824,
#33825),.UNSPECIFIED.,.F.,.F.,(4,3,3,3,3,3,3,3,3,4),(320.87965390068,320.923486933286,
321.923248574823,322.92301021636,323.422891037128,323.922771857897,324.922533499433,
325.92229514097,326.922056782507,327.16283920786),.UNSPECIFIED.);
#177=B_SPLINE_CURVE_WITH_KNOTS('',3,(#33830,#33831,#33832,#33833,#33834,
#33835,#33836,#33837,#33838,#33839,#33840,#33841,#33842,#33843,#33844,#33845,
#33846,#33847,#33848,#33849,#33850,#33851,#33852,#33853,#33854),
 .UNSPECIFIED.,.F.,.F.,(4,3,3,3,3,3,3,3,4),(-336.673479464503,-335.838931530152,
-335.004383595801,-334.169835661451,-333.3352877271,-332.500739792749,-331.666191858398,
-330.831643924048,-330.390294157323),.UNSPECIFIED.);
#178=B_SPLINE_CURVE_WITH_KNOTS('',3,(#33855,#33856,#33857,#33858,#33859,
#33860,#33861,#33862,#33863,#33864,#33865,#33866,#33867,#33868,#33869,#33870,
#33871,#33872,#33873,#33874,#33875,#33876,#33877,#33878,#33879),
 .UNSPECIFIED.,.F.,.F.,(4,3,3,3,3,3,3,3,4),(327.16283920786,327.921818424043,
328.92158006558,329.921341707117,330.421222527885,330.921103348654,331.92086499019,
332.920626631727,333.44602451504),.UNSPECIFIED.);
#179=B_SPLINE_CURVE_WITH_KNOTS('',3,(#33884,#33885,#33886,#33887,#33888,
#33889,#33890,#33891,#33892,#33893,#33894,#33895,#33896,#33897,#33898,#33899,
#33900,#33901,#33902,#33903,#33904,#33905,#33906,#33907,#33908),
 .UNSPECIFIED.,.F.,.F.,(4,3,3,3,3,3,3,3,4),(-342.956664771683,-342.122116837332,
-341.287568902981,-340.45302096863,-339.61847303428,-338.783925099929,-337.949377165578,
-337.114829231228,-336.673479464503),.UNSPECIFIED.);
#180=B_SPLINE_CURVE_WITH_KNOTS('',3,(#33909,#33910,#33911,#33912,#33913,
#33914,#33915,#33916,#33917,#33918,#33919,#33920,#33921,#33922,#33923,#33924,
#33925,#33926,#33927,#33928,#33929,#33930,#33931,#33932,#33933),
 .UNSPECIFIED.,.F.,.F.,(4,3,3,3,3,3,3,3,4),(333.44602451504,334.28057244939,
335.115120383741,335.949668318092,336.784216252443,337.618764186793,338.453312121144,
339.287860055495,339.729209822219),.UNSPECIFIED.);
#181=B_SPLINE_CURVE_WITH_KNOTS('',3,(#33938,#33939,#33940,#33941,#33942,
#33943,#33944,#33945,#33946,#33947,#33948,#33949,#33950,#33951,#33952,#33953,
#33954,#33955,#33956,#33957,#33958,#33959,#33960,#33961,#33962),
 .UNSPECIFIED.,.F.,.F.,(4,3,3,3,3,3,3,3,4),(-349.239850078862,-348.405302144511,
-347.570754210161,-346.73620627581,-345.901658341459,-345.067110407109,
-344.232562472758,-343.398014538407,-342.956664771683),.UNSPECIFIED.);
#182=B_SPLINE_CURVE_WITH_KNOTS('',3,(#33963,#33964,#33965,#33966,#33967,
#33968,#33969,#33970,#33971,#33972,#33973,#33974,#33975,#33976,#33977,#33978,
#33979,#33980,#33981,#33982,#33983,#33984,#33985,#33986,#33987),
 .UNSPECIFIED.,.F.,.F.,(4,3,3,3,3,3,3,3,4),(339.729209822219,340.56375775657,
341.398305690921,342.232853625271,343.067401559622,343.901949493973,344.736497428324,
345.571045362674,346.012395129399),.UNSPECIFIED.);
#183=B_SPLINE_CURVE_WITH_KNOTS('',3,(#33992,#33993,#33994,#33995,#33996,
#33997,#33998,#33999,#34000,#34001,#34002,#34003,#34004,#34005,#34006,#34007,
#34008,#34009,#34010,#34011,#34012,#34013,#34014,#34015,#34016),
 .UNSPECIFIED.,.F.,.F.,(4,3,3,3,3,3,3,3,4),(-355.523035386042,-354.688487451691,
-353.85393951734,-353.019391582989,-352.184843648639,-351.350295714288,
-350.515747779937,-349.681199845586,-349.239850078862),.UNSPECIFIED.);
#184=B_SPLINE_CURVE_WITH_KNOTS('',3,(#34017,#34018,#34019,#34020,#34021,
#34022,#34023,#34024,#34025,#34026,#34027,#34028,#34029,#34030,#34031,#34032,
#34033,#34034,#34035,#34036,#34037,#34038,#34039,#34040,#34041),
 .UNSPECIFIED.,.F.,.F.,(4,3,3,3,3,3,3,3,4),(346.012395129399,346.917289613241,
347.917051254778,348.916812896315,349.916574537851,350.916336179388,351.416217000156,
351.916097820925,352.295580436578),.UNSPECIFIED.);
#185=B_SPLINE_CURVE_WITH_KNOTS('',3,(#34046,#34047,#34048,#34049,#34050,
#34051,#34052,#34053,#34054,#34055,#34056,#34057,#34058,#34059,#34060,#34061,
#34062,#34063,#34064,#34065,#34066,#34067,#34068,#34069,#34070),
 .UNSPECIFIED.,.F.,.F.,(4,3,3,3,3,3,3,3,4),(-361.806220693221,-360.913952594755,
-359.914190953218,-358.914429311681,-358.414548490913,-357.914667670145,
-356.914906028608,-355.915144387071,-355.523035386042),.UNSPECIFIED.);
#186=B_SPLINE_CURVE_WITH_KNOTS('',3,(#34071,#34072,#34073,#34074,#34075,
#34076,#34077,#34078,#34079,#34080,#34081,#34082,#34083,#34084,#34085,#34086,
#34087,#34088,#34089,#34090,#34091,#34092,#34093,#34094,#34095),
 .UNSPECIFIED.,.F.,.F.,(4,3,3,3,3,3,3,3,4),(352.295580436578,353.130128370929,
353.96467630528,354.79922423963,355.633772173981,356.468320108332,357.302868042682,
358.137415977033,358.578765743758),.UNSPECIFIED.);
#187=B_SPLINE_CURVE_WITH_KNOTS('',3,(#34100,#34101,#34102,#34103,#34104,
#34105,#34106,#34107,#34108,#34109,#34110,#34111,#34112,#34113,#34114,#34115,
#34116,#34117,#34118,#34119,#34120,#34121,#34122,#34123,#34124),
 .UNSPECIFIED.,.F.,.F.,(4,3,3,3,3,3,3,3,4),(-368.089406000401,-367.25485806605,
-366.4203101317,-365.585762197349,-364.751214262998,-363.916666328648,-363.082118394297,
-362.247570459947,-361.806220693221),.UNSPECIFIED.);
#188=B_SPLINE_CURVE_WITH_KNOTS('',3,(#34125,#34126,#34127,#34128,#34129,
#34130,#34131,#34132,#34133,#34134,#34135,#34136,#34137,#34138,#34139,#34140,
#34141,#34142,#34143,#34144,#34145,#34146),.UNSPECIFIED.,.F.,.F.,(4,3,3,
3,3,3,3,4),(358.578765743758,358.914429311682,359.914190953219,360.913952594755,
361.913714236292,362.913475877829,363.913237519365,364.861951050937),
 .UNSPECIFIED.);
#189=B_SPLINE_CURVE_WITH_KNOTS('',3,(#34151,#34152,#34153,#34154,#34155,
#34156,#34157,#34158,#34159,#34160,#34161,#34162,#34163,#34164,#34165,#34166,
#34167,#34168,#34169,#34170,#34171,#34172,#34173,#34174,#34175),
 .UNSPECIFIED.,.F.,.F.,(4,3,3,3,3,3,3,3,4),(-374.37259130758,-373.53804337323,
-372.703495438879,-371.868947504528,-371.034399570178,-370.199851635827,
-369.365303701476,-368.530755767125,-368.089406000401),.UNSPECIFIED.);
#190=B_SPLINE_CURVE_WITH_KNOTS('',3,(#34176,#34177,#34178,#34179,#34180,
#34181,#34182,#34183,#34184,#34185,#34186,#34187,#34188,#34189,#34190,#34191,
#34192,#34193,#34194,#34195,#34196,#34197,#34198,#34199,#34200),
 .UNSPECIFIED.,.F.,.F.,(4,3,3,3,3,3,3,3,4),(364.861951050937,365.696498985288,
366.531046919639,367.36559485399,368.200142788341,369.034690722691,369.869238657042,
370.703786591393,371.145136358117),.UNSPECIFIED.);
#191=B_SPLINE_CURVE_WITH_KNOTS('',3,(#34205,#34206,#34207,#34208,#34209,
#34210,#34211,#34212,#34213,#34214,#34215,#34216,#34217,#34218,#34219,#34220,
#34221,#34222,#34223,#34224,#34225,#34226,#34227,#34228,#34229),
 .UNSPECIFIED.,.F.,.F.,(4,3,3,3,3,3,3,3,4),(-380.65577661476,-379.821228680409,
-378.986680746059,-378.152132811708,-377.317584877357,-376.483036943007,
-375.648489008656,-374.813941074305,-374.37259130758),.UNSPECIFIED.);
#192=B_SPLINE_CURVE_WITH_KNOTS('',3,(#34230,#34231,#34232,#34233,#34234,
#34235,#34236,#34237,#34238,#34239,#34240,#34241,#34242,#34243,#34244,#34245,
#34246,#34247,#34248,#34249,#34250,#34251,#34252,#34253,#34254),
 .UNSPECIFIED.,.F.,.F.,(4,3,3,3,3,3,3,3,4),(371.145136358117,371.979684292468,
372.814232226818,373.648780161169,374.48332809552,375.31787602987,376.152423964221,
376.986971898572,377.428321665297),.UNSPECIFIED.);
#193=B_SPLINE_CURVE_WITH_KNOTS('',3,(#34259,#34260,#34261,#34262,#34263,
#34264,#34265,#34266,#34267,#34268,#34269,#34270,#34271,#34272,#34273,#34274,
#34275,#34276,#34277,#34278,#34279,#34280,#34281,#34282,#34283),
 .UNSPECIFIED.,.F.,.F.,(4,3,3,3,3,3,3,3,4),(-386.938961921939,-386.104413987589,
-385.269866053238,-384.435318118887,-383.600770184537,-382.766222250186,
-381.931674315835,-381.097126381484,-380.65577661476),.UNSPECIFIED.);
#194=B_SPLINE_CURVE_WITH_KNOTS('',3,(#34284,#34285,#34286,#34287,#34288,
#34289,#34290,#34291,#34292,#34293,#34294,#34295,#34296,#34297,#34298,#34299,
#34300,#34301,#34302,#34303,#34304,#34305,#34306,#34307,#34308),
 .UNSPECIFIED.,.F.,.F.,(4,3,3,3,3,3,3,3,4),(377.428321665297,378.262869599647,
379.097417533998,379.931965468349,380.7665134027,381.601061337051,382.435609271401,
383.270157205752,383.711506972476),.UNSPECIFIED.);
#195=B_SPLINE_CURVE_WITH_KNOTS('',3,(#34313,#34314,#34315,#34316,#34317,
#34318,#34319,#34320,#34321,#34322,#34323,#34324,#34325,#34326,#34327,#34328,
#34329,#34330,#34331,#34332,#34333,#34334),.UNSPECIFIED.,.F.,.F.,(4,3,3,
3,3,3,3,4),(-393.222147229119,-392.90632512393,-391.906563482393,-390.906801840856,
-389.90704019932,-388.907278557783,-387.907516916246,-386.938961921939),
 .UNSPECIFIED.);
#196=B_SPLINE_CURVE_WITH_KNOTS('',3,(#34335,#34336,#34337,#34338,#34339,
#34340,#34341,#34342,#34343,#34344,#34345,#34346,#34347,#34348,#34349,#34350,
#34351,#34352,#34353,#34354,#34355,#34356,#34357,#34358,#34359),
 .UNSPECIFIED.,.F.,.F.,(4,3,3,3,3,3,3,3,4),(383.711506972476,384.546054906827,
385.380602841178,386.215150775528,387.049698709879,387.88424664423,388.718794578581,
389.553342512931,389.994692279656),.UNSPECIFIED.);
#197=B_SPLINE_CURVE_WITH_KNOTS('',3,(#34364,#34365,#34366,#34367,#34368,
#34369,#34370,#34371,#34372,#34373,#34374,#34375,#34376,#34377,#34378,#34379,
#34380,#34381,#34382,#34383,#34384,#34385,#34386,#34387,#34388),
 .UNSPECIFIED.,.F.,.F.,(4,3,3,3,3,3,3,3,4),(-399.505332536299,-398.670784601948,
-397.836236667597,-397.001688733247,-396.167140798896,-395.332592864546,
-394.498044930195,-393.663496995844,-393.222147229119),.UNSPECIFIED.);
#198=B_SPLINE_CURVE_WITH_KNOTS('',3,(#34389,#34390,#34391,#34392,#34393,
#34394,#34395,#34396,#34397,#34398,#34399,#34400,#34401,#34402,#34403,#34404,
#34405,#34406,#34407,#34408,#34409,#34410,#34411,#34412,#34413),
 .UNSPECIFIED.,.F.,.F.,(4,3,3,3,3,3,3,3,4),(389.994692279656,390.906801840857,
391.906563482393,392.90632512393,393.406205944699,393.906086765467,394.905848407004,
395.90561004854,396.277877586835),.UNSPECIFIED.);
#199=B_SPLINE_CURVE_WITH_KNOTS('',3,(#34418,#34419,#34420,#34421,#34422,
#34423,#34424,#34425,#34426,#34427,#34428,#34429,#34430,#34431,#34432,#34433,
#34434,#34435,#34436,#34437,#34438,#34439,#34440,#34441,#34442),
 .UNSPECIFIED.,.F.,.F.,(4,3,3,3,3,3,3,3,4),(-405.788517843478,-404.90346482237,
-403.903703180834,-402.903941539297,-401.90417989776,-400.904418256223,
-400.404537435455,-399.904656614687,-399.505332536299),.UNSPECIFIED.);
#200=B_SPLINE_CURVE_WITH_KNOTS('',3,(#34443,#34444,#34445,#34446,#34447,
#34448,#34449,#34450,#34451,#34452,#34453,#34454,#34455,#34456,#34457,#34458,
#34459,#34460,#34461,#34462,#34463,#34464,#34465,#34466,#34467),
 .UNSPECIFIED.,.F.,.F.,(4,3,3,3,3,3,3,3,4),(396.277877586835,397.112425521186,
397.946973455537,398.781521389887,399.616069324238,400.450617258589,401.285165192939,
402.11971312729,402.561062894015),.UNSPECIFIED.);
#201=B_SPLINE_CURVE_WITH_KNOTS('',3,(#34472,#34473,#34474,#34475,#34476,
#34477,#34478,#34479,#34480,#34481,#34482,#34483,#34484,#34485,#34486,#34487,
#34488,#34489,#34490,#34491,#34492,#34493,#34494,#34495,#34496),
 .UNSPECIFIED.,.F.,.F.,(4,3,3,3,3,3,3,3,4),(-412.071703150658,-411.237155216307,
-410.402607281956,-409.568059347606,-408.733511413255,-407.898963478904,
-407.064415544553,-406.229867610203,-405.788517843478),.UNSPECIFIED.);
#202=B_SPLINE_CURVE_WITH_KNOTS('',3,(#34497,#34498,#34499,#34500,#34501,
#34502,#34503,#34504,#34505,#34506,#34507,#34508,#34509,#34510,#34511,#34512,
#34513,#34514,#34515,#34516,#34517,#34518,#34519,#34520,#34521),
 .UNSPECIFIED.,.F.,.F.,(4,3,3,3,3,3,3,3,4),(402.561062894015,402.903941539297,
403.903703180834,404.903464822371,405.903226463907,406.902988105444,407.402868926213,
407.902749746981,408.844248201194),.UNSPECIFIED.);
#203=B_SPLINE_CURVE_WITH_KNOTS('',3,(#34526,#34527,#34528,#34529,#34530,
#34531,#34532,#34533,#34534,#34535,#34536,#34537,#34538,#34539,#34540,#34541,
#34542,#34543,#34544,#34545,#34546,#34547,#34548,#34549,#34550),
 .UNSPECIFIED.,.F.,.F.,(4,3,3,3,3,3,3,3,4),(-418.354888457837,-417.520340523487,
-416.685792589136,-415.851244654785,-415.016696720434,-414.182148786084,
-413.347600851733,-412.513052917382,-412.071703150658),.UNSPECIFIED.);
#204=B_SPLINE_CURVE_WITH_KNOTS('',3,(#34551,#34552,#34553,#34554,#34555,
#34556,#34557,#34558,#34559,#34560,#34561,#34562,#34563,#34564,#34565,#34566,
#34567,#34568,#34569,#34570,#34571,#34572,#34573,#34574,#34575),
 .UNSPECIFIED.,.F.,.F.,(4,3,3,3,3,3,3,3,4),(408.844248201194,409.678796135545,
410.513344069896,411.347892004246,412.182439938597,413.016987872948,413.851535807298,
414.686083741649,415.127433508374),.UNSPECIFIED.);
#205=B_SPLINE_CURVE_WITH_KNOTS('',3,(#34580,#34581,#34582,#34583,#34584,
#34585,#34586,#34587,#34588,#34589,#34590,#34591,#34592,#34593,#34594,#34595,
#34596,#34597,#34598,#34599,#34600,#34601,#34602,#34603,#34604),
 .UNSPECIFIED.,.F.,.F.,(4,3,3,3,3,3,3,3,4),(-424.638073765017,-423.898936011568,
-422.899174370031,-421.899412728495,-421.399531907726,-420.899651086958,
-419.899889445421,-418.900127803884,-418.354888457837),.UNSPECIFIED.);
#206=B_SPLINE_CURVE_WITH_KNOTS('',3,(#34605,#34606,#34607,#34608,#34609,
#34610,#34611,#34612,#34613,#34614,#34615,#34616,#34617,#34618,#34619,#34620,
#34621,#34622,#34623,#34624,#34625,#34626,#34627,#34628,#34629),
 .UNSPECIFIED.,.F.,.F.,(4,3,3,3,3,3,3,3,4),(415.127433508374,415.961981442725,
416.796529377076,417.631077311426,418.465625245777,419.300173180128,420.134721114479,
420.969269048829,421.410618815554),.UNSPECIFIED.);
#207=B_SPLINE_CURVE_WITH_KNOTS('',3,(#34634,#34635,#34636,#34637,#34638,
#34639,#34640,#34641,#34642,#34643,#34644,#34645,#34646,#34647,#34648,#34649,
#34650,#34651,#34652,#34653,#34654,#34655,#34656,#34657,#34658,#34659,#34660,
#34661),.UNSPECIFIED.,.F.,.F.,(4,3,3,3,3,3,3,3,3,4),(-430.921259072197,
-430.897267502325,-429.897505860788,-428.897744219252,-428.397863398483,
-427.897982577715,-426.898220936178,-425.898459294641,-424.898697653105,
-424.638073765017),.UNSPECIFIED.);
#208=B_SPLINE_CURVE_WITH_KNOTS('',3,(#34662,#34663,#34664,#34665,#34666,
#34667,#34668,#34669,#34670,#34671,#34672,#34673,#34674,#34675,#34676,#34677,
#34678,#34679,#34680,#34681,#34682,#34683,#34684,#34685,#34686),
 .UNSPECIFIED.,.F.,.F.,(4,3,3,3,3,3,3,3,4),(421.410618815554,422.245166749904,
423.079714684255,423.914262618605,424.748810552956,425.583358487307,426.417906421657,
427.252454356008,427.693804122733),.UNSPECIFIED.);
#209=B_SPLINE_CURVE_WITH_KNOTS('',3,(#34691,#34692,#34693,#34694,#34695,
#34696,#34697,#34698,#34699,#34700,#34701,#34702,#34703,#34704,#34705,#34706,
#34707,#34708,#34709,#34710,#34711,#34712,#34713,#34714,#34715),
 .UNSPECIFIED.,.F.,.F.,(4,3,3,3,3,3,3,3,4),(-437.204444379376,-436.895837351545,
-435.896075710009,-435.39619488924,-434.896314068472,-433.896552426935,
-432.896790785398,-431.897029143862,-430.921259072197),.UNSPECIFIED.);
#210=B_SPLINE_CURVE_WITH_KNOTS('',3,(#34716,#34717,#34718,#34719,#34720,
#34721,#34722,#34723,#34724,#34725,#34726,#34727,#34728,#34729,#34730,#34731,
#34732,#34733,#34734,#34735,#34736,#34737,#34738,#34739,#34740),
 .UNSPECIFIED.,.F.,.F.,(4,3,3,3,3,3,3,3,4),(427.693804122733,428.528352057084,
429.362899991434,430.197447925785,431.031995860136,431.866543794486,432.701091728837,
433.535639663188,433.976989429913),.UNSPECIFIED.);
#211=B_SPLINE_CURVE_WITH_KNOTS('',3,(#34745,#34746,#34747,#34748,#34749,
#34750,#34751,#34752,#34753,#34754,#34755,#34756,#34757,#34758,#34759,#34760,
#34761,#34762,#34763,#34764,#34765,#34766,#34767,#34768,#34769),
 .UNSPECIFIED.,.F.,.F.,(4,3,3,3,3,3,3,3,4),(-443.487629686556,-442.653081752205,
-441.818533817854,-440.983985883503,-440.149437949153,-439.314890014802,
-438.480342080451,-437.645794146101,-437.204444379376),.UNSPECIFIED.);
#212=B_SPLINE_CURVE_WITH_KNOTS('',3,(#34770,#34771,#34772,#34773,#34774,
#34775,#34776,#34777,#34778,#34779,#34780,#34781,#34782,#34783,#34784,#34785,
#34786,#34787,#34788,#34789,#34790,#34791,#34792,#34793,#34794),
 .UNSPECIFIED.,.F.,.F.,(4,3,3,3,3,3,3,3,4),(433.976989429913,434.896314068472,
435.396194889241,435.896075710009,436.895837351546,437.895598993082,438.895360634619,
439.895122276156,440.260174737092),.UNSPECIFIED.);
#213=B_SPLINE_CURVE_WITH_KNOTS('',3,(#34799,#34800,#34801,#34802,#34803,
#34804,#34805,#34806,#34807,#34808,#34809,#34810,#34811,#34812,#34813,#34814,
#34815,#34816,#34817,#34818,#34819,#34820,#34821,#34822,#34823),
 .UNSPECIFIED.,.F.,.F.,(4,3,3,3,3,3,3,3,4),(-449.770814993735,-449.392857870754,
-448.892977049986,-447.893215408449,-446.893453766913,-445.893692125376,
-444.893930483839,-443.894168842302,-443.487629686556),.UNSPECIFIED.);
#214=B_SPLINE_CURVE_WITH_KNOTS('',3,(#34824,#34825,#34826,#34827,#34828,
#34829,#34830,#34831,#34832,#34833,#34834,#34835,#34836,#34837,#34838,#34839,
#34840,#34841,#34842,#34843,#34844,#34845,#34846,#34847,#34848),
 .UNSPECIFIED.,.F.,.F.,(4,3,3,3,3,3,3,3,4),(440.260174737092,441.094722671443,
441.929270605794,442.763818540144,443.598366474495,444.432914408846,445.267462343196,
446.102010277547,446.543360044272),.UNSPECIFIED.);
#215=B_SPLINE_CURVE_WITH_KNOTS('',3,(#34853,#34854,#34855,#34856,#34857,
#34858,#34859,#34860,#34861,#34862,#34863,#34864,#34865,#34866,#34867,#34868,
#34869,#34870,#34871,#34872,#34873,#34874,#34875,#34876,#34877),
 .UNSPECIFIED.,.F.,.F.,(4,3,3,3,3,3,3,3,4),(-456.054000300915,-455.219452366564,
-454.384904432213,-453.550356497862,-452.715808563511,-451.881260629161,
-451.04671269481,-450.212164760459,-449.770814993735),.UNSPECIFIED.);
#216=B_SPLINE_CURVE_WITH_KNOTS('',3,(#34878,#34879,#34880,#34881,#34882,
#34883,#34884,#34885,#34886,#34887,#34888,#34889,#34890,#34891,#34892,#34893,
#34894,#34895,#34896,#34897,#34898,#34899,#34900,#34901,#34902),
 .UNSPECIFIED.,.F.,.F.,(4,3,3,3,3,3,3,3,4),(446.543360044272,446.893453766913,
447.89321540845,448.892977049986,449.392857870755,449.892738691523,450.89250033306,
451.892261974596,452.826545351451),.UNSPECIFIED.);
#217=B_SPLINE_CURVE_WITH_KNOTS('',3,(#34907,#34908,#34909,#34910,#34911,
#34912,#34913,#34914,#34915,#34916,#34917,#34918,#34919,#34920,#34921,#34922,
#34923,#34924,#34925,#34926,#34927,#34928,#34929,#34930,#34931),
 .UNSPECIFIED.,.F.,.F.,(4,3,3,3,3,3,3,3,4),(-462.337185608094,-461.889878389963,
-460.890116748427,-459.89035510689,-458.890593465353,-457.890831823816,
-456.89107018228,-456.391189361511,-456.054000300915),.UNSPECIFIED.);
#218=B_SPLINE_CURVE_WITH_KNOTS('',3,(#34932,#34933,#34934,#34935,#34936,
#34937,#34938,#34939,#34940,#34941,#34942,#34943,#34944,#34945,#34946,#34947,
#34948,#34949,#34950,#34951,#34952,#34953,#34954,#34955,#34956,#34957,#34958,
#34959),.UNSPECIFIED.,.F.,.F.,(4,3,3,3,3,3,3,3,3,4),(452.826545351451,452.892023616133,
453.89178525767,454.891546899207,455.891308540743,456.391189361512,456.89107018228,
457.890831823817,458.890593465354,459.109730658631),.UNSPECIFIED.);
#219=B_SPLINE_CURVE_WITH_KNOTS('',3,(#34964,#34965,#34966,#34967,#34968,
#34969,#34970,#34971,#34972,#34973,#34974,#34975,#34976,#34977,#34978,#34979,
#34980,#34981,#34982,#34983,#34984,#34985,#34986,#34987,#34988),
 .UNSPECIFIED.,.F.,.F.,(4,3,3,3,3,3,3,3,4),(-468.620370915274,-467.785822980923,
-466.951275046573,-466.116727112222,-465.282179177871,-464.447631243521,
-463.61308330917,-462.778535374819,-462.337185608094),.UNSPECIFIED.);
#220=B_SPLINE_CURVE_WITH_KNOTS('',3,(#34989,#34990,#34991,#34992,#34993,
#34994,#34995,#34996,#34997,#34998,#34999,#35000,#35001,#35002,#35003,#35004,
#35005,#35006,#35007,#35008,#35009,#35010,#35011,#35012,#35013),
 .UNSPECIFIED.,.F.,.F.,(4,3,3,3,3,3,3,3,4),(459.109730658631,459.944278592982,
460.778826527332,461.613374461683,462.447922396034,463.282470330384,464.117018264735,
464.951566199086,465.392915965811),.UNSPECIFIED.);
#221=B_SPLINE_CURVE_WITH_KNOTS('',3,(#35018,#35019,#35020,#35021,#35022,
#35023,#35024,#35025,#35026,#35027,#35028,#35029,#35030,#35031,#35032,#35033,
#35034,#35035,#35036,#35037,#35038,#35039,#35040,#35041,#35042,#35043,#35044,
#35045),.UNSPECIFIED.,.F.,.F.,(4,3,3,3,3,3,3,3,3,4),(-474.903556222453,
-474.886779729941,-473.887018088404,-472.887256446867,-471.88749480533,
-470.887733163794,-470.387852343025,-469.887971522257,-468.88820988072,
-468.620370915274),.UNSPECIFIED.);
#222=B_SPLINE_CURVE_WITH_KNOTS('',3,(#35046,#35047,#35048,#35049,#35050,
#35051,#35052,#35053,#35054,#35055,#35056,#35057,#35058,#35059,#35060,#35061,
#35062,#35063,#35064,#35065,#35066,#35067,#35068,#35069,#35070),
 .UNSPECIFIED.,.F.,.F.,(4,3,3,3,3,3,3,3,4),(465.392915965811,466.227463900161,
467.062011834512,467.896559768863,468.731107703214,469.565655637564,470.400203571915,
471.234751506266,471.67610127299),.UNSPECIFIED.);
#223=B_SPLINE_CURVE_WITH_KNOTS('',3,(#35075,#35076,#35077,#35078,#35079,
#35080,#35081,#35082,#35083,#35084,#35085,#35086,#35087,#35088,#35089,#35090,
#35091,#35092,#35093,#35094,#35095,#35096,#35097,#35098,#35099),
 .UNSPECIFIED.,.F.,.F.,(4,3,3,3,3,3,3,3,4),(-481.186741529633,-480.885349579161,
-479.885587937624,-478.885826296087,-477.886064654551,-477.386183833782,
-476.886303013014,-475.886541371477,-474.903556222453),.UNSPECIFIED.);
#224=B_SPLINE_CURVE_WITH_KNOTS('',3,(#35100,#35101,#35102,#35103,#35104,
#35105,#35106,#35107,#35108,#35109,#35110,#35111,#35112,#35113,#35114,#35115,
#35116,#35117,#35118,#35119,#35120,#35121,#35122,#35123,#35124),
 .UNSPECIFIED.,.F.,.F.,(4,3,3,3,3,3,3,3,4),(471.67610127299,472.510649207341,
473.345197141692,474.179745076042,475.014293010393,475.848840944744,476.683388879095,
477.517936813446,477.95928658017),.UNSPECIFIED.);
#225=B_SPLINE_CURVE_WITH_KNOTS('',3,(#35129,#35130,#35131,#35132,#35133,
#35134,#35135,#35136,#35137,#35138,#35139,#35140,#35141,#35142,#35143,#35144,
#35145,#35146,#35147,#35148,#35149,#35150,#35151,#35152,#35153),
 .UNSPECIFIED.,.F.,.F.,(4,3,3,3,3,3,3,3,4),(-487.469926836813,-486.883919428381,
-485.884157786844,-484.884396145308,-484.384515324539,-483.884634503771,
-482.884872862234,-481.885111220698,-481.186741529633),.UNSPECIFIED.);
#226=B_SPLINE_CURVE_WITH_KNOTS('',3,(#35154,#35155,#35156,#35157,#35158,
#35159,#35160,#35161,#35162,#35163,#35164,#35165,#35166,#35167,#35168,#35169,
#35170,#35171,#35172,#35173,#35174,#35175),.UNSPECIFIED.,.F.,.F.,(4,3,3,
3,3,3,3,4),(477.95928658017,478.885826296088,479.885587937625,480.885349579161,
481.885111220698,482.884872862235,483.884634503771,484.242471887349),
 .UNSPECIFIED.);
#227=B_SPLINE_CURVE_WITH_KNOTS('',3,(#35180,#35181,#35182,#35183,#35184,
#35185,#35186,#35187,#35188,#35189,#35190,#35191,#35192,#35193,#35194,#35195,
#35196,#35197,#35198,#35199,#35200,#35201,#35202,#35203,#35204),
 .UNSPECIFIED.,.F.,.F.,(4,3,3,3,3,3,3,3,4),(-493.753112143992,-492.882489277601,
-491.882727636065,-491.382846815296,-490.882965994528,-489.883204352991,
-488.883442711455,-487.883681069918,-487.469926836813),.UNSPECIFIED.);
#228=B_SPLINE_CURVE_WITH_KNOTS('',3,(#35205,#35206,#35207,#35208,#35209,
#35210,#35211,#35212,#35213,#35214,#35215,#35216,#35217,#35218,#35219,#35220,
#35221,#35222,#35223,#35224,#35225,#35226,#35227,#35228,#35229),
 .UNSPECIFIED.,.F.,.F.,(4,3,3,3,3,3,3,3,4),(484.242471887349,485.0770198217,
485.91156775605,486.746115690401,487.580663624752,488.415211559102,489.249759493453,
490.084307427803,490.525657194529),.UNSPECIFIED.);
#229=B_SPLINE_CURVE_WITH_KNOTS('',3,(#35234,#35235,#35236,#35237,#35238,
#35239,#35240,#35241,#35242,#35243,#35244,#35245,#35246,#35247,#35248,#35249,
#35250,#35251,#35252,#35253,#35254,#35255,#35256,#35257,#35258),
 .UNSPECIFIED.,.F.,.F.,(4,3,3,3,3,3,3,3,4),(-500.036297451172,-499.201749516821,
-498.36720158247,-497.53265364812,-496.698105713769,-495.863557779418,-495.029009845068,
-494.194461910717,-493.753112143992),.UNSPECIFIED.);
#230=B_SPLINE_CURVE_WITH_KNOTS('',3,(#35259,#35260,#35261,#35262,#35263,
#35264,#35265,#35266,#35267,#35268,#35269,#35270,#35271,#35272,#35273,#35274,
#35275,#35276,#35277,#35278,#35279,#35280,#35281,#35282,#35283),
 .UNSPECIFIED.,.F.,.F.,(4,3,3,3,3,3,3,3,4),(490.525657194529,490.882965994528,
491.382846815297,491.882727636065,492.882489277602,493.882250919139,494.882012560675,
495.881774202212,496.808842501708),.UNSPECIFIED.);
#231=B_SPLINE_CURVE_WITH_KNOTS('',3,(#35288,#35289,#35290,#35291,#35292,
#35293,#35294,#35295,#35296,#35297,#35298,#35299,#35300,#35301,#35302,#35303,
#35304,#35305,#35306,#35307,#35308,#35309,#35310,#35311,#35312),
 .UNSPECIFIED.,.F.,.F.,(4,3,3,3,3,3,3,3,4),(-506.319482758351,-505.879390617579,
-505.37950979681,-504.879628976042,-503.879867334505,-502.880105692969,
-501.880344051432,-500.880582409895,-500.036297451172),.UNSPECIFIED.);
#232=B_SPLINE_CURVE_WITH_KNOTS('',3,(#35313,#35314,#35315,#35316,#35317,
#35318,#35319,#35320,#35321,#35322,#35323,#35324,#35325,#35326,#35327,#35328,
#35329,#35330,#35331,#35332,#35333,#35334,#35335,#35336,#35337),
 .UNSPECIFIED.,.F.,.F.,(4,3,3,3,3,3,3,3,4),(496.808842501708,497.643390436059,
498.47793837041,499.312486304761,500.147034239112,500.981582173463,501.816130107813,
502.650678042164,503.092027808888),.UNSPECIFIED.);
#233=B_SPLINE_CURVE_WITH_KNOTS('',3,(#35342,#35343,#35344,#35345,#35346,
#35347,#35348,#35349,#35350,#35351,#35352,#35353,#35354,#35355,#35356,#35357,
#35358,#35359,#35360,#35361,#35362,#35363,#35364,#35365,#35366),
 .UNSPECIFIED.,.F.,.F.,(4,3,3,3,3,3,3,3,4),(-512.602668065531,-511.76812013118,
-510.933572196829,-510.099024262479,-509.264476328128,-508.429928393777,
-507.595380459427,-506.760832525076,-506.319482758351),.UNSPECIFIED.);
#234=B_SPLINE_CURVE_WITH_KNOTS('',3,(#35367,#35368,#35369,#35370,#35371,
#35372,#35373,#35374,#35375,#35376,#35377,#35378,#35379,#35380,#35381,#35382,
#35383,#35384,#35385,#35386,#35387,#35388,#35389,#35390,#35391),
 .UNSPECIFIED.,.F.,.F.,(4,3,3,3,3,3,3,3,4),(503.092027808888,503.926575743239,
504.761123677589,505.59567161194,506.430219546291,507.264767480641,508.099315414992,
508.933863349343,509.375213116067),.UNSPECIFIED.);
#235=B_SPLINE_CURVE_WITH_KNOTS('',3,(#35396,#35397,#35398,#35399,#35400,
#35401,#35402,#35403,#35404,#35405,#35406,#35407,#35408,#35409,#35410,#35411,
#35412,#35413,#35414,#35415,#35416,#35417,#35418,#35419,#35420),
 .UNSPECIFIED.,.F.,.F.,(4,3,3,3,3,3,3,3,4),(-518.88585337271,-518.876291957556,
-517.876530316019,-516.876768674483,-515.877007032946,-514.877245391409,
-513.877483749872,-512.877722108336,-512.602668065531),.UNSPECIFIED.);
#236=B_SPLINE_CURVE_WITH_KNOTS('',3,(#35421,#35422,#35423,#35424,#35425,
#35426,#35427,#35428,#35429,#35430,#35431,#35432,#35433,#35434,#35435,#35436,
#35437,#35438,#35439,#35440,#35441,#35442,#35443,#35444,#35445),
 .UNSPECIFIED.,.F.,.F.,(4,3,3,3,3,3,3,3,4),(509.375213116067,509.878437183726,
510.878198825263,511.877960466799,512.377841287568,512.877722108336,513.877483749873,
514.87724539141,515.658398423247),.UNSPECIFIED.);
#237=B_SPLINE_CURVE_WITH_KNOTS('',3,(#35450,#35451,#35452,#35453,#35454,
#35455,#35456,#35457,#35458,#35459,#35460,#35461,#35462,#35463,#35464,#35465,
#35466,#35467,#35468,#35469,#35470,#35471,#35472,#35473,#35474),
 .UNSPECIFIED.,.F.,.F.,(4,3,3,3,3,3,3,3,4),(-525.16903867989,-524.874861806776,
-523.87510016524,-522.875338523703,-521.875576882166,-520.875815240629,
-519.876053599093,-519.376172778324,-518.88585337271),.UNSPECIFIED.);
#238=B_SPLINE_CURVE_WITH_KNOTS('',3,(#35475,#35476,#35477,#35478,#35479,
#35480,#35481,#35482,#35483,#35484,#35485,#35486,#35487,#35488,#35489,#35490,
#35491,#35492,#35493,#35494,#35495,#35496,#35497,#35498,#35499,#35500,#35501,
#35502),.UNSPECIFIED.,.F.,.F.,(4,3,3,3,3,3,3,3,3,4),(515.658398423247,515.877007032946,
516.876768674483,517.87653031602,518.876291957556,519.376172778325,519.876053599093,
520.87581524063,521.875576882167,521.941583730426),.UNSPECIFIED.);
#239=B_SPLINE_CURVE_WITH_KNOTS('',3,(#35507,#35508,#35509,#35510,#35511,
#35512,#35513,#35514,#35515,#35516,#35517,#35518,#35519,#35520,#35521,#35522,
#35523,#35524,#35525,#35526,#35527,#35528,#35529,#35530,#35531),
 .UNSPECIFIED.,.F.,.F.,(4,3,3,3,3,3,3,3,4),(-531.45222398707,-530.617676052719,
-529.783128118368,-528.948580184017,-528.114032249666,-527.279484315316,
-526.444936380965,-525.610388446614,-525.16903867989),.UNSPECIFIED.);
#240=B_SPLINE_CURVE_WITH_KNOTS('',3,(#35532,#35533,#35534,#35535,#35536,
#35537,#35538,#35539,#35540,#35541,#35542,#35543,#35544,#35545,#35546,#35547,
#35548,#35549,#35550,#35551,#35552,#35553,#35554,#35555,#35556),
 .UNSPECIFIED.,.F.,.F.,(4,3,3,3,3,3,3,3,4),(521.941583730426,522.875338523703,
523.87510016524,524.874861806777,525.874623448314,526.374504269082,526.87438508985,
527.874146731387,528.224769037606),.UNSPECIFIED.);
#241=B_SPLINE_CURVE_WITH_KNOTS('',3,(#35561,#35562,#35563,#35564,#35565,
#35566,#35567,#35568,#35569,#35570,#35571,#35572,#35573,#35574,#35575,#35576,
#35577,#35578,#35579,#35580,#35581,#35582,#35583,#35584,#35585),
 .UNSPECIFIED.,.F.,.F.,(4,3,3,3,3,3,3,3,4),(-537.735409294249,-536.872001505217,
-535.87223986368,-534.872478222144,-533.872716580607,-533.372835759838,
-532.87295493907,-531.873193297533,-531.45222398707),.UNSPECIFIED.);
#242=B_SPLINE_CURVE_WITH_KNOTS('',3,(#35586,#35587,#35588,#35589,#35590,
#35591,#35592,#35593,#35594,#35595,#35596,#35597,#35598,#35599,#35600,#35601,
#35602,#35603,#35604,#35605,#35606,#35607,#35608,#35609,#35610),
 .UNSPECIFIED.,.F.,.F.,(4,3,3,3,3,3,3,3,4),(528.224769037606,529.059316971957,
529.893864906308,530.728412840658,531.562960775009,532.39750870936,533.232056643711,
534.066604578062,534.507954344786),.UNSPECIFIED.);
#243=B_SPLINE_CURVE_WITH_KNOTS('',3,(#35615,#35616,#35617,#35618,#35619,
#35620,#35621,#35622,#35623,#35624,#35625,#35626,#35627,#35628,#35629,#35630,
#35631,#35632,#35633,#35634,#35635,#35636,#35637,#35638,#35639),
 .UNSPECIFIED.,.F.,.F.,(4,3,3,3,3,3,3,3,4),(-544.018594601429,-543.184046667078,
-542.349498732727,-541.514950798377,-540.680402864026,-539.845854929675,
-539.011306995325,-538.176759060974,-537.735409294249),.UNSPECIFIED.);
#244=B_SPLINE_CURVE_WITH_KNOTS('',3,(#35640,#35641,#35642,#35643,#35644,
#35645,#35646,#35647,#35648,#35649,#35650,#35651,#35652,#35653,#35654,#35655,
#35656,#35657,#35658,#35659,#35660,#35661,#35662,#35663,#35664),
 .UNSPECIFIED.,.F.,.F.,(4,3,3,3,3,3,3,3,4),(534.507954344786,534.872478222144,
535.872239863681,536.872001505217,537.871763146754,538.871524788291,539.871286429828,
540.371167250596,540.791139651965),.UNSPECIFIED.);
#245=B_SPLINE_CURVE_WITH_KNOTS('',3,(#35669,#35670,#35671,#35672,#35673,
#35674,#35675,#35676,#35677,#35678,#35679,#35680,#35681,#35682,#35683,#35684,
#35685,#35686,#35687,#35688,#35689,#35690,#35691,#35692,#35693),
 .UNSPECIFIED.,.F.,.F.,(4,3,3,3,3,3,3,3,4),(-550.301779908608,-549.868902845194,
-548.869141203658,-547.869379562121,-547.369498741352,-546.869617920584,
-545.869856279047,-544.870094637511,-544.018594601429),.UNSPECIFIED.);
#246=B_SPLINE_CURVE_WITH_KNOTS('',3,(#35694,#35695,#35696,#35697,#35698,
#35699,#35700,#35701,#35702,#35703,#35704,#35705,#35706,#35707,#35708,#35709,
#35710,#35711,#35712,#35713,#35714,#35715,#35716,#35717,#35718),
 .UNSPECIFIED.,.F.,.F.,(4,3,3,3,3,3,3,3,4),(540.791139651965,541.625687586316,
542.460235520667,543.294783455017,544.129331389368,544.963879323719,545.798427258069,
546.63297519242,547.074324959145),.UNSPECIFIED.);
#247=B_SPLINE_CURVE_WITH_KNOTS('',3,(#35723,#35724,#35725,#35726,#35727,
#35728,#35729,#35730,#35731,#35732,#35733,#35734,#35735,#35736,#35737,#35738,
#35739,#35740,#35741,#35742,#35743,#35744,#35745,#35746,#35747),
 .UNSPECIFIED.,.F.,.F.,(4,3,3,3,3,3,3,3,4),(-556.584965215788,-555.750417281437,
-554.915869347087,-554.081321412736,-553.246773478385,-552.412225544035,
-551.577677609684,-550.743129675333,-550.301779908608),.UNSPECIFIED.);
#248=B_SPLINE_CURVE_WITH_KNOTS('',3,(#35748,#35749,#35750,#35751,#35752,
#35753,#35754,#35755,#35756,#35757,#35758,#35759,#35760,#35761,#35762,#35763,
#35764,#35765,#35766,#35767,#35768,#35769,#35770,#35771,#35772),
 .UNSPECIFIED.,.F.,.F.,(4,3,3,3,3,3,3,3,4),(547.074324959145,547.369498741353,
547.869379562121,548.869141203658,549.868902845195,550.868664486731,551.868426128268,
552.868187769805,553.357510266324),.UNSPECIFIED.);
#249=B_SPLINE_CURVE_WITH_KNOTS('',3,(#35777,#35778,#35779,#35780,#35781,
#35782,#35783,#35784,#35785,#35786,#35787,#35788,#35789,#35790,#35791,#35792,
#35793,#35794,#35795,#35796,#35797,#35798,#35799,#35800,#35801),
 .UNSPECIFIED.,.F.,.F.,(4,3,3,3,3,3,3,3,4),(-562.868150522967,-562.033602588617,
-561.199054654266,-560.364506719915,-559.529958785564,-558.695410851214,
-557.860862916863,-557.026314982512,-556.584965215788),.UNSPECIFIED.);
#250=B_SPLINE_CURVE_WITH_KNOTS('',3,(#35802,#35803,#35804,#35805,#35806,
#35807,#35808,#35809,#35810,#35811,#35812,#35813,#35814,#35815,#35816,#35817,
#35818,#35819,#35820,#35821,#35822,#35823,#35824,#35825,#35826),
 .UNSPECIFIED.,.F.,.F.,(4,3,3,3,3,3,3,3,4),(553.357510266324,554.192058200675,
555.026606135026,555.861154069376,556.695702003727,557.530249938078,558.364797872428,
559.199345806779,559.640695573504),.UNSPECIFIED.);
#251=B_SPLINE_CURVE_WITH_KNOTS('',3,(#35831,#35832,#35833,#35834,#35835,
#35836,#35837,#35838,#35839,#35840,#35841,#35842,#35843,#35844,#35845,#35846,
#35847,#35848,#35849,#35850,#35851,#35852,#35853,#35854,#35855),
 .UNSPECIFIED.,.F.,.F.,(4,3,3,3,3,3,3,3,4),(-569.151335830147,-568.864374034392,
-568.364493213624,-567.864612392855,-566.864850751318,-565.865089109782,
-564.865327468245,-563.865565826708,-562.868150522967),.UNSPECIFIED.);
#252=B_SPLINE_CURVE_WITH_KNOTS('',3,(#35856,#35857,#35858,#35859,#35860,
#35861,#35862,#35863,#35864,#35865,#35866,#35867,#35868,#35869,#35870,#35871,
#35872,#35873,#35874,#35875,#35876,#35877,#35878,#35879,#35880),
 .UNSPECIFIED.,.F.,.F.,(4,3,3,3,3,3,3,3,4),(559.640695573504,560.475243507855,
561.309791442206,562.144339376557,562.978887310907,563.813435245258,564.647983179609,
565.48253111396,565.923880880684),.UNSPECIFIED.);
#253=B_SPLINE_CURVE_WITH_KNOTS('',3,(#35885,#35886,#35887,#35888,#35889,
#35890,#35891,#35892,#35893,#35894,#35895,#35896,#35897,#35898,#35899,#35900,
#35901,#35902,#35903,#35904,#35905,#35906,#35907,#35908,#35909),
 .UNSPECIFIED.,.F.,.F.,(4,3,3,3,3,3,3,3,4),(-575.434521137327,-574.599973202976,
-573.765425268625,-572.930877334275,-572.096329399924,-571.261781465573,
-570.427233531223,-569.592685596872,-569.151335830147),.UNSPECIFIED.);
#254=B_SPLINE_CURVE_WITH_KNOTS('',3,(#35910,#35911,#35912,#35913,#35914,
#35915,#35916,#35917,#35918,#35919,#35920,#35921,#35922,#35923,#35924,#35925,
#35926,#35927,#35928,#35929,#35930,#35931,#35932,#35933,#35934),
 .UNSPECIFIED.,.F.,.F.,(4,3,3,3,3,3,3,3,4),(565.923880880684,566.864850751319,
567.864612392856,568.364493213624,568.864374034392,569.864135675929,570.863897317466,
571.863658959003,572.207066187863),.UNSPECIFIED.);
#255=B_SPLINE_CURVE_WITH_KNOTS('',3,(#35939,#35940,#35941,#35942,#35943,
#35944,#35945,#35946,#35947,#35948,#35949,#35950,#35951,#35952,#35953,#35954,
#35955,#35956,#35957,#35958,#35959,#35960),.UNSPECIFIED.,.F.,.F.,(4,3,3,
3,3,3,3,4),(-581.717706444506,-580.861513732832,-579.861752091296,-578.861990449759,
-577.862228808222,-576.862467166686,-575.862705525149,-575.434521137327),
 .UNSPECIFIED.);
#256=B_SPLINE_CURVE_WITH_KNOTS('',3,(#35961,#35962,#35963,#35964,#35965,
#35966,#35967,#35968,#35969,#35970,#35971,#35972,#35973,#35974,#35975,#35976,
#35977,#35978,#35979,#35980,#35981,#35982,#35983,#35984,#35985),
 .UNSPECIFIED.,.F.,.F.,(4,3,3,3,3,3,3,3,4),(572.207066187863,572.863420600539,
573.863182242076,574.862943883613,575.362824704381,575.862705525149,576.862467166686,
577.862228808223,578.490251495043),.UNSPECIFIED.);
#257=B_SPLINE_CURVE_WITH_KNOTS('',3,(#35990,#35991,#35992,#35993,#35994,
#35995,#35996,#35997,#35998,#35999,#36000,#36001,#36002,#36003,#36004,#36005,
#36006,#36007,#36008,#36009,#36010,#36011,#36012,#36013,#36014),
 .UNSPECIFIED.,.F.,.F.,(4,3,3,3,3,3,3,3,4),(-588.000891751686,-587.166343817335,
-586.331795882984,-585.497247948633,-584.662700014282,-583.828152079931,
-582.99360414558,-582.159056211229,-581.717706444506),.UNSPECIFIED.);
#258=B_SPLINE_CURVE_WITH_KNOTS('',3,(#36015,#36016,#36017,#36018,#36019,
#36020,#36021,#36022,#36023,#36024,#36025,#36026,#36027,#36028,#36029,#36030,
#36031,#36032,#36033,#36034,#36035,#36036,#36037,#36038,#36039),
 .UNSPECIFIED.,.F.,.F.,(4,3,3,3,3,3,3,3,4),(578.490251495043,578.861990449759,
579.861752091296,580.861513732833,581.86127537437,582.361156195138,582.861037015906,
583.860798657443,584.773436802222),.UNSPECIFIED.);
#259=B_SPLINE_CURVE_WITH_KNOTS('',3,(#36044,#36045,#36046,#36047,#36048,
#36049,#36050,#36051,#36052,#36053,#36054,#36055,#36056,#36057,#36058,#36059,
#36060,#36061,#36062,#36063,#36064,#36065,#36066,#36067,#36068),
 .UNSPECIFIED.,.F.,.F.,(4,3,3,3,3,3,3,3,4),(-594.284077058865,-593.85841507281,
-592.858653431273,-591.858891789736,-590.8591301482,-589.859368506663,-589.359487685895,
-588.859606865126,-588.000891751686),.UNSPECIFIED.);
#260=B_SPLINE_CURVE_WITH_KNOTS('',3,(#36069,#36070,#36071,#36072,#36073,
#36074,#36075,#36076,#36077,#36078,#36079,#36080,#36081,#36082,#36083,#36084,
#36085,#36086,#36087,#36088,#36089,#36090,#36091,#36092,#36093),
 .UNSPECIFIED.,.F.,.F.,(4,3,3,3,3,3,3,3,4),(584.773436802222,585.607984736573,
586.442532670923,587.277080605274,588.111628539624,588.946176473975,589.780724408326,
590.615272342676,591.056622109402),.UNSPECIFIED.);
#261=B_SPLINE_CURVE_WITH_KNOTS('',3,(#36098,#36099,#36100,#36101,#36102,
#36103,#36104,#36105,#36106,#36107,#36108,#36109,#36110,#36111,#36112,#36113,
#36114,#36115,#36116,#36117,#36118,#36119,#36120,#36121,#36122),
 .UNSPECIFIED.,.F.,.F.,(4,3,3,3,3,3,3,3,4),(-600.567262366045,-599.732714431694,
-598.898166497343,-598.063618562993,-597.229070628642,-596.394522694291,
-595.559974759941,-594.72542682559,-594.284077058865),.UNSPECIFIED.);
#262=B_SPLINE_CURVE_WITH_KNOTS('',3,(#36123,#36124,#36125,#36126,#36127,
#36128,#36129,#36130,#36131,#36132,#36133,#36134,#36135,#36136,#36137,#36138,
#36139,#36140,#36141,#36142,#36143,#36144,#36145,#36146,#36147),
 .UNSPECIFIED.,.F.,.F.,(4,3,3,3,3,3,3,3,4),(591.056622109402,591.858891789737,
592.858653431274,593.85841507281,594.858176714347,595.857938355884,596.357819176652,
596.85769999742,597.339807416581),.UNSPECIFIED.);
#263=B_SPLINE_CURVE_WITH_KNOTS('',3,(#36152,#36153,#36154,#36155,#36156,
#36157,#36158,#36159,#36160,#36161,#36162,#36163,#36164,#36165,#36166,#36167,
#36168,#36169,#36170,#36171,#36172,#36173,#36174,#36175,#36176),
 .UNSPECIFIED.,.F.,.F.,(4,3,3,3,3,3,3,3,4),(-606.850447673224,-605.85555477125,
-604.855793129714,-603.856031488177,-603.356150667409,-602.85626984664,
-601.856508205104,-600.856746563567,-600.567262366045),.UNSPECIFIED.);
#264=B_SPLINE_CURVE_WITH_KNOTS('',3,(#36177,#36178,#36179,#36180,#36181,
#36182,#36183,#36184,#36185,#36186,#36187,#36188,#36189,#36190,#36191,#36192,
#36193,#36194,#36195,#36196,#36197,#36198,#36199,#36200,#36201),
 .UNSPECIFIED.,.F.,.F.,(4,3,3,3,3,3,3,3,4),(597.339807416581,598.174355350932,
599.008903285283,599.843451219633,600.677999153984,601.512547088335,602.347095022685,
603.181642957036,603.622992723761),.UNSPECIFIED.);
#265=B_SPLINE_CURVE_WITH_KNOTS('',3,(#36206,#36207,#36208,#36209,#36210,
#36211,#36212,#36213,#36214,#36215,#36216,#36217,#36218,#36219,#36220,#36221,
#36222,#36223,#36224,#36225,#36226,#36227,#36228,#36229,#36230,#36231,#36232,
#36233),.UNSPECIFIED.,.F.,.F.,(4,3,3,3,3,3,3,3,3,4),(-613.133632980404,
-612.853886262007,-611.854124620471,-610.854362978934,-610.354482158166,
-609.854601337397,-608.854839695861,-607.855078054324,-606.855316412787,
-606.850447673224),.UNSPECIFIED.);
#266=B_SPLINE_CURVE_WITH_KNOTS('',3,(#36234,#36235,#36236,#36237,#36238,
#36239,#36240,#36241,#36242,#36243,#36244,#36245,#36246,#36247,#36248,#36249,
#36250,#36251,#36252,#36253,#36254,#36255,#36256,#36257,#36258),
 .UNSPECIFIED.,.F.,.F.,(4,3,3,3,3,3,3,3,4),(603.622992723761,604.457540658112,
605.292088592463,606.126636526814,606.961184461165,607.795732395515,608.630280329866,
609.464828264217,609.906178030941),.UNSPECIFIED.);
#267=B_SPLINE_CURVE_WITH_KNOTS('',3,(#36263,#36264,#36265,#36266,#36267,
#36268,#36269,#36270,#36271,#36272,#36273,#36274,#36275,#36276,#36277,#36278,
#36279,#36280,#36281,#36282,#36283,#36284,#36285,#36286,#36287),
 .UNSPECIFIED.,.F.,.F.,(4,3,3,3,3,3,3,3,4),(-619.416818287584,-618.582270353233,
-617.747722418882,-616.913174484532,-616.078626550181,-615.24407861583,
-614.40953068148,-613.574982747129,-613.133632980404),.UNSPECIFIED.);
#268=B_SPLINE_CURVE_WITH_KNOTS('',3,(#36288,#36289,#36290,#36291,#36292,
#36293,#36294,#36295,#36296,#36297,#36298,#36299,#36300,#36301,#36302,#36303,
#36304,#36305,#36306,#36307,#36308,#36309,#36310,#36311,#36312),
 .UNSPECIFIED.,.F.,.F.,(4,3,3,3,3,3,3,3,4),(609.906178030941,610.354482158166,
610.854362978934,611.854124620471,612.853886262008,613.853647903545,614.853409545081,
615.853171186618,616.18936333812),.UNSPECIFIED.);
#269=B_SPLINE_CURVE_WITH_KNOTS('',3,(#36317,#36318,#36319,#36320,#36321,
#36322,#36323,#36324,#36325,#36326,#36327,#36328,#36329,#36330,#36331,#36332,
#36333,#36334,#36335,#36336,#36337,#36338,#36339,#36340,#36341),
 .UNSPECIFIED.,.F.,.F.,(4,3,3,3,3,3,3,3,4),(-625.700003594763,-624.865455660412,
-624.030907726062,-623.196359791711,-622.36181185736,-621.527263923009,
-620.692715988658,-619.858168054308,-619.416818287584),.UNSPECIFIED.);
#270=B_SPLINE_CURVE_WITH_KNOTS('',3,(#36342,#36343,#36344,#36345,#36346,
#36347,#36348,#36349,#36350,#36351,#36352,#36353,#36354,#36355,#36356,#36357,
#36358,#36359,#36360,#36361,#36362,#36363,#36364,#36365,#36366),
 .UNSPECIFIED.,.F.,.F.,(4,3,3,3,3,3,3,3,4),(616.18936333812,617.023911272471,
617.858459206821,618.693007141172,619.527555075523,620.362103009873,621.196650944224,
622.031198878575,622.4725486453),.UNSPECIFIED.);
#271=B_SPLINE_CURVE_WITH_KNOTS('',3,(#36373,#36374,#36375,#36376,#36377,
#36378,#36379,#36380,#36381,#36382,#36383,#36384,#36385,#36386,#36387,#36388,
#36389,#36390,#36391,#36392,#36393,#36394),.UNSPECIFIED.,.F.,.F.,(4,3,3,
3,3,3,3,4),(-630.849595809668,-630.015047875317,-629.180499940967,-628.345952006616,
-627.511404072265,-626.676856137915,-625.842308203564,-625.700003594763),
 .UNSPECIFIED.);
#272=B_SPLINE_CURVE_WITH_KNOTS('',3,(#36395,#36396,#36397,#36398,#36399,
#36400,#36401,#36402,#36403,#36404,#36405,#36406,#36407,#36408,#36409,#36410,
#36411,#36412,#36413,#36414,#36415,#36416,#36417,#36418,#36419),
 .UNSPECIFIED.,.F.,.F.,(4,3,3,3,3,3,3,3,4),(622.4725486453,622.851502677375,
623.851264318912,624.35114513968,624.851025960449,625.850787601985,626.850549243522,
627.850310885059,628.755733952479),.UNSPECIFIED.);
#273=B_SPLINE_CURVE_WITH_KNOTS('',3,(#36425,#36426,#36427,#36428,#36429,
#36430,#36431,#36432,#36433,#36434,#36435,#36436,#36437,#36438,#36439,#36440,
#36441),.UNSPECIFIED.,.F.,.F.,(4,1,1,1,1,1,1,1,1,1,1,1,1,1,4),(15.707963267949,
15.9832685139281,16.4771965724115,16.9711246308949,17.4650526893783,17.9589807478618,
18.4529088063452,18.9468368648286,19.440764923312,19.9346929817954,20.4286210402789,
20.9225490987623,21.4164771572457,21.9104052157291,21.9911485751284),
 .UNSPECIFIED.);
#274=B_SPLINE_CURVE_WITH_KNOTS('',3,(#36446,#36447,#36448,#36449,#36450),
 .UNSPECIFIED.,.F.,.F.,(4,1,4),(14.9954123969612,15.4893404554446,15.707963267949),
 .UNSPECIFIED.);
#275=B_SPLINE_CURVE_WITH_KNOTS('',3,(#36453,#36454,#36455,#36456,#36457,
#36458,#36459,#36460,#36461,#36462,#36463,#36464,#36465),.UNSPECIFIED.,
 .F.,.F.,(4,3,3,3,4),(-15.707963267949,-15.4479023213137,-14.9539744342492,
-14.4600465471847,-14.1765193863714),.UNSPECIFIED.);
#276=B_SPLINE_CURVE_WITH_KNOTS('',3,(#36470,#36471,#36472,#36473,#36474,
#36475,#36476,#36477,#36478,#36479,#36480,#36481,#36482,#36483,#36484,#36485),
 .UNSPECIFIED.,.F.,.F.,(4,1,1,1,1,1,1,1,1,1,1,1,1,4),(21.9911485751284,
22.4043332742125,22.898261332696,23.3921893911794,23.8861174496628,24.3800455081462,
24.8739735666297,25.3679016251131,25.8618296835965,26.3557577420799,26.8496858005633,
27.3436138590468,27.8375419175302,28.2743338823082),.UNSPECIFIED.);
#277=B_SPLINE_CURVE_WITH_KNOTS('',3,(#36486,#36487,#36488,#36489,#36490,
#36491,#36492,#36493,#36494,#36495,#36496,#36497,#36498,#36499,#36500,#36501,
#36502,#36503,#36504,#36505,#36506,#36507,#36508,#36509,#36510,#36511,#36512,
#36513,#36514,#36515,#36516,#36517,#36518,#36519,#36520,#36521,#36522,#36523,
#36524,#36525,#36526,#36527,#36528),.UNSPECIFIED.,.F.,.F.,(4,3,3,3,3,3,
3,3,3,3,3,3,3,3,4),(-21.9911485751284,-21.868964853152,-21.3750369660875,
-20.881109079023,-20.3871811919585,-19.893253304894,-19.3993254178296,-18.9053975307651,
-18.4114696437006,-17.9175417566361,-17.4236138695716,-16.9296859825071,
-16.4357580954427,-15.9418302083782,-15.707963267949),.UNSPECIFIED.);
#278=B_SPLINE_CURVE_WITH_KNOTS('',3,(#36533,#36534,#36535,#36536,#36537,
#36538,#36539,#36540,#36541,#36542,#36543,#36544,#36545,#36546,#36547,#36548,
#36549),.UNSPECIFIED.,.F.,.F.,(4,1,1,1,1,1,1,1,1,1,1,1,1,1,4),(28.2743338823082,
28.3314699760136,28.825398034497,29.3193260929804,29.8132541514639,30.3071822099473,
30.8011102684307,31.2950383269141,31.7889663853976,32.282894443881,32.7768225023644,
33.2707505608478,33.7646786193312,34.2586066778147,34.5575191894877),
 .UNSPECIFIED.);
#279=B_SPLINE_CURVE_WITH_KNOTS('',3,(#36550,#36551,#36552,#36553,#36554,
#36555,#36556,#36557,#36558,#36559,#36560,#36561,#36562,#36563,#36564,#36565,
#36566,#36567,#36568,#36569,#36570,#36571,#36572,#36573,#36574,#36575,#36576,
#36577,#36578,#36579,#36580,#36581,#36582,#36583,#36584,#36585,#36586,#36587,
#36588,#36589),.UNSPECIFIED.,.F.,.F.,(4,3,3,3,3,3,3,3,3,3,3,3,3,4),(-28.2743338823079,
-27.7960994979258,-27.3021716108613,-26.8082437237968,-26.3143158367323,
-25.8203879496678,-25.3264600626034,-24.8325321755389,-24.3386042884744,
-23.8446764014099,-23.3507485143454,-22.8568206272809,-22.3628927402165,
-21.9911485751284),.UNSPECIFIED.);
#280=B_SPLINE_CURVE_WITH_KNOTS('',3,(#36594,#36595,#36596,#36597,#36598,
#36599,#36600,#36601,#36602,#36603,#36604,#36605,#36606,#36607,#36608,#36609,
#36610),.UNSPECIFIED.,.F.,.F.,(4,1,1,1,1,1,1,1,1,1,1,1,1,1,4),(34.5575191894877,
34.7525347362981,35.2464627947815,35.7403908532649,36.2343189117483,36.7282469702318,
37.2221750287152,37.7161030871986,38.210031145682,38.7039592041655,39.1978872626489,
39.6918153211323,40.1857433796157,40.6796714380991,40.8407044966672),
 .UNSPECIFIED.);
#281=B_SPLINE_CURVE_WITH_KNOTS('',3,(#36611,#36612,#36613,#36614,#36615,
#36616,#36617,#36618,#36619,#36620,#36621,#36622,#36623,#36624,#36625,#36626,
#36627,#36628,#36629,#36630,#36631,#36632,#36633,#36634,#36635,#36636,#36637,
#36638,#36639,#36640,#36641,#36642,#36643,#36644,#36645,#36646,#36647,#36648,
#36649,#36650,#36651,#36652,#36653),.UNSPECIFIED.,.F.,.F.,(4,3,3,3,3,3,
3,3,3,3,3,3,3,3,4),(-34.5575191894877,-34.217162029764,-33.7232341426995,
-33.2293062556351,-32.7353783685706,-32.2414504815061,-31.7475225944416,
-31.2535947073771,-30.7596668203126,-30.2657389332482,-29.7718110461837,
-29.2778831591192,-28.7839552720547,-28.2900273849902,-28.2743338823079),
 .UNSPECIFIED.);
#282=B_SPLINE_CURVE_WITH_KNOTS('',3,(#36658,#36659,#36660,#36661,#36662,
#36663,#36664,#36665,#36666,#36667,#36668,#36669,#36670,#36671,#36672,#36673,
#36674),.UNSPECIFIED.,.F.,.F.,(4,1,1,1,1,1,1,1,1,1,1,1,1,1,4),(40.8407044966672,
41.1735994965826,41.667527555066,42.1614556135494,42.6553836720328,43.1493117305162,
43.6432397889997,44.1371678474831,44.6310959059665,45.1250239644499,45.6189520229333,
46.1128800814168,46.6068081399002,47.1007361983836,47.1238898038469),
 .UNSPECIFIED.);
#283=B_SPLINE_CURVE_WITH_KNOTS('',3,(#36675,#36676,#36677,#36678,#36679,
#36680,#36681,#36682,#36683,#36684,#36685,#36686,#36687,#36688,#36689,#36690,
#36691,#36692,#36693,#36694,#36695,#36696,#36697,#36698,#36699,#36700,#36701,
#36702,#36703,#36704,#36705,#36706,#36707,#36708,#36709,#36710,#36711,#36712,
#36713,#36714,#36715,#36716,#36717),.UNSPECIFIED.,.F.,.F.,(4,3,3,3,3,3,
3,3,3,3,3,3,3,3,4),(-40.8407044966672,-40.6382245616023,-40.1442966745378,
-39.6503687874733,-39.1564409004088,-38.6625130133444,-38.1685851262799,
-37.6746572392154,-37.1807293521509,-36.6868014650864,-36.1928735780219,
-35.6989456909575,-35.205017803893,-34.7110899168285,-34.5575191894877),
 .UNSPECIFIED.);
#284=B_SPLINE_CURVE_WITH_KNOTS('',3,(#36722,#36723,#36724,#36725,#36726,
#36727,#36728,#36729,#36730,#36731,#36732,#36733,#36734,#36735,#36736,#36737),
 .UNSPECIFIED.,.F.,.F.,(4,1,1,1,1,1,1,1,1,1,1,1,1,4),(47.1238898038469,
47.594664256867,48.0885923153505,48.5825203738339,49.0764484323173,49.5703764908007,
50.0643045492841,50.5582326077676,51.052160666251,51.5460887247344,52.0400167832178,
52.5339448417012,53.0278729001847,53.4070751110264),.UNSPECIFIED.);
#285=B_SPLINE_CURVE_WITH_KNOTS('',3,(#36738,#36739,#36740,#36741,#36742,
#36743,#36744,#36745,#36746,#36747,#36748,#36749,#36750,#36751,#36752,#36753,
#36754,#36755,#36756,#36757,#36758,#36759,#36760,#36761,#36762,#36763,#36764,
#36765,#36766,#36767,#36768,#36769,#36770,#36771,#36772,#36773,#36774,#36775,
#36776,#36777,#36778,#36779,#36780),.UNSPECIFIED.,.F.,.F.,(4,3,3,3,3,3,
3,3,3,3,3,3,3,3,4),(-47.1238898038469,-47.0592870934406,-46.5653592063761,
-46.0714313193116,-45.5775034322471,-45.0835755451826,-44.5896476581181,
-44.0957197710537,-43.6017918839892,-43.1078639969247,-42.6139361098602,
-42.1200082227957,-41.6260803357312,-41.1321524486668,-40.8407044966672),
 .UNSPECIFIED.);
#286=B_SPLINE_CURVE_WITH_KNOTS('',3,(#36785,#36786,#36787,#36788,#36789,
#36790,#36791,#36792,#36793,#36794,#36795,#36796,#36797,#36798,#36799,#36800,
#36801),.UNSPECIFIED.,.F.,.F.,(4,1,1,1,1,1,1,1,1,1,1,1,1,1,4),(53.4070751110264,
53.5218009586681,54.0157290171515,54.5096570756349,55.0035851341184,55.4975131926018,
55.9914412510852,56.4853693095686,56.979297368052,57.4732254265355,57.9671534850189,
58.4610815435023,58.9550096019857,59.4489376604691,59.6902604182061),
 .UNSPECIFIED.);
#287=B_SPLINE_CURVE_WITH_KNOTS('',3,(#36802,#36803,#36804,#36805,#36806,
#36807,#36808,#36809,#36810,#36811,#36812,#36813,#36814,#36815,#36816,#36817,
#36818,#36819,#36820,#36821,#36822,#36823,#36824,#36825,#36826,#36827,#36828,
#36829,#36830,#36831,#36832,#36833,#36834,#36835,#36836,#36837,#36838,#36839,
#36840,#36841),.UNSPECIFIED.,.F.,.F.,(4,3,3,3,3,3,3,3,3,3,3,3,3,4),(-53.4070751110264,
-52.9864217382143,-52.4924938511499,-51.9985659640854,-51.5046380770209,
-51.0107101899564,-50.5167823028919,-50.0228544158274,-49.528926528763,
-49.0349986416985,-48.541070754634,-48.0471428675695,-47.553214980505,-47.1238898038469),
 .UNSPECIFIED.);
#288=B_SPLINE_CURVE_WITH_KNOTS('',3,(#36846,#36847,#36848,#36849,#36850,
#36851,#36852,#36853,#36854,#36855,#36856,#36857,#36858,#36859,#36860,#36861,
#36862),.UNSPECIFIED.,.F.,.F.,(4,1,1,1,1,1,1,1,1,1,1,1,1,1,4),(59.6902604182061,
59.9428657189526,60.436793777436,60.9307218359194,61.4246498944028,61.9185779528863,
62.4125060113697,62.9064340698531,63.4003621283365,63.8942901868199,64.3882182453034,
64.8821463037868,65.3760743622702,65.8700024207536,65.9734457253856),
 .UNSPECIFIED.);
#289=B_SPLINE_CURVE_WITH_KNOTS('',3,(#36863,#36864,#36865,#36866,#36867,
#36868,#36869,#36870,#36871,#36872,#36873,#36874,#36875,#36876,#36877,#36878,
#36879,#36880,#36881,#36882,#36883,#36884,#36885,#36886,#36887,#36888,#36889,
#36890,#36891,#36892,#36893,#36894,#36895,#36896,#36897,#36898,#36899,#36900,
#36901,#36902,#36903,#36904,#36905),.UNSPECIFIED.,.F.,.F.,(4,3,3,3,3,3,
3,3,3,3,3,3,3,3,4),(-59.6902604182059,-59.4074842700526,-58.9135563829881,
-58.4196284959236,-57.9257006088591,-57.4317727217947,-56.9378448347302,
-56.4439169476657,-55.9499890606012,-55.4560611735367,-54.9621332864723,
-54.4682053994078,-53.9742775123433,-53.4803496252788,-53.4070751110264),
 .UNSPECIFIED.);
#290=B_SPLINE_CURVE_WITH_KNOTS('',3,(#36910,#36911,#36912,#36913,#36914,
#36915,#36916,#36917,#36918,#36919,#36920,#36921,#36922,#36923,#36924,#36925),
 .UNSPECIFIED.,.F.,.F.,(4,1,1,1,1,1,1,1,1,1,1,1,1,4),(65.9734457253856,
66.363930479237,66.8578585377205,67.3517865962039,67.8457146546873,68.3396427131707,
68.8335707716542,69.3274988301376,69.821426888621,70.3153549471044,70.8092830055878,
71.3032110640713,71.7971391225547,72.2566310325653),.UNSPECIFIED.);
#291=B_SPLINE_CURVE_WITH_KNOTS('',3,(#36926,#36927,#36928,#36929,#36930,
#36931,#36932,#36933,#36934,#36935,#36936,#36937,#36938,#36939,#36940,#36941,
#36942,#36943,#36944,#36945,#36946,#36947,#36948,#36949,#36950,#36951,#36952,
#36953,#36954,#36955,#36956,#36957,#36958,#36959,#36960,#36961,#36962,#36963,
#36964,#36965,#36966,#36967,#36968),.UNSPECIFIED.,.F.,.F.,(4,3,3,3,3,3,
3,3,3,3,3,3,3,3,4),(-65.9734457253856,-65.8285468018909,-65.3346189148264,
-64.8406910277619,-64.3467631406974,-63.8528352536329,-63.3589073665684,
-62.864979479504,-62.3710515924395,-61.877123705375,-61.3831958183105,-60.889267931246,
-60.3953400441816,-59.9014121571171,-59.6902604182059),.UNSPECIFIED.);
#292=B_SPLINE_CURVE_WITH_KNOTS('',3,(#36975,#36976,#36977,#36978,#36979,
#36980,#36981,#36982,#36983,#36984,#36985,#36986),.UNSPECIFIED.,.F.,.F.,
(4,1,1,1,1,1,1,1,1,4),(72.2566310325653,72.2910671810381,72.7849952395215,
73.2789232980049,73.7728513564884,74.2667794149718,74.7607074734552,75.2546355319386,
75.748563590422,76.0320696667063),.UNSPECIFIED.);
#293=B_SPLINE_CURVE_WITH_KNOTS('',3,(#36987,#36988,#36989,#36990,#36991,
#36992,#36993,#36994,#36995,#36996,#36997,#36998,#36999,#37000,#37001,#37002,
#37003,#37004,#37005,#37006,#37007,#37008,#37009,#37010,#37011,#37012,#37013,
#37014,#37015,#37016,#37017,#37018,#37019,#37020,#37021,#37022,#37023,#37024,
#37025,#37026,#37027,#37028,#37029),.UNSPECIFIED.,.F.,.F.,(4,3,3,3,3,3,
3,3,3,3,3,3,3,3,4),(-72.2566310325651,-72.2496093337291,-71.7556814466647,
-71.2617535596002,-70.7678256725357,-70.2738977854712,-69.7799698984067,
-69.2860420113422,-68.7921141242778,-68.2981862372133,-67.8042583501488,
-67.3103304630843,-66.8164025760198,-66.3224746889554,-65.9734457253856),
 .UNSPECIFIED.);
#294=B_SPLINE_CURVE_WITH_KNOTS('',3,(#37035,#37036,#37037,#37038,#37039,
#37040,#37041,#37042,#37043,#37044,#37045,#37046),.UNSPECIFIED.,.F.,.F.,
(4,1,1,1,1,1,1,1,1,4),(72.2566310325653,72.2910671810381,72.7849952395215,
73.2789232980049,73.7728513564884,74.2667794149718,74.7607074734552,75.2546355319386,
75.748563590422,76.2424703929574),.UNSPECIFIED.);
#295=B_SPLINE_CURVE_WITH_KNOTS('',3,(#37049,#37050,#37051,#37052,#37053,
#37054,#37055,#37056,#37057),.UNSPECIFIED.,.F.,.F.,(4,1,1,1,1,1,4),(72.2566310325653,
72.7435372207936,73.2374651078581,73.7313929949226,74.2253208819871,74.7192487690515,
75.0027759298649),.UNSPECIFIED.);
#296=B_SPLINE_CURVE_WITH_KNOTS('',3,(#37062,#37063,#37064,#37065,#37066,
#37067,#37068,#37069,#37070,#37071,#37072,#37073,#37074,#37075,#37076,#37077),
 .UNSPECIFIED.,.F.,.F.,(4,1,1,1,1,1,1,1,1,1,1,1,1,4),(65.9734457253856,
66.363930479237,66.8578585377205,67.3517865962039,67.8457146546873,68.3396427131707,
68.8335707716542,69.3274988301376,69.821426888621,70.3153549471044,70.8092830055878,
71.3032110640713,71.7971391225547,72.2566310325653),.UNSPECIFIED.);
#297=B_SPLINE_CURVE_WITH_KNOTS('',3,(#37078,#37079,#37080,#37081,#37082,
#37083,#37084,#37085,#37086,#37087,#37088,#37089,#37090,#37091,#37092,#37093,
#37094),.UNSPECIFIED.,.F.,.F.,(4,1,1,1,1,1,1,1,1,1,1,1,1,1,4),(65.9734457253856,
66.3224746889554,66.8164025760198,67.3103304630843,67.8042583501488,68.2981862372133,
68.7921141242778,69.2860420113422,69.7799698984067,70.2738977854712,70.7678256725357,
71.2617535596002,71.7556814466647,72.2496093337291,72.2566310325653),
 .UNSPECIFIED.);
#298=B_SPLINE_CURVE_WITH_KNOTS('',3,(#37099,#37100,#37101,#37102,#37103,
#37104,#37105,#37106,#37107,#37108,#37109,#37110,#37111,#37112,#37113,#37114,
#37115),.UNSPECIFIED.,.F.,.F.,(4,1,1,1,1,1,1,1,1,1,1,1,1,1,4),(59.6902604182061,
59.9428657189526,60.436793777436,60.9307218359194,61.4246498944028,61.9185779528863,
62.4125060113697,62.9064340698531,63.4003621283365,63.8942901868199,64.3882182453034,
64.8821463037868,65.3760743622702,65.8700024207536,65.9734457253856),
 .UNSPECIFIED.);
#299=B_SPLINE_CURVE_WITH_KNOTS('',3,(#37116,#37117,#37118,#37119,#37120,
#37121,#37122,#37123,#37124,#37125,#37126,#37127,#37128,#37129,#37130,#37131,
#37132),.UNSPECIFIED.,.F.,.F.,(4,1,1,1,1,1,1,1,1,1,1,1,1,1,4),(59.6902604182061,
59.9014121571171,60.3953400441816,60.889267931246,61.3831958183105,61.877123705375,
62.3710515924395,62.864979479504,63.3589073665685,63.8528352536329,64.3467631406974,
64.8406910277619,65.3346189148264,65.8285468018909,65.9734457253856),
 .UNSPECIFIED.);
#300=B_SPLINE_CURVE_WITH_KNOTS('',3,(#37137,#37138,#37139,#37140,#37141,
#37142,#37143,#37144,#37145,#37146,#37147,#37148,#37149,#37150,#37151,#37152,
#37153),.UNSPECIFIED.,.F.,.F.,(4,1,1,1,1,1,1,1,1,1,1,1,1,1,4),(53.4070751110264,
53.5218009586681,54.0157290171515,54.5096570756349,55.0035851341184,55.4975131926018,
55.9914412510852,56.4853693095686,56.979297368052,57.4732254265355,57.9671534850189,
58.4610815435023,58.9550096019857,59.4489376604691,59.6902604182061),
 .UNSPECIFIED.);
#301=B_SPLINE_CURVE_WITH_KNOTS('',3,(#37154,#37155,#37156,#37157,#37158,
#37159,#37160,#37161,#37162,#37163,#37164,#37165,#37166,#37167,#37168,#37169,
#37170),.UNSPECIFIED.,.F.,.F.,(4,1,1,1,1,1,1,1,1,1,1,1,1,1,4),(53.4070751110264,
53.4803496252788,53.9742775123433,54.4682053994078,54.9621332864723,55.4560611735367,
55.9499890606012,56.4439169476657,56.9378448347302,57.4317727217947,57.9257006088591,
58.4196284959236,58.9135563829881,59.4074842700526,59.6902604182061),
 .UNSPECIFIED.);
#302=B_SPLINE_CURVE_WITH_KNOTS('',3,(#37175,#37176,#37177,#37178,#37179,
#37180,#37181,#37182,#37183,#37184,#37185,#37186,#37187,#37188,#37189,#37190),
 .UNSPECIFIED.,.F.,.F.,(4,1,1,1,1,1,1,1,1,1,1,1,1,4),(47.1238898038469,
47.594664256867,48.0885923153505,48.5825203738339,49.0764484323173,49.5703764908007,
50.0643045492841,50.5582326077676,51.052160666251,51.5460887247344,52.0400167832178,
52.5339448417012,53.0278729001847,53.4070751110264),.UNSPECIFIED.);
#303=B_SPLINE_CURVE_WITH_KNOTS('',3,(#37191,#37192,#37193,#37194,#37195,
#37196,#37197,#37198,#37199,#37200,#37201,#37202,#37203,#37204,#37205,#37206),
 .UNSPECIFIED.,.F.,.F.,(4,1,1,1,1,1,1,1,1,1,1,1,1,4),(47.1238898038469,
47.553214980505,48.0471428675695,48.541070754634,49.0349986416985,49.528926528763,
50.0228544158274,50.5167823028919,51.0107101899564,51.5046380770209,51.9985659640854,
52.4924938511499,52.9864217382143,53.4070751110264),.UNSPECIFIED.);
#304=B_SPLINE_CURVE_WITH_KNOTS('',3,(#37211,#37212,#37213,#37214,#37215,
#37216,#37217,#37218,#37219,#37220,#37221,#37222,#37223,#37224,#37225,#37226,
#37227),.UNSPECIFIED.,.F.,.F.,(4,1,1,1,1,1,1,1,1,1,1,1,1,1,4),(40.8407044966672,
41.1735994965826,41.667527555066,42.1614556135494,42.6553836720328,43.1493117305162,
43.6432397889997,44.1371678474831,44.6310959059665,45.1250239644499,45.6189520229333,
46.1128800814168,46.6068081399002,47.1007361983836,47.1238898038469),
 .UNSPECIFIED.);
#305=B_SPLINE_CURVE_WITH_KNOTS('',3,(#37228,#37229,#37230,#37231,#37232,
#37233,#37234,#37235,#37236,#37237,#37238,#37239,#37240,#37241,#37242,#37243,
#37244),.UNSPECIFIED.,.F.,.F.,(4,1,1,1,1,1,1,1,1,1,1,1,1,1,4),(40.8407044966672,
41.1321524486668,41.6260803357312,42.1200082227957,42.6139361098602,43.1078639969247,
43.6017918839892,44.0957197710537,44.5896476581181,45.0835755451826,45.5775034322471,
46.0714313193116,46.5653592063761,47.0592870934405,47.1238898038469),
 .UNSPECIFIED.);
#306=B_SPLINE_CURVE_WITH_KNOTS('',3,(#37249,#37250,#37251,#37252,#37253,
#37254,#37255,#37256,#37257,#37258,#37259,#37260,#37261,#37262,#37263,#37264,
#37265),.UNSPECIFIED.,.F.,.F.,(4,1,1,1,1,1,1,1,1,1,1,1,1,1,4),(34.5575191894877,
34.7525347362981,35.2464627947815,35.7403908532649,36.2343189117483,36.7282469702318,
37.2221750287152,37.7161030871986,38.210031145682,38.7039592041655,39.1978872626489,
39.6918153211323,40.1857433796157,40.6796714380991,40.8407044966672),
 .UNSPECIFIED.);
#307=B_SPLINE_CURVE_WITH_KNOTS('',3,(#37266,#37267,#37268,#37269,#37270,
#37271,#37272,#37273,#37274,#37275,#37276,#37277,#37278,#37279,#37280,#37281,
#37282),.UNSPECIFIED.,.F.,.F.,(4,1,1,1,1,1,1,1,1,1,1,1,1,1,4),(34.5575191894877,
34.7110899168285,35.205017803893,35.6989456909575,36.1928735780219,36.6868014650864,
37.1807293521509,37.6746572392154,38.1685851262799,38.6625130133444,39.1564409004088,
39.6503687874733,40.1442966745378,40.6382245616023,40.8407044966672),
 .UNSPECIFIED.);
#308=B_SPLINE_CURVE_WITH_KNOTS('',3,(#37287,#37288,#37289,#37290,#37291,
#37292,#37293,#37294,#37295,#37296,#37297,#37298,#37299,#37300,#37301,#37302,
#37303),.UNSPECIFIED.,.F.,.F.,(4,1,1,1,1,1,1,1,1,1,1,1,1,1,4),(28.2743338823082,
28.3314699760136,28.825398034497,29.3193260929804,29.8132541514639,30.3071822099473,
30.8011102684307,31.2950383269141,31.7889663853976,32.282894443881,32.7768225023644,
33.2707505608478,33.7646786193312,34.2586066778147,34.5575191894877),
 .UNSPECIFIED.);
#309=B_SPLINE_CURVE_WITH_KNOTS('',3,(#37304,#37305,#37306,#37307,#37308,
#37309,#37310,#37311,#37312,#37313,#37314,#37315,#37316,#37317,#37318,#37319,
#37320),.UNSPECIFIED.,.F.,.F.,(4,1,1,1,1,1,1,1,1,1,1,1,1,1,4),(28.2743338823082,
28.2900273849902,28.7839552720547,29.2778831591192,29.7718110461837,30.2657389332482,
30.7596668203126,31.2535947073771,31.7475225944416,32.2414504815061,32.7353783685706,
33.2293062556351,33.7232341426995,34.217162029764,34.5575191894877),
 .UNSPECIFIED.);
#310=B_SPLINE_CURVE_WITH_KNOTS('',3,(#37325,#37326,#37327,#37328,#37329,
#37330,#37331,#37332,#37333,#37334,#37335,#37336,#37337,#37338,#37339,#37340),
 .UNSPECIFIED.,.F.,.F.,(4,1,1,1,1,1,1,1,1,1,1,1,1,4),(21.9911485751284,
22.4043332742125,22.898261332696,23.3921893911794,23.8861174496628,24.3800455081462,
24.8739735666297,25.3679016251131,25.8618296835965,26.3557577420799,26.8496858005633,
27.3436138590468,27.8375419175302,28.2743338823082),.UNSPECIFIED.);
#311=B_SPLINE_CURVE_WITH_KNOTS('',3,(#37341,#37342,#37343,#37344,#37345,
#37346,#37347,#37348,#37349,#37350,#37351,#37352,#37353,#37354,#37355,#37356),
 .UNSPECIFIED.,.F.,.F.,(4,1,1,1,1,1,1,1,1,1,1,1,1,4),(21.9911485751284,
22.3628927402165,22.8568206272809,23.3507485143454,23.8446764014099,24.3386042884744,
24.8325321755389,25.3264600626033,25.8203879496678,26.3143158367323,26.8082437237968,
27.3021716108613,27.7960994979258,28.2743338823082),.UNSPECIFIED.);
#312=B_SPLINE_CURVE_WITH_KNOTS('',3,(#37361,#37362,#37363,#37364,#37365,
#37366,#37367,#37368,#37369,#37370,#37371,#37372,#37373,#37374,#37375,#37376,
#37377),.UNSPECIFIED.,.F.,.F.,(4,1,1,1,1,1,1,1,1,1,1,1,1,1,4),(15.707963267949,
15.9832685139281,16.4771965724115,16.9711246308949,17.4650526893783,17.9589807478618,
18.4529088063452,18.9468368648286,19.440764923312,19.9346929817954,20.4286210402789,
20.9225490987623,21.4164771572457,21.9104052157291,21.9911485751284),
 .UNSPECIFIED.);
#313=B_SPLINE_CURVE_WITH_KNOTS('',3,(#37378,#37379,#37380,#37381,#37382,
#37383,#37384,#37385,#37386,#37387,#37388,#37389,#37390,#37391,#37392,#37393,
#37394),.UNSPECIFIED.,.F.,.F.,(4,1,1,1,1,1,1,1,1,1,1,1,1,1,4),(15.707963267949,
15.9418302083782,16.4357580954427,16.9296859825072,17.4236138695716,17.9175417566361,
18.4114696437006,18.9053975307651,19.3993254178296,19.893253304894,20.3871811919585,
20.881109079023,21.3750369660875,21.868964853152,21.9911485751284),
 .UNSPECIFIED.);
#314=B_SPLINE_CURVE_WITH_KNOTS('',3,(#37400,#37401,#37402,#37403,#37404,
#37405,#37406,#37407,#37408),.UNSPECIFIED.,.F.,.F.,(4,1,1,1,1,1,4),(637.743308678727,
637.89409268595,638.893854327487,639.893615969023,640.89337761056,641.893139252097,
641.932632128719),.UNSPECIFIED.);
#315=B_SPLINE_CURVE_WITH_KNOTS('',3,(#37411,#37412,#37413,#37414,#37415,
#37416,#37417),.UNSPECIFIED.,.F.,.F.,(4,1,1,1,4),(637.743308678728,637.837647252847,
638.837408894383,639.337289715152,639.83717053592),.UNSPECIFIED.);
#316=B_SPLINE_CURVE_WITH_KNOTS('',3,(#37422,#37423,#37424,#37425,#37426,
#37427,#37428,#37429,#37430,#37431,#37432),.UNSPECIFIED.,.F.,.F.,(4,1,1,
1,1,1,1,1,4),(631.460123371548,631.895522836729,632.895284478266,633.895046119803,
634.89480776134,635.894569402876,636.394450223645,636.894331044413,637.743308678727),
 .UNSPECIFIED.);
#317=B_SPLINE_CURVE_WITH_KNOTS('',3,(#37433,#37434,#37435,#37436,#37437,
#37438,#37439,#37440,#37441,#37442,#37443),.UNSPECIFIED.,.F.,.F.,(4,1,1,
1,1,1,1,1,4),(631.460123371548,631.839077403626,632.838839045163,633.338719865931,
633.8386006867,634.838362328236,635.838123969773,636.83788561131,637.743308678728),
 .UNSPECIFIED.);
#318=B_SPLINE_CURVE_WITH_KNOTS('',3,(#37448,#37449,#37450,#37451,#37452,
#37453,#37454,#37455,#37456,#37457,#37458,#37459,#37460,#37461,#37462,#37463,
#37464,#37465,#37466,#37467,#37468,#37469),.UNSPECIFIED.,.F.,.F.,(4,3,3,
3,3,3,3,4),(625.176938064368,626.085415137985,626.993892211602,627.902369285219,
628.810846358836,629.719323432453,630.62780050607,631.460123371548),
 .UNSPECIFIED.);
#319=B_SPLINE_CURVE_WITH_KNOTS('',3,(#37470,#37471,#37472,#37473,#37474,
#37475,#37476,#37477,#37478,#37479,#37480),.UNSPECIFIED.,.F.,.F.,(4,1,1,
1,1,1,1,1,4),(625.176938064369,625.840507554406,626.340388375174,626.840269195943,
627.84003083748,628.839792479016,629.839554120553,630.83931576209,631.460123371548),
 .UNSPECIFIED.);
#320=B_SPLINE_CURVE_WITH_KNOTS('',3,(#37485,#37486,#37487,#37488,#37489,
#37490,#37491,#37492,#37493,#37494,#37495,#37496,#37497,#37498,#37499,#37500,
#37501,#37502,#37503,#37504,#37505,#37506,#37507,#37508,#37509,#37510,#37511,
#37512),.UNSPECIFIED.,.F.,.F.,(4,3,3,3,3,3,3,3,3,4),(618.893752757189,618.898621496752,
619.898383138289,620.898144779826,621.897906421362,622.397787242131,622.897668062899,
623.897429704436,624.897191345972,625.176938064368),.UNSPECIFIED.);
#321=B_SPLINE_CURVE_WITH_KNOTS('',3,(#37513,#37514,#37515,#37516,#37517,
#37518,#37519,#37520,#37521,#37522,#37523),.UNSPECIFIED.,.F.,.F.,(4,1,1,
1,1,1,1,1,4),(618.893752757189,619.342056884417,619.841937705186,620.841699346722,
621.841460988259,622.841222629796,623.840984271333,624.840745912869,625.176938064369),
 .UNSPECIFIED.);
#322=B_SPLINE_CURVE_WITH_KNOTS('',3,(#37528,#37529,#37530,#37531,#37532,
#37533,#37534,#37535,#37536,#37537,#37538,#37539,#37540,#37541,#37542,#37543,
#37544,#37545,#37546,#37547,#37548,#37549,#37550,#37551,#37552),
 .UNSPECIFIED.,.F.,.F.,(4,3,3,3,3,3,3,3,4),(612.610567450009,612.900051647532,
613.899813289069,614.899574930605,615.399455751374,615.899336572142,616.899098213679,
617.898859855216,618.893752757189),.UNSPECIFIED.);
#323=B_SPLINE_CURVE_WITH_KNOTS('',3,(#37553,#37554,#37555,#37556,#37557,
#37558,#37559,#37560,#37561,#37562,#37563,#37564,#37565,#37566,#37567,#37568,
#37569,#37570,#37571,#37572,#37573,#37574,#37575,#37576,#37577),
 .UNSPECIFIED.,.F.,.F.,(4,3,3,3,3,3,3,3,4),(612.61056745001,612.843606214429,
613.843367855966,614.843129497502,615.842891139039,616.842652780576,617.842414422112,
618.842176063649,618.893752757189),.UNSPECIFIED.);
#324=B_SPLINE_CURVE_WITH_KNOTS('',3,(#37582,#37583,#37584,#37585,#37586,
#37587,#37588,#37589,#37590,#37591,#37592,#37593,#37594,#37595,#37596,#37597,
#37598,#37599,#37600,#37601,#37602,#37603),.UNSPECIFIED.,.F.,.F.,(4,3,3,
3,3,3,3,4),(606.327382142829,607.235859216446,608.144336290063,609.05281336368,
609.961290437297,610.869767510914,611.778244584531,612.610567450009),
 .UNSPECIFIED.);
#325=B_SPLINE_CURVE_WITH_KNOTS('',3,(#37604,#37605,#37606,#37607,#37608,
#37609,#37610,#37611,#37612,#37613,#37614,#37615,#37616,#37617,#37618,#37619,
#37620,#37621,#37622,#37623,#37624,#37625,#37626,#37627,#37628),
 .UNSPECIFIED.,.F.,.F.,(4,3,3,3,3,3,3,3,4),(606.32738214283,606.845036365208,
607.844798006745,608.844559648282,609.844321289819,610.844082931355,611.843844572892,
612.343725393661,612.61056745001),.UNSPECIFIED.);
#326=B_SPLINE_CURVE_WITH_KNOTS('',3,(#37633,#37634,#37635,#37636,#37637,
#37638,#37639,#37640,#37641,#37642,#37643),.UNSPECIFIED.,.F.,.F.,(4,1,1,
1,1,1,1,1,4),(600.04419683565,600.902911949091,601.40279276986,601.902673590628,
602.902435232165,603.902196873701,604.901958515238,605.901720156775,606.327382142829),
 .UNSPECIFIED.);
#327=B_SPLINE_CURVE_WITH_KNOTS('',3,(#37644,#37645,#37646,#37647,#37648,
#37649,#37650,#37651,#37652,#37653,#37654),.UNSPECIFIED.,.F.,.F.,(4,1,1,
1,1,1,1,1,4),(600.044196835651,600.846466515988,601.846228157525,602.845989799061,
603.845751440598,604.845513082135,605.345393902903,605.845274723672,606.32738214283),
 .UNSPECIFIED.);
#328=B_SPLINE_CURVE_WITH_KNOTS('',3,(#37659,#37660,#37661,#37662,#37663,
#37664,#37665,#37666,#37667,#37668,#37669,#37670),.UNSPECIFIED.,.F.,.F.,
(4,1,1,1,1,1,1,1,1,4),(593.76101152847,593.904580458334,594.404461279103,
594.904342099871,595.904103741408,596.903865382944,597.903627024481,598.903388666018,
599.903150307555,600.04419683565),.UNSPECIFIED.);
#329=B_SPLINE_CURVE_WITH_KNOTS('',3,(#37671,#37672,#37673,#37674,#37675,
#37676,#37677,#37678,#37679,#37680,#37681,#37682),.UNSPECIFIED.,.F.,.F.,
(4,1,1,1,1,1,1,1,1,4),(593.761011528471,593.848135025231,594.847896666768,
595.847658308305,596.847419949841,597.847181591378,598.347062412146,598.846943232915,
599.846704874451,600.044196835651),.UNSPECIFIED.);
#330=B_SPLINE_CURVE_WITH_KNOTS('',3,(#37687,#37688,#37689,#37690,#37691,
#37692,#37693,#37694,#37695,#37696,#37697,#37698,#37699,#37700,#37701,#37702,
#37703,#37704,#37705,#37706,#37707,#37708),.UNSPECIFIED.,.F.,.F.,(4,3,3,
3,3,3,3,4),(587.477826221291,587.906010609114,588.905772250651,589.905533892187,
590.905295533724,591.905057175261,592.904818816798,593.76101152847),
 .UNSPECIFIED.);
#331=B_SPLINE_CURVE_WITH_KNOTS('',3,(#37709,#37710,#37711,#37712,#37713,
#37714,#37715,#37716,#37717,#37718,#37719),.UNSPECIFIED.,.F.,.F.,(4,1,1,
1,1,1,1,1,4),(587.477826221291,587.849565176011,588.849326817548,589.849088459084,
590.848850100621,591.348730921389,591.848611742158,592.848373383694,593.761011528471),
 .UNSPECIFIED.);
#332=B_SPLINE_CURVE_WITH_KNOTS('',3,(#37724,#37725,#37726,#37727,#37728,
#37729,#37730,#37731,#37732,#37733,#37734,#37735,#37736,#37737,#37738,#37739,
#37740,#37741,#37742,#37743,#37744,#37745,#37746,#37747,#37748),
 .UNSPECIFIED.,.F.,.F.,(4,3,3,3,3,3,3,3,4),(581.194640914111,581.907440759894,
582.90720240143,583.906964042967,584.906725684504,585.906487326041,586.906248967577,
587.406129788346,587.477826221291),.UNSPECIFIED.);
#333=B_SPLINE_CURVE_WITH_KNOTS('',3,(#37749,#37750,#37751,#37752,#37753,
#37754,#37755,#37756,#37757,#37758,#37759,#37760,#37761,#37762,#37763,#37764,
#37765,#37766,#37767,#37768,#37769,#37770,#37771,#37772,#37773),
 .UNSPECIFIED.,.F.,.F.,(4,3,3,3,3,3,3,3,4),(581.194640914112,581.850995326791,
582.850756968327,583.850518609864,584.350399430632,584.850280251401,585.850041892937,
586.849803534474,587.477826221291),.UNSPECIFIED.);
#334=B_SPLINE_CURVE_WITH_KNOTS('',3,(#37778,#37779,#37780,#37781,#37782,
#37783,#37784,#37785,#37786,#37787,#37788),.UNSPECIFIED.,.F.,.F.,(4,1,1,
1,1,1,1,1,4),(574.911455606932,575.908870910673,576.90863255221,577.908394193747,
578.908155835284,579.90791747682,580.407798297589,580.907679118357,581.194640914111),
 .UNSPECIFIED.);
#335=B_SPLINE_CURVE_WITH_KNOTS('',3,(#37789,#37790,#37791,#37792,#37793,
#37794,#37795,#37796,#37797,#37798,#37799,#37800,#37801,#37802,#37803,#37804,
#37805,#37806,#37807,#37808,#37809,#37810,#37811,#37812,#37813),
 .UNSPECIFIED.,.F.,.F.,(4,3,3,3,3,3,3,3,4),(574.911455606932,575.85242547757,
576.852187119107,577.352067939875,577.851948760644,578.85171040218,579.851472043717,
580.851233685254,581.194640914112),.UNSPECIFIED.);
#336=B_SPLINE_CURVE_WITH_KNOTS('',3,(#37818,#37819,#37820,#37821,#37822,
#37823,#37824,#37825,#37826,#37827,#37828,#37829),.UNSPECIFIED.,.F.,.F.,
(4,1,1,1,1,1,1,1,1,4),(568.628270299752,568.910539419916,569.910301061453,
570.91006270299,571.909824344526,572.909585986063,573.409466806832,573.9093476276,
574.909109269137,574.911455606932),.UNSPECIFIED.);
#337=B_SPLINE_CURVE_WITH_KNOTS('',3,(#37830,#37831,#37832,#37833,#37834,
#37835,#37836,#37837,#37838,#37839,#37840,#37841),.UNSPECIFIED.,.F.,.F.,
(4,1,1,1,1,1,1,1,1,4),(568.628270299753,568.854093986813,569.85385562835,
570.353736449118,570.853617269887,571.853378911423,572.85314055296,573.852902194497,
574.852663836033,574.911455606932),.UNSPECIFIED.);
#338=B_SPLINE_CURVE_WITH_KNOTS('',3,(#37846,#37847,#37848,#37849,#37850,
#37851,#37852,#37853,#37854,#37855,#37856,#37857,#37858,#37859,#37860,#37861,
#37862,#37863,#37864,#37865,#37866,#37867),.UNSPECIFIED.,.F.,.F.,(4,3,3,
3,3,3,3,4),(562.345084992572,563.253562066189,564.162039139807,565.070516213424,
565.978993287041,566.887470360658,567.795947434275,568.628270299752),
 .UNSPECIFIED.);
#339=B_SPLINE_CURVE_WITH_KNOTS('',3,(#37868,#37869,#37870,#37871,#37872,
#37873,#37874,#37875,#37876,#37877,#37878),.UNSPECIFIED.,.F.,.F.,(4,1,1,
1,1,1,1,1,4),(562.345084992573,562.855524137593,563.355404958361,563.85528577913,
564.855047420666,565.854809062203,566.85457070374,567.854332345276,568.628270299753),
 .UNSPECIFIED.);
#340=B_SPLINE_CURVE_WITH_KNOTS('',3,(#37883,#37884,#37885,#37886,#37887,
#37888,#37889,#37890,#37891,#37892,#37893,#37894,#37895,#37896,#37897,#37898,
#37899,#37900,#37901,#37902,#37903,#37904,#37905,#37906,#37907),
 .UNSPECIFIED.,.F.,.F.,(4,3,3,3,3,3,3,3,4),(556.061899685393,556.913399721476,
557.913161363013,558.912923004549,559.412803825317,559.912684646086,560.912446287623,
561.912207929159,562.345084992572),.UNSPECIFIED.);
#341=B_SPLINE_CURVE_WITH_KNOTS('',3,(#37908,#37909,#37910,#37911,#37912,
#37913,#37914,#37915,#37916,#37917,#37918),.UNSPECIFIED.,.F.,.F.,(4,1,1,
1,1,1,1,1,4),(556.061899685394,556.357073467604,556.856954288373,557.856715929909,
558.856477571446,559.856239212983,560.856000854519,561.855762496056,562.345084992573),
 .UNSPECIFIED.);
#342=B_SPLINE_CURVE_WITH_KNOTS('',3,(#37923,#37924,#37925,#37926,#37927,
#37928,#37929,#37930,#37931,#37932,#37933,#37934,#37935,#37936,#37937,#37938,
#37939,#37940,#37941,#37942,#37943,#37944,#37945,#37946,#37947,#37948,#37949,
#37950),.UNSPECIFIED.,.F.,.F.,(4,3,3,3,3,3,3,3,3,4),(549.778714378213,549.915068230719,
550.914829872255,551.914591513792,552.414472334561,552.914353155329,553.914114796866,
554.913876438402,555.913638079939,556.061899685393),.UNSPECIFIED.);
#343=B_SPLINE_CURVE_WITH_KNOTS('',3,(#37951,#37952,#37953,#37954,#37955,
#37956,#37957,#37958,#37959,#37960,#37961,#37962,#37963,#37964,#37965,#37966,
#37967,#37968,#37969,#37970,#37971,#37972,#37973,#37974,#37975),
 .UNSPECIFIED.,.F.,.F.,(4,3,3,3,3,3,3,3,4),(549.778714378214,549.858622797616,
550.858384439152,551.858146080689,552.857907722226,553.857669363763,554.857431005299,
555.857192646836,556.061899685394),.UNSPECIFIED.);
#344=B_SPLINE_CURVE_WITH_KNOTS('',3,(#37980,#37981,#37982,#37983,#37984,
#37985,#37986,#37987,#37988,#37989,#37990,#37991,#37992,#37993,#37994,#37995,
#37996,#37997,#37998,#37999,#38000,#38001,#38002,#38003,#38004),
 .UNSPECIFIED.,.F.,.F.,(4,3,3,3,3,3,3,3,4),(543.495529071034,543.916498381498,
544.916260023035,545.416140843804,545.916021664572,546.915783306109,547.915544947645,
548.915306589182,549.778714378213),.UNSPECIFIED.);
#345=B_SPLINE_CURVE_WITH_KNOTS('',3,(#38005,#38006,#38007,#38008,#38009,
#38010,#38011,#38012,#38013,#38014,#38015,#38016,#38017,#38018,#38019,#38020,
#38021,#38022,#38023,#38024,#38025,#38026,#38027,#38028,#38029),
 .UNSPECIFIED.,.F.,.F.,(4,3,3,3,3,3,3,3,4),(543.495529071035,543.860052948395,
544.859814589932,545.859576231469,546.859337873005,547.859099514542,548.858861156079,
549.358741976847,549.778714378214),.UNSPECIFIED.);
#346=B_SPLINE_CURVE_WITH_KNOTS('',3,(#38034,#38035,#38036,#38037,#38038,
#38039,#38040,#38041,#38042,#38043,#38044),.UNSPECIFIED.,.F.,.F.,(4,1,1,
1,1,1,1,1,4),(537.212343763854,537.917928532278,538.417809353046,538.917690173815,
539.917451815352,540.917213456888,541.916975098425,542.916736739962,543.495529071034),
 .UNSPECIFIED.);
#347=B_SPLINE_CURVE_WITH_KNOTS('',3,(#38045,#38046,#38047,#38048,#38049,
#38050,#38051,#38052,#38053,#38054,#38055,#38056,#38057,#38058,#38059,#38060,
#38061,#38062,#38063,#38064,#38065,#38066,#38067,#38068,#38069),
 .UNSPECIFIED.,.F.,.F.,(4,3,3,3,3,3,3,3,4),(537.212343763855,537.861483099175,
538.861244740712,539.861006382248,540.860768023785,541.860529665322,542.36041048609,
542.860291306859,543.495529071035),.UNSPECIFIED.);
#348=B_SPLINE_CURVE_WITH_KNOTS('',3,(#38074,#38075,#38076,#38077,#38078,
#38079,#38080,#38081,#38082,#38083,#38084),.UNSPECIFIED.,.F.,.F.,(4,1,1,
1,1,1,1,1,4),(530.929158456675,531.419477862289,531.919358683058,532.919120324594,
533.918881966131,534.918643607668,535.918405249205,536.918166890741,537.212343763854),
 .UNSPECIFIED.);
#349=B_SPLINE_CURVE_WITH_KNOTS('',3,(#38085,#38086,#38087,#38088,#38089,
#38090,#38091,#38092,#38093,#38094,#38095),.UNSPECIFIED.,.F.,.F.,(4,1,1,
1,1,1,1,1,4),(530.929158456675,531.862913249955,532.862674891491,533.862436533028,
534.862198174565,535.362078995333,535.861959816101,536.861721457638,537.212343763855),
 .UNSPECIFIED.);
#350=B_SPLINE_CURVE_WITH_KNOTS('',3,(#38100,#38101,#38102,#38103,#38104,
#38105,#38106,#38107,#38108,#38109,#38110),.UNSPECIFIED.,.F.,.F.,(4,1,1,
1,1,1,1,1,4),(524.645973149495,524.921027192301,525.920788833837,526.920550475374,
527.920312116911,528.920073758448,529.919835399984,530.919597041521,530.929158456675),
 .UNSPECIFIED.);
#351=B_SPLINE_CURVE_WITH_KNOTS('',3,(#38111,#38112,#38113,#38114,#38115,
#38116,#38117,#38118,#38119,#38120,#38121,#38122),.UNSPECIFIED.,.F.,.F.,
(4,1,1,1,1,1,1,1,1,4),(524.645973149496,524.864581759198,525.864343400734,
526.864105042271,527.863866683808,528.363747504576,528.863628325344,529.863389966881,
530.863151608418,530.929158456675),.UNSPECIFIED.);
#352=B_SPLINE_CURVE_WITH_KNOTS('',3,(#38127,#38128,#38129,#38130,#38131,
#38132,#38133,#38134,#38135,#38136,#38137,#38138,#38139,#38140,#38141,#38142,
#38143,#38144,#38145,#38146,#38147,#38148,#38149,#38150,#38151),
 .UNSPECIFIED.,.F.,.F.,(4,3,3,3,3,3,3,3,4),(518.362787842315,518.922457343081,
519.922218984617,520.921980626154,521.921742267691,522.921503909227,523.921265550764,
524.421146371532,524.645973149495),.UNSPECIFIED.);
#353=B_SPLINE_CURVE_WITH_KNOTS('',3,(#38152,#38153,#38154,#38155,#38156,
#38157,#38158,#38159,#38160,#38161,#38162),.UNSPECIFIED.,.F.,.F.,(4,1,1,
1,1,1,1,1,4),(518.362787842316,518.866011909977,519.865773551514,520.865535193051,
521.365416013819,521.865296834587,522.865058476124,523.864820117661,524.645973149496),
 .UNSPECIFIED.);
#354=B_SPLINE_CURVE_WITH_KNOTS('',3,(#38167,#38168,#38169,#38170,#38171,
#38172,#38173,#38174,#38175,#38176,#38177,#38178,#38179,#38180,#38181,#38182,
#38183,#38184,#38185,#38186,#38187,#38188,#38189,#38190,#38191),
 .UNSPECIFIED.,.F.,.F.,(4,3,3,3,3,3,3,3,4),(512.079602535136,512.92388749386,
513.923649135397,514.923410776934,515.92317241847,516.922934060007,517.422814880776,
517.922695701544,518.362787842315),.UNSPECIFIED.);
#355=B_SPLINE_CURVE_WITH_KNOTS('',3,(#38192,#38193,#38194,#38195,#38196,
#38197,#38198,#38199,#38200,#38201,#38202,#38203,#38204,#38205,#38206,#38207,
#38208,#38209,#38210,#38211,#38212,#38213,#38214,#38215,#38216),
 .UNSPECIFIED.,.F.,.F.,(4,3,3,3,3,3,3,3,4),(512.079602535137,512.867442060757,
513.867203702294,514.367084523062,514.86696534383,515.866726985367,516.866488626904,
517.866250268441,518.362787842316),.UNSPECIFIED.);
#356=B_SPLINE_CURVE_WITH_KNOTS('',3,(#38221,#38222,#38223,#38224,#38225,
#38226,#38227,#38228,#38229,#38230,#38231,#38232),.UNSPECIFIED.,.F.,.F.,
(4,1,1,1,1,1,1,1,1,4),(505.796417227956,505.925556003103,506.92531764464,
507.925079286177,508.924840927713,509.92460256925,510.424483390018,510.924364210787,
511.924125852324,512.079602535136),.UNSPECIFIED.);
#357=B_SPLINE_CURVE_WITH_KNOTS('',3,(#38233,#38234,#38235,#38236,#38237,
#38238,#38239,#38240,#38241,#38242,#38243,#38244,#38245,#38246,#38247,#38248,
#38249,#38250,#38251,#38252,#38253,#38254,#38255,#38256,#38257,#38258,#38259,
#38260),.UNSPECIFIED.,.F.,.F.,(4,3,3,3,3,3,3,3,3,4),(505.796417227957,505.86911057,
506.868872211537,507.368753032305,507.868633853074,508.86839549461,509.868157136147,
510.867918777684,511.86768041922,512.079602535137),.UNSPECIFIED.);
#358=B_SPLINE_CURVE_WITH_KNOTS('',3,(#38265,#38266,#38267,#38268,#38269,
#38270,#38271,#38272,#38273,#38274,#38275),.UNSPECIFIED.,.F.,.F.,(4,1,1,
1,1,1,1,1,4),(499.513231920777,499.926986153883,500.92674779542,501.926509436956,
502.926271078493,503.426151899261,503.92603272003,504.925794361566,505.796417227956),
 .UNSPECIFIED.);
#359=B_SPLINE_CURVE_WITH_KNOTS('',3,(#38276,#38277,#38278,#38279,#38280,
#38281,#38282,#38283,#38284,#38285,#38286),.UNSPECIFIED.,.F.,.F.,(4,1,1,
1,1,1,1,1,4),(499.513231920778,499.87054072078,500.370421541548,500.870302362316,
501.870064003853,502.86982564539,503.869587286927,504.869348928463,505.796417227957),
 .UNSPECIFIED.);
#360=B_SPLINE_CURVE_WITH_KNOTS('',3,(#38291,#38292,#38293,#38294,#38295,
#38296,#38297,#38298,#38299,#38300,#38301),.UNSPECIFIED.,.F.,.F.,(4,1,1,
1,1,1,1,1,4),(493.230046613597,493.928416304663,494.928177946199,495.927939587736,
496.427820408504,496.927701229273,497.92746287081,498.927224512346,499.513231920777),
 .UNSPECIFIED.);
#361=B_SPLINE_CURVE_WITH_KNOTS('',3,(#38302,#38303,#38304,#38305,#38306,
#38307,#38308,#38309,#38310,#38311,#38312),.UNSPECIFIED.,.F.,.F.,(4,1,1,
1,1,1,1,1,4),(493.230046613598,493.372090050791,493.871970871559,494.871732513096,
495.871494154633,496.87125579617,497.871017437706,498.870779079243,499.513231920778),
 .UNSPECIFIED.);
#362=B_SPLINE_CURVE_WITH_KNOTS('',3,(#38317,#38318,#38319,#38320,#38321,
#38322,#38323,#38324,#38325,#38326,#38327),.UNSPECIFIED.,.F.,.F.,(4,1,1,
1,1,1,1,1,4),(486.946861306418,487.929846455442,488.929608096979,489.429488917747,
489.929369738516,490.929131380052,491.928893021589,492.928654663126,493.230046613597),
 .UNSPECIFIED.);
#363=B_SPLINE_CURVE_WITH_KNOTS('',3,(#38328,#38329,#38330,#38331,#38332,
#38333,#38334,#38335,#38336,#38337),.UNSPECIFIED.,.F.,.F.,(4,1,1,1,1,1,
1,4),(486.946861306418,487.873401022339,488.873162663876,489.872924305412,
490.872685946949,491.872447588486,492.872209230023,493.230046613598),
 .UNSPECIFIED.);
#364=B_SPLINE_CURVE_WITH_KNOTS('',3,(#38342,#38343,#38344,#38345,#38346,
#38347,#38348,#38349,#38350,#38351,#38352,#38353),.UNSPECIFIED.,.F.,.F.,
(4,1,1,1,1,1,1,1,1,4),(480.663675999238,480.931514964685,481.931276606222,
482.43115742699,482.931038247759,483.930799889295,484.930561530832,485.930323172369,
486.930084813906,486.946861306418),.UNSPECIFIED.);
#365=B_SPLINE_CURVE_WITH_KNOTS('',3,(#38354,#38355,#38356,#38357,#38358,
#38359,#38360,#38361,#38362,#38363,#38364,#38365),.UNSPECIFIED.,.F.,.F.,
(4,1,1,1,1,1,1,1,1,4),(480.663675999239,480.875069531582,481.874831173119,
482.874592814655,483.874354456192,484.874116097729,485.873877739266,486.373758560034,
486.873639380802,486.946861306418),.UNSPECIFIED.);
#366=B_SPLINE_CURVE_WITH_KNOTS('',3,(#38370,#38371,#38372,#38373,#38374,
#38375,#38376,#38377,#38378,#38379,#38380),.UNSPECIFIED.,.F.,.F.,(4,1,1,
1,1,1,1,1,4),(474.380490692059,474.932945115465,475.432825936233,475.932706757002,
476.932468398538,477.932230040075,478.931991681612,479.931753323149,480.663675999238),
 .UNSPECIFIED.);
#367=B_SPLINE_CURVE_WITH_KNOTS('',3,(#38381,#38382,#38383,#38384,#38385,
#38386,#38387,#38388,#38389,#38390,#38391),.UNSPECIFIED.,.F.,.F.,(4,1,1,
1,1,1,1,1,4),(474.380490692059,474.876499682362,475.876261323898,476.876022965435,
477.875784606972,478.875546248509,479.375427069277,479.875307890045,480.663675999239),
 .UNSPECIFIED.);
#368=B_SPLINE_CURVE_WITH_KNOTS('',3,(#38396,#38397,#38398,#38399,#38400,
#38401,#38402,#38403,#38404,#38405,#38406),.UNSPECIFIED.,.F.,.F.,(4,1,1,
1,1,1,1,1,4),(468.097305384879,468.434494445476,468.934375266245,469.934136907781,
470.933898549318,471.933660190855,472.933421832392,473.933183473928,474.380490692059),
 .UNSPECIFIED.);
#369=B_SPLINE_CURVE_WITH_KNOTS('',3,(#38407,#38408,#38409,#38410,#38411,
#38412,#38413,#38414,#38415,#38416,#38417),.UNSPECIFIED.,.F.,.F.,(4,1,1,
1,1,1,1,1,4),(468.09730538488,468.877929833141,469.877691474678,470.877453116215,
471.877214757752,472.37709557852,472.876976399288,473.876738040825,474.380490692059),
 .UNSPECIFIED.);
#370=B_SPLINE_CURVE_WITH_KNOTS('',3,(#38422,#38423,#38424,#38425,#38426,
#38427,#38428,#38429,#38430,#38431,#38432),.UNSPECIFIED.,.F.,.F.,(4,1,1,
1,1,1,1,1,4),(461.814120077699,461.936043775488,462.935805417024,463.935567058561,
464.935328700098,465.935090341635,466.934851983171,467.934613624708,468.097305384879),
 .UNSPECIFIED.);
#371=B_SPLINE_CURVE_WITH_KNOTS('',3,(#38433,#38434,#38435,#38436,#38437,
#38438,#38439,#38440,#38441,#38442,#38443,#38444),.UNSPECIFIED.,.F.,.F.,
(4,1,1,1,1,1,1,1,1,4),(461.8141200777,461.879598342384,462.879359983921,
463.879121625458,464.878883266995,465.378764087763,465.878644908531,466.878406550068,
467.878168191605,468.09730538488),.UNSPECIFIED.);
#372=B_SPLINE_CURVE_WITH_KNOTS('',3,(#38449,#38450,#38451,#38452,#38453,
#38454,#38455,#38456,#38457,#38458,#38459),.UNSPECIFIED.,.F.,.F.,(4,1,1,
1,1,1,1,1,4),(455.53093477052,455.937473926267,456.937235567804,457.936997209341,
458.936758850878,459.936520492414,460.936282133951,461.436162954719,461.814120077699),
 .UNSPECIFIED.);
#373=B_SPLINE_CURVE_WITH_KNOTS('',3,(#38460,#38461,#38462,#38463,#38464,
#38465,#38466,#38467,#38468,#38469,#38470),.UNSPECIFIED.,.F.,.F.,(4,1,1,
1,1,1,1,1,4),(455.530934770521,455.881028493164,456.880790134701,457.880551776237,
458.380432597006,458.880313417774,459.880075059311,460.879836700848,461.8141200777),
 .UNSPECIFIED.);
#374=B_SPLINE_CURVE_WITH_KNOTS('',3,(#38475,#38476,#38477,#38478,#38479,
#38480,#38481,#38482,#38483,#38484,#38485),.UNSPECIFIED.,.F.,.F.,(4,1,1,
1,1,1,1,1,4),(449.24774946334,449.938904077047,450.938665718584,451.93842736012,
452.938189001657,453.937950643194,454.437831463962,454.937712284731,455.53093477052),
 .UNSPECIFIED.);
#375=B_SPLINE_CURVE_WITH_KNOTS('',3,(#38486,#38487,#38488,#38489,#38490,
#38491,#38492,#38493,#38494,#38495,#38496,#38497,#38498,#38499,#38500,#38501,
#38502,#38503,#38504,#38505,#38506,#38507),.UNSPECIFIED.,.F.,.F.,(4,3,3,
3,3,3,3,4),(449.247749463341,450.156226536958,451.064703610575,451.973180684192,
452.881657757809,453.790134831426,454.698611905043,455.530934770521),
 .UNSPECIFIED.);
#376=B_SPLINE_CURVE_WITH_KNOTS('',3,(#38512,#38513,#38514,#38515,#38516,
#38517,#38518,#38519,#38520,#38521,#38522,#38523,#38524,#38525,#38526,#38527,
#38528,#38529,#38530,#38531,#38532,#38533,#38534,#38535,#38536),
 .UNSPECIFIED.,.F.,.F.,(4,3,3,3,3,3,3,3,4),(442.964564156161,443.940334227827,
444.940095869364,445.9398575109,446.939619152437,447.439499973205,447.939380793974,
448.93914243551,449.24774946334),.UNSPECIFIED.);
#377=B_SPLINE_CURVE_WITH_KNOTS('',3,(#38537,#38538,#38539,#38540,#38541,
#38542,#38543,#38544,#38545,#38546,#38547),.UNSPECIFIED.,.F.,.F.,(4,1,1,
1,1,1,1,1,4),(442.964564156161,443.883888794723,444.383769615492,444.88365043626,
445.883412077797,446.883173719334,447.88293536087,448.882697002407,449.247749463341),
 .UNSPECIFIED.);
#378=B_SPLINE_CURVE_WITH_KNOTS('',3,(#38552,#38553,#38554,#38555,#38556,
#38557,#38558,#38559,#38560,#38561,#38562,#38563,#38564,#38565,#38566,#38567,
#38568,#38569,#38570,#38571,#38572,#38573,#38574,#38575,#38576,#38577,#38578,
#38579),.UNSPECIFIED.,.F.,.F.,(4,3,3,3,3,3,3,3,3,4),(436.681378848981,436.94200273707,
437.941764378607,438.941526020143,439.94128766168,440.441168482448,440.941049303217,
441.940810944753,442.94057258629,442.964564156161),.UNSPECIFIED.);
#379=B_SPLINE_CURVE_WITH_KNOTS('',3,(#38580,#38581,#38582,#38583,#38584,
#38585,#38586,#38587,#38588,#38589,#38590,#38591),.UNSPECIFIED.,.F.,.F.,
(4,1,1,1,1,1,1,1,1,4),(436.681378848982,436.885557303966,437.385438124735,
437.885318945503,438.88508058704,439.884842228577,440.884603870113,441.88436551165,
442.884127153187,442.964564156161),.UNSPECIFIED.);
#380=B_SPLINE_CURVE_WITH_KNOTS('',3,(#38596,#38597,#38598,#38599,#38600,
#38601,#38602,#38603,#38604,#38605,#38606),.UNSPECIFIED.,.F.,.F.,(4,1,1,
1,1,1,1,1,4),(430.398193541802,430.943432887849,431.943194529386,432.942956170923,
433.442836991691,433.94271781246,434.942479453996,435.942241095533,436.681378848981),
 .UNSPECIFIED.);
#381=B_SPLINE_CURVE_WITH_KNOTS('',3,(#38607,#38608,#38609,#38610,#38611,
#38612,#38613,#38614,#38615,#38616),.UNSPECIFIED.,.F.,.F.,(4,1,1,1,1,1,
1,4),(430.398193541802,430.886987454746,431.886749096283,432.88651073782,
433.886272379356,434.886034020893,435.88579566243,436.681378848982),
 .UNSPECIFIED.);
#382=B_SPLINE_CURVE_WITH_KNOTS('',3,(#38621,#38622,#38623,#38624,#38625,
#38626,#38627,#38628,#38629,#38630,#38631),.UNSPECIFIED.,.F.,.F.,(4,1,1,
1,1,1,1,1,4),(424.115008234622,424.944863038629,425.944624680166,426.444505500934,
426.944386321703,427.944147963239,428.943909604776,429.943671246313,430.398193541802),
 .UNSPECIFIED.);
#383=B_SPLINE_CURVE_WITH_KNOTS('',3,(#38632,#38633,#38634,#38635,#38636,
#38637,#38638,#38639,#38640,#38641,#38642),.UNSPECIFIED.,.F.,.F.,(4,1,1,
1,1,1,1,1,4),(424.115008234623,424.888417605526,425.888179247063,426.887940888599,
427.887702530136,428.887464171673,429.887225813209,430.387106633978,430.398193541802),
 .UNSPECIFIED.);
#384=B_SPLINE_CURVE_WITH_KNOTS('',3,(#38647,#38648,#38649,#38650,#38651,
#38652,#38653,#38654,#38655,#38656,#38657,#38658),.UNSPECIFIED.,.F.,.F.,
(4,1,1,1,1,1,1,1,1,4),(417.831822927443,417.946531547872,418.946293189409,
419.446174010177,419.946054830946,420.945816472482,421.945578114019,422.945339755556,
423.945101397092,424.115008234622),.UNSPECIFIED.);
#385=B_SPLINE_CURVE_WITH_KNOTS('',3,(#38659,#38660,#38661,#38662,#38663,
#38664,#38665,#38666,#38667,#38668,#38669,#38670),.UNSPECIFIED.,.F.,.F.,
(4,1,1,1,1,1,1,1,1,4),(417.831822927443,417.890086114769,418.889847756306,
419.889609397842,420.889371039379,421.889132680916,422.888894322452,423.388775143221,
423.888655963989,424.115008234623),.UNSPECIFIED.);
#386=B_SPLINE_CURVE_WITH_KNOTS('',3,(#38675,#38676,#38677,#38678,#38679,
#38680,#38681,#38682,#38683,#38684,#38685),.UNSPECIFIED.,.F.,.F.,(4,1,1,
1,1,1,1,1,4),(411.548637620263,411.947961698652,412.44784251942,412.947723340189,
413.947484981725,414.947246623262,415.947008264799,416.946769906335,417.831822927443),
 .UNSPECIFIED.);
#387=B_SPLINE_CURVE_WITH_KNOTS('',3,(#38686,#38687,#38688,#38689,#38690,
#38691,#38692,#38693,#38694,#38695,#38696),.UNSPECIFIED.,.F.,.F.,(4,1,1,
1,1,1,1,1,4),(411.548637620264,411.891516265548,412.891277907085,413.891039548622,
414.890801190159,415.890562831695,416.390443652464,416.890324473232,417.831822927443),
 .UNSPECIFIED.);
#388=B_SPLINE_CURVE_WITH_KNOTS('',3,(#38701,#38702,#38703,#38704,#38705,
#38706,#38707,#38708,#38709,#38710,#38711),.UNSPECIFIED.,.F.,.F.,(4,1,1,
1,1,1,1,1,4),(405.265452313083,405.449511028663,405.949391849432,406.949153490968,
407.948915132505,408.948676774042,409.948438415578,410.948200057115,411.548637620263),
 .UNSPECIFIED.);
#389=B_SPLINE_CURVE_WITH_KNOTS('',3,(#38712,#38713,#38714,#38715,#38716,
#38717,#38718,#38719,#38720,#38721,#38722,#38723,#38724,#38725,#38726,#38727,
#38728,#38729,#38730,#38731,#38732,#38733),.UNSPECIFIED.,.F.,.F.,(4,3,3,
3,3,3,3,4),(405.265452313084,406.173929386701,407.082406460318,407.990883533935,
408.899360607552,409.807837681169,410.716314754786,411.548637620264),
 .UNSPECIFIED.);
#390=B_SPLINE_CURVE_WITH_KNOTS('',3,(#38738,#38739,#38740,#38741,#38742,
#38743,#38744,#38745,#38746,#38747),.UNSPECIFIED.,.F.,.F.,(4,1,1,1,1,1,
1,4),(398.982267005904,399.950822000211,400.950583641748,401.950345283285,
402.950106924821,403.949868566358,404.949630207895,405.265452313083),
 .UNSPECIFIED.);
#391=B_SPLINE_CURVE_WITH_KNOTS('',3,(#38748,#38749,#38750,#38751,#38752,
#38753,#38754,#38755,#38756,#38757,#38758),.UNSPECIFIED.,.F.,.F.,(4,1,1,
1,1,1,1,1,4),(398.982267005905,399.894376567108,400.894138208645,401.893899850181,
402.39378067095,402.893661491718,403.893423133255,404.893184774791,405.265452313084),
 .UNSPECIFIED.);
#392=B_SPLINE_CURVE_WITH_KNOTS('',3,(#38763,#38764,#38765,#38766,#38767,
#38768,#38769,#38770,#38771,#38772,#38773,#38774),.UNSPECIFIED.,.F.,.F.,
(4,1,1,1,1,1,1,1,1,4),(392.699081698724,392.952490509454,393.952252150991,
394.952013792528,395.951775434064,396.951537075601,397.951298717138,398.451179537906,
398.951060358675,398.982267005904),.UNSPECIFIED.);
#393=B_SPLINE_CURVE_WITH_KNOTS('',3,(#38775,#38776,#38777,#38778,#38779,
#38780,#38781,#38782,#38783,#38784,#38785,#38786),.UNSPECIFIED.,.F.,.F.,
(4,1,1,1,1,1,1,1,1,4),(392.699081698725,392.896045076351,393.895806717888,
394.895568359424,395.395449180193,395.895330000961,396.895091642498,397.894853284034,
398.894614925571,398.982267005905),.UNSPECIFIED.);
#394=B_SPLINE_CURVE_WITH_KNOTS('',3,(#38791,#38792,#38793,#38794,#38795,
#38796,#38797,#38798,#38799,#38800,#38801),.UNSPECIFIED.,.F.,.F.,(4,1,1,
1,1,1,1,1,4),(386.415896391545,386.953920660234,387.953682301771,388.953443943307,
389.953205584844,390.952967226381,391.452848047149,391.952728867918,392.699081698724),
 .UNSPECIFIED.);
#395=B_SPLINE_CURVE_WITH_KNOTS('',3,(#38802,#38803,#38804,#38805,#38806,
#38807,#38808,#38809,#38810,#38811,#38812),.UNSPECIFIED.,.F.,.F.,(4,1,1,
1,1,1,1,1,4),(386.415896391545,386.897475227131,387.897236868667,388.397117689436,
388.896998510204,389.896760151741,390.896521793277,391.896283434814,392.699081698725),
 .UNSPECIFIED.);
#396=B_SPLINE_CURVE_WITH_KNOTS('',3,(#38817,#38818,#38819,#38820,#38821,
#38822,#38823,#38824,#38825,#38826,#38827),.UNSPECIFIED.,.F.,.F.,(4,1,1,
1,1,1,1,1,4),(380.132711084365,380.955350811014,381.95511245255,382.954874094087,
383.954635735624,384.454516556392,384.95439737716,385.954159018697,386.415896391545),
 .UNSPECIFIED.);
#397=B_SPLINE_CURVE_WITH_KNOTS('',3,(#38828,#38829,#38830,#38831,#38832,
#38833,#38834,#38835,#38836,#38837,#38838),.UNSPECIFIED.,.F.,.F.,(4,1,1,
1,1,1,1,1,4),(380.132711084366,380.89890537791,381.398786198679,381.898667019447,
382.898428660984,383.89819030252,384.897951944057,385.897713585594,386.415896391545),
 .UNSPECIFIED.);
#398=B_SPLINE_CURVE_WITH_KNOTS('',3,(#38843,#38844,#38845,#38846,#38847,
#38848,#38849,#38850,#38851,#38852,#38853,#38854),.UNSPECIFIED.,.F.,.F.,
(4,1,1,1,1,1,1,1,1,4),(373.849525777185,373.957019320257,374.956780961793,
375.95654260333,376.956304244867,377.456185065635,377.956065886403,378.95582752794,
379.955589169477,380.132711084365),.UNSPECIFIED.);
#399=B_SPLINE_CURVE_WITH_KNOTS('',3,(#38855,#38856,#38857,#38858,#38859,
#38860,#38861,#38862,#38863,#38864,#38865,#38866),.UNSPECIFIED.,.F.,.F.,
(4,1,1,1,1,1,1,1,1,4),(373.849525777186,373.900573887153,374.400454707922,
374.90033552869,375.900097170227,376.899858811763,377.8996204533,378.899382094837,
379.899143736374,380.132711084366),.UNSPECIFIED.);
#400=B_SPLINE_CURVE_WITH_KNOTS('',3,(#38871,#38872,#38873,#38874,#38875,
#38876,#38877,#38878,#38879,#38880,#38881),.UNSPECIFIED.,.F.,.F.,(4,1,1,
1,1,1,1,1,4),(367.566340470006,367.958449471036,368.958211112573,369.95797275411,
370.457853574878,370.957734395646,371.957496037183,372.95725767872,373.849525777185),
 .UNSPECIFIED.);
#401=B_SPLINE_CURVE_WITH_KNOTS('',3,(#38882,#38883,#38884,#38885,#38886,
#38887,#38888,#38889,#38890,#38891),.UNSPECIFIED.,.F.,.F.,(4,1,1,1,1,1,
1,4),(367.566340470007,367.902004037933,368.90176567947,369.901527321006,
370.901288962543,371.90105060408,372.900812245617,373.849525777186),
 .UNSPECIFIED.);
#402=B_SPLINE_CURVE_WITH_KNOTS('',3,(#38896,#38897,#38898,#38899,#38900,
#38901,#38902,#38903,#38904,#38905,#38906,#38907,#38908,#38909,#38910,#38911,
#38912,#38913,#38914,#38915,#38916,#38917),.UNSPECIFIED.,.F.,.F.,(4,3,3,
3,3,3,3,4),(361.283155162826,362.191632236443,363.10010931006,364.008586383677,
364.917063457294,365.825540530911,366.734017604529,367.566340470006),
 .UNSPECIFIED.);
#403=B_SPLINE_CURVE_WITH_KNOTS('',3,(#38918,#38919,#38920,#38921,#38922,
#38923,#38924,#38925,#38926,#38927,#38928),.UNSPECIFIED.,.F.,.F.,(4,1,1,
1,1,1,1,1,4),(361.283155162827,361.903434188713,362.903195830249,363.902957471786,
364.902719113323,365.902480754859,366.902242396396,367.402123217165,367.566340470007),
 .UNSPECIFIED.);
#404=B_SPLINE_CURVE_WITH_KNOTS('',3,(#38933,#38934,#38935,#38936,#38937,
#38938,#38939,#38940,#38941,#38942,#38943),.UNSPECIFIED.,.F.,.F.,(4,1,1,
1,1,1,1,1,4),(354.999969855647,355.961309772596,356.461190593364,356.961071414132,
357.960833055669,358.960594697206,359.960356338743,360.960117980279,361.283155162826),
 .UNSPECIFIED.);
#405=B_SPLINE_CURVE_WITH_KNOTS('',3,(#38944,#38945,#38946,#38947,#38948,
#38949,#38950,#38951,#38952,#38953,#38954),.UNSPECIFIED.,.F.,.F.,(4,1,1,
1,1,1,1,1,4),(354.999969855648,355.904864339492,356.904625981029,357.904387622566,
358.904149264102,359.903910905639,360.403791726408,360.903672547176,361.283155162827),
 .UNSPECIFIED.);
#406=B_SPLINE_CURVE_WITH_KNOTS('',3,(#38959,#38960,#38961,#38962,#38963,
#38964,#38965,#38966,#38967,#38968,#38969,#38970),.UNSPECIFIED.,.F.,.F.,
(4,1,1,1,1,1,1,1,1,4),(348.716784548467,348.962978281839,349.462859102607,
349.962739923375,350.962501564912,351.962263206449,352.962024847986,353.961786489522,
354.961548131059,354.999969855647),.UNSPECIFIED.);
#407=B_SPLINE_CURVE_WITH_KNOTS('',3,(#38971,#38972,#38973,#38974,#38975,
#38976,#38977,#38978,#38979,#38980,#38981,#38982),.UNSPECIFIED.,.F.,.F.,
(4,1,1,1,1,1,1,1,1,4),(348.716784548468,348.906532848735,349.906294490272,
350.906056131809,351.905817773345,352.905579414882,353.40546023565,353.905341056419,
354.905102697956,354.999969855648),.UNSPECIFIED.);
#408=B_SPLINE_CURVE_WITH_KNOTS('',3,(#38987,#38988,#38989,#38990,#38991,
#38992,#38993,#38994,#38995,#38996,#38997),.UNSPECIFIED.,.F.,.F.,(4,1,1,
1,1,1,1,1,4),(342.433599241288,342.46452761185,342.964408432618,343.964170074155,
344.963931715692,345.963693357229,346.963454998765,347.963216640302,348.716784548467),
 .UNSPECIFIED.);
#409=B_SPLINE_CURVE_WITH_KNOTS('',3,(#38998,#38999,#39000,#39001,#39002,
#39003,#39004,#39005,#39006,#39007,#39008),.UNSPECIFIED.,.F.,.F.,(4,1,1,
1,1,1,1,1,4),(342.433599241289,342.907962999515,343.907724641052,344.907486282588,
345.907247924125,346.407128744893,346.907009565662,347.906771207199,348.716784548468),
 .UNSPECIFIED.);
#410=B_SPLINE_CURVE_WITH_KNOTS('',3,(#39013,#39014,#39015,#39016,#39017,
#39018,#39019,#39020,#39021,#39022),.UNSPECIFIED.,.F.,.F.,(4,1,1,1,1,1,
1,4),(336.150413934108,336.965838583398,337.965600224935,338.965361866472,
339.965123508008,340.964885149545,341.964646791082,342.433599241288),
 .UNSPECIFIED.);
#411=B_SPLINE_CURVE_WITH_KNOTS('',3,(#39023,#39024,#39025,#39026,#39027,
#39028,#39029,#39030,#39031,#39032,#39033),.UNSPECIFIED.,.F.,.F.,(4,1,1,
1,1,1,1,1,4),(336.150413934109,336.909393150295,337.909154791831,338.908916433368,
339.408797254136,339.908678074905,340.908439716442,341.908201357978,342.433599241289),
 .UNSPECIFIED.);
#412=B_SPLINE_CURVE_WITH_KNOTS('',3,(#39038,#39039,#39040,#39041,#39042,
#39043,#39044,#39045,#39046,#39047,#39048,#39049),.UNSPECIFIED.,.F.,.F.,
(4,1,1,1,1,1,1,1,1,4),(329.867228626929,329.967507092641,330.967268734178,
331.967030375715,332.966792017251,333.966553658788,334.966315300325,335.466196121093,
335.966076941861,336.150413934108),.UNSPECIFIED.);
#413=B_SPLINE_CURVE_WITH_KNOTS('',3,(#39050,#39051,#39052,#39053,#39054,
#39055,#39056,#39057,#39058,#39059,#39060,#39061),.UNSPECIFIED.,.F.,.F.,
(4,1,1,1,1,1,1,1,1,4),(329.867228626929,329.911061659538,330.910823301074,
331.910584942611,332.410465763379,332.910346584148,333.910108225684,334.909869867221,
335.909631508758,336.150413934109),.UNSPECIFIED.);
#414=B_SPLINE_CURVE_WITH_KNOTS('',3,(#39066,#39067,#39068,#39069,#39070,
#39071,#39072,#39073,#39074,#39075,#39076),.UNSPECIFIED.,.F.,.F.,(4,1,1,
1,1,1,1,1,4),(323.584043319749,323.968937243421,324.968698884957,325.968460526494,
326.468341347263,326.968222168031,327.967983809568,328.967745451104,329.867228626929),
 .UNSPECIFIED.);
#415=B_SPLINE_CURVE_WITH_KNOTS('',3,(#39077,#39078,#39079,#39080,#39081,
#39082,#39083,#39084,#39085,#39086),.UNSPECIFIED.,.F.,.F.,(4,1,1,1,1,1,
1,4),(323.58404331975,323.912491810317,324.912253451854,325.912015093391,
326.911776734928,327.911538376464,328.911300018001,329.867228626929),
 .UNSPECIFIED.);
#416=B_SPLINE_CURVE_WITH_KNOTS('',3,(#39091,#39092,#39093,#39094,#39095,
#39096,#39097,#39098,#39099,#39100,#39101,#39102,#39103,#39104,#39105,#39106,
#39107,#39108,#39109,#39110,#39111,#39112),.UNSPECIFIED.,.F.,.F.,(4,3,3,
3,3,3,3,4),(317.300858012569,318.209335086186,319.117812159803,320.02628923342,
320.934766307037,321.843243380654,322.751720454271,323.584043319749),
 .UNSPECIFIED.);
#417=B_SPLINE_CURVE_WITH_KNOTS('',3,(#39113,#39114,#39115,#39116,#39117,
#39118,#39119,#39120,#39121,#39122,#39123),.UNSPECIFIED.,.F.,.F.,(4,1,1,
1,1,1,1,1,4),(317.30085801257,317.913921961097,318.913683602634,319.91344524417,
320.913206885707,321.912968527244,322.912730168781,323.412610989549,323.58404331975),
 .UNSPECIFIED.);
#418=B_SPLINE_CURVE_WITH_KNOTS('',3,(#39128,#39129,#39130,#39131,#39132,
#39133,#39134,#39135,#39136,#39137,#39138),.UNSPECIFIED.,.F.,.F.,(4,1,1,
1,1,1,1,1,4),(311.01767270539,311.97179754498,312.471678365749,312.971559186517,
313.971320828054,314.97108246959,315.970844111127,316.970605752664,317.300858012569),
 .UNSPECIFIED.);
#419=B_SPLINE_CURVE_WITH_KNOTS('',3,(#39139,#39140,#39141,#39142,#39143,
#39144,#39145,#39146,#39147,#39148,#39149),.UNSPECIFIED.,.F.,.F.,(4,1,1,
1,1,1,1,1,4),(311.017672705391,311.915352111877,312.915113753413,313.91487539495,
314.914637036487,315.914398678024,316.414279498792,316.91416031956,317.30085801257),
 .UNSPECIFIED.);
#420=B_SPLINE_CURVE_WITH_KNOTS('',3,(#39154,#39155,#39156,#39157,#39158,
#39159,#39160,#39161,#39162,#39163,#39164,#39165),.UNSPECIFIED.,.F.,.F.,
(4,1,1,1,1,1,1,1,1,4),(304.73448739821,304.973466054223,305.473346874992,
305.97322769576,306.972989337297,307.972750978833,308.97251262037,309.972274261907,
310.972035903443,311.01767270539),.UNSPECIFIED.);
#421=B_SPLINE_CURVE_WITH_KNOTS('',3,(#39166,#39167,#39168,#39169,#39170,
#39171,#39172,#39173,#39174,#39175,#39176,#39177),.UNSPECIFIED.,.F.,.F.,
(4,1,1,1,1,1,1,1,1,4),(304.734487398211,304.91702062112,305.916782262656,
306.916543904193,307.91630554573,308.916067187267,309.415948008035,309.915828828803,
310.91559047034,311.017672705391),.UNSPECIFIED.);
#422=B_SPLINE_CURVE_WITH_KNOTS('',3,(#39182,#39183,#39184,#39185,#39186,
#39187,#39188,#39189,#39190,#39191,#39192),.UNSPECIFIED.,.F.,.F.,(4,1,1,
1,1,1,1,1,4),(298.451302091031,298.475015384234,298.974896205003,299.97465784654,
300.974419488076,301.974181129613,302.97394277115,303.973704412686,304.73448739821),
 .UNSPECIFIED.);
#423=B_SPLINE_CURVE_WITH_KNOTS('',3,(#39193,#39194,#39195,#39196,#39197,
#39198,#39199,#39200,#39201,#39202,#39203),.UNSPECIFIED.,.F.,.F.,(4,1,1,
1,1,1,1,1,4),(298.451302091031,298.918450771899,299.918212413436,300.917974054973,
301.91773569651,302.417616517278,302.917497338046,303.917258979583,304.734487398211),
 .UNSPECIFIED.);
#424=B_SPLINE_CURVE_WITH_KNOTS('',3,(#39208,#39209,#39210,#39211,#39212,
#39213,#39214,#39215,#39216,#39217),.UNSPECIFIED.,.F.,.F.,(4,1,1,1,1,1,
1,4),(292.168116783851,292.976326355783,293.976087997319,294.975849638856,
295.975611280393,296.975372921929,297.975134563466,298.451302091031),
 .UNSPECIFIED.);
#425=B_SPLINE_CURVE_WITH_KNOTS('',3,(#39218,#39219,#39220,#39221,#39222,
#39223,#39224,#39225,#39226,#39227,#39228),.UNSPECIFIED.,.F.,.F.,(4,1,1,
1,1,1,1,1,4),(292.168116783852,292.919880922679,293.919642564216,294.919404205753,
295.419285026521,295.919165847289,296.918927488826,297.918689130363,298.451302091031),
 .UNSPECIFIED.);
#426=B_SPLINE_CURVE_WITH_KNOTS('',3,(#39233,#39234,#39235,#39236,#39237,
#39238,#39239,#39240,#39241,#39242,#39243,#39244),.UNSPECIFIED.,.F.,.F.,
(4,1,1,1,1,1,1,1,1,4),(285.884931476672,285.977994865025,286.977756506562,
287.977518148099,288.977279789636,289.977041431172,290.976803072709,291.476683893477,
291.976564714246,292.168116783851),.UNSPECIFIED.);
#427=B_SPLINE_CURVE_WITH_KNOTS('',3,(#39245,#39246,#39247,#39248,#39249,
#39250,#39251,#39252,#39253,#39254,#39255,#39256),.UNSPECIFIED.,.F.,.F.,
(4,1,1,1,1,1,1,1,1,4),(285.884931476672,285.921549431922,286.921311073459,
287.921072714995,288.420953535764,288.920834356532,289.920595998069,290.920357639606,
291.920119281142,292.168116783852),.UNSPECIFIED.);
#428=B_SPLINE_CURVE_WITH_KNOTS('',3,(#39261,#39262,#39263,#39264,#39265,
#39266,#39267,#39268,#39269,#39270,#39271),.UNSPECIFIED.,.F.,.F.,(4,1,1,
1,1,1,1,1,4),(279.601746169492,279.979425015805,280.979186657342,281.978948298879,
282.978709940415,283.978471581952,284.47835240272,284.978233223489,285.884931476672),
 .UNSPECIFIED.);
#429=B_SPLINE_CURVE_WITH_KNOTS('',3,(#39272,#39273,#39274,#39275,#39276,
#39277,#39278,#39279,#39280,#39281,#39282),.UNSPECIFIED.,.F.,.F.,(4,1,1,
1,1,1,1,1,4),(279.601746169493,279.922979582702,280.922741224238,281.422622045007,
281.922502865775,282.922264507312,283.922026148849,284.921787790385,285.884931476672),
 .UNSPECIFIED.);
#430=B_SPLINE_CURVE_WITH_KNOTS('',3,(#39287,#39288,#39289,#39290,#39291,
#39292,#39293,#39294,#39295,#39296,#39297,#39298,#39299,#39300,#39301,#39302,
#39303,#39304,#39305,#39306,#39307,#39308),.UNSPECIFIED.,.F.,.F.,(4,3,3,
3,3,3,3,4),(273.318560862313,274.227037935929,275.135515009546,276.043992083163,
276.95246915678,277.860946230397,278.769423304014,279.601746169492),
 .UNSPECIFIED.);
#431=B_SPLINE_CURVE_WITH_KNOTS('',3,(#39309,#39310,#39311,#39312,#39313,
#39314,#39315,#39316,#39317,#39318,#39319),.UNSPECIFIED.,.F.,.F.,(4,1,1,
1,1,1,1,1,4),(273.318560862313,273.924409733481,274.42429055425,274.924171375018,
275.923933016555,276.923694658092,277.923456299628,278.923217941165,279.601746169493),
 .UNSPECIFIED.);
#432=B_SPLINE_CURVE_WITH_KNOTS('',3,(#39324,#39325,#39326,#39327,#39328,
#39329,#39330,#39331,#39332,#39333,#39334),.UNSPECIFIED.,.F.,.F.,(4,1,1,
1,1,1,1,1,4),(267.035375555133,267.982285317365,268.982046958901,269.981808600438,
270.481689421206,270.981570241975,271.981331883511,272.981093525048,273.318560862312),
 .UNSPECIFIED.);
#433=B_SPLINE_CURVE_WITH_KNOTS('',3,(#39335,#39336,#39337,#39338,#39339,
#39340,#39341,#39342,#39343,#39344,#39345),.UNSPECIFIED.,.F.,.F.,(4,1,1,
1,1,1,1,1,4),(267.035375555134,267.425959063493,267.925839884261,268.925601525798,
269.925363167335,270.925124808871,271.924886450408,272.924648091945,273.318560862313),
 .UNSPECIFIED.);
#434=B_SPLINE_CURVE_WITH_KNOTS('',3,(#39350,#39351,#39352,#39353,#39354,
#39355,#39356,#39357,#39358,#39359,#39360,#39361),.UNSPECIFIED.,.F.,.F.,
(4,1,1,1,1,1,1,1,1,4),(260.752190247953,260.983953826608,261.983715468144,
262.983477109681,263.483357930449,263.983238751218,264.983000392754,265.982762034291,
266.982523675828,267.035375555133),.UNSPECIFIED.);
#435=B_SPLINE_CURVE_WITH_KNOTS('',3,(#39362,#39363,#39364,#39365,#39366,
#39367,#39368,#39369,#39370,#39371,#39372),.UNSPECIFIED.,.F.,.F.,(4,1,1,
1,1,1,1,1,4),(260.752190247954,260.927508393504,261.927270035041,262.927031676578,
263.926793318114,264.926554959651,265.926316601188,266.926078242724,267.035375555134),
 .UNSPECIFIED.);
#436=B_SPLINE_CURVE_WITH_KNOTS('',3,(#39377,#39378,#39379,#39380,#39381,
#39382,#39383,#39384,#39385,#39386,#39387),.UNSPECIFIED.,.F.,.F.,(4,1,1,
1,1,1,1,1,4),(254.469004940774,254.985383977387,255.985145618924,256.485026439692,
256.984907260461,257.984668901997,258.984430543534,259.984192185071,260.752190247953),
 .UNSPECIFIED.);
#437=B_SPLINE_CURVE_WITH_KNOTS('',3,(#39388,#39389,#39390,#39391,#39392,
#39393,#39394,#39395,#39396,#39397,#39398),.UNSPECIFIED.,.F.,.F.,(4,1,1,
1,1,1,1,1,4),(254.469004940774,254.928938544284,255.928700185821,256.928461827357,
257.928223468894,258.927985110431,259.927746751967,260.427627572736,260.752190247954),
 .UNSPECIFIED.);
#438=B_SPLINE_CURVE_WITH_KNOTS('',3,(#39403,#39404,#39405,#39406,#39407,
#39408,#39409,#39410,#39411,#39412,#39413),.UNSPECIFIED.,.F.,.F.,(4,1,1,
1,1,1,1,1,4),(248.185819633594,248.986814128167,249.486694948935,249.986575769704,
250.98633741124,251.986099052777,252.985860694314,253.985622335851,254.469004940774),
 .UNSPECIFIED.);
#439=B_SPLINE_CURVE_WITH_KNOTS('',3,(#39414,#39415,#39416,#39417,#39418,
#39419,#39420,#39421,#39422,#39423,#39424),.UNSPECIFIED.,.F.,.F.,(4,1,1,
1,1,1,1,1,4),(248.185819633595,248.930368695063,249.9301303366,250.929891978137,
251.929653619674,252.92941526121,253.429296081979,253.929176902747,254.469004940774),
 .UNSPECIFIED.);
#440=B_SPLINE_CURVE_WITH_KNOTS('',3,(#39429,#39430,#39431,#39432,#39433,
#39434,#39435,#39436,#39437,#39438,#39439,#39440),.UNSPECIFIED.,.F.,.F.,
(4,1,1,1,1,1,1,1,1,4),(241.902634326415,241.98848263741,242.488363458178,
242.988244278947,243.988005920483,244.98776756202,245.987529203557,246.987290845094,
247.98705248663,248.185819633594),.UNSPECIFIED.);
#441=B_SPLINE_CURVE_WITH_KNOTS('',3,(#39441,#39442,#39443,#39444,#39445,
#39446,#39447,#39448,#39449,#39450,#39451,#39452),.UNSPECIFIED.,.F.,.F.,
(4,1,1,1,1,1,1,1,1,4),(241.902634326415,241.932037204306,242.931798845843,
243.93156048738,244.931322128917,245.931083770453,246.430964591222,246.93084541199,
247.930607053527,248.185819633595),.UNSPECIFIED.);
#442=B_SPLINE_CURVE_WITH_KNOTS('',3,(#39457,#39458,#39459,#39460,#39461,
#39462,#39463,#39464,#39465,#39466),.UNSPECIFIED.,.F.,.F.,(4,1,1,1,1,1,
1,4),(235.619449019235,235.98991278819,236.989674429726,237.989436071263,
238.9891977128,239.988959354337,240.988720995873,241.902634326415),
 .UNSPECIFIED.);
#443=B_SPLINE_CURVE_WITH_KNOTS('',3,(#39467,#39468,#39469,#39470,#39471,
#39472,#39473,#39474,#39475,#39476,#39477),.UNSPECIFIED.,.F.,.F.,(4,1,1,
1,1,1,1,1,4),(235.619449019236,235.933467355086,236.933228996623,237.93299063816,
238.932752279696,239.432633100465,239.932513921233,240.93227556277,241.902634326415),
 .UNSPECIFIED.);
#444=B_SPLINE_CURVE_WITH_KNOTS('',3,(#39482,#39483,#39484,#39485,#39486,
#39487,#39488,#39489,#39490,#39491,#39492),.UNSPECIFIED.,.F.,.F.,(4,1,1,
1,1,1,1,1,4),(229.336263712056,229.991342938969,230.991104580506,231.990866222043,
232.99062786358,233.990389505116,234.990151146653,235.490031967421,235.619449019235),
 .UNSPECIFIED.);
#445=B_SPLINE_CURVE_WITH_KNOTS('',3,(#39493,#39494,#39495,#39496,#39497,
#39498,#39499,#39500,#39501,#39502,#39503),.UNSPECIFIED.,.F.,.F.,(4,1,1,
1,1,1,1,1,4),(229.336263712056,229.934897505866,230.934659147403,231.934420788939,
232.434301609708,232.934182430476,233.933944072013,234.933705713549,235.619449019236),
 .UNSPECIFIED.);
#446=B_SPLINE_CURVE_WITH_KNOTS('',3,(#39508,#39509,#39510,#39511,#39512,
#39513,#39514,#39515,#39516,#39517,#39518),.UNSPECIFIED.,.F.,.F.,(4,1,1,
1,1,1,1,1,4),(223.053078404876,223.992773089749,224.992534731286,225.992296372822,
226.992058014359,227.991819655896,228.491700476664,228.991581297433,229.336263712056),
 .UNSPECIFIED.);
#447=B_SPLINE_CURVE_WITH_KNOTS('',3,(#39519,#39520,#39521,#39522,#39523,
#39524,#39525,#39526,#39527,#39528,#39529),.UNSPECIFIED.,.F.,.F.,(4,1,1,
1,1,1,1,1,4),(223.053078404877,223.936327656646,224.936089298182,225.435970118951,
225.935850939719,226.935612581256,227.935374222792,228.935135864329,229.336263712056),
 .UNSPECIFIED.);
#448=B_SPLINE_CURVE_WITH_KNOTS('',3,(#39534,#39535,#39536,#39537,#39538,
#39539,#39540,#39541,#39542,#39543,#39544,#39545),.UNSPECIFIED.,.F.,.F.,
(4,1,1,1,1,1,1,1,1,4),(216.769893097696,216.994441598992,217.994203240529,
218.993964882065,219.993726523602,220.993488165139,221.493368985907,221.993249806676,
222.993011448212,223.053078404876),.UNSPECIFIED.);
#449=B_SPLINE_CURVE_WITH_KNOTS('',3,(#39546,#39547,#39548,#39549,#39550,
#39551,#39552,#39553,#39554,#39555,#39556,#39557),.UNSPECIFIED.,.F.,.F.,
(4,1,1,1,1,1,1,1,1,4),(216.769893097697,216.937996165889,217.937757807425,
218.437638628194,218.937519448962,219.937281090499,220.937042732035,221.936804373572,
222.936566015109,223.053078404877),.UNSPECIFIED.);
#450=B_SPLINE_CURVE_WITH_KNOTS('',3,(#39562,#39563,#39564,#39565,#39566,
#39567,#39568,#39569,#39570,#39571,#39572),.UNSPECIFIED.,.F.,.F.,(4,1,1,
1,1,1,1,1,4),(210.486707790517,210.995871749772,211.995633391308,212.995395032845,
213.995156674382,214.49503749515,214.994918315919,215.994679957455,216.769893097696),
 .UNSPECIFIED.);
#451=B_SPLINE_CURVE_WITH_KNOTS('',3,(#39573,#39574,#39575,#39576,#39577,
#39578,#39579,#39580,#39581,#39582,#39583),.UNSPECIFIED.,.F.,.F.,(4,1,1,
1,1,1,1,1,4),(210.486707790518,210.939426316668,211.439307137437,211.939187958205,
212.938949599742,213.938711241278,214.938472882815,215.938234524352,216.769893097697),
 .UNSPECIFIED.);
#452=B_SPLINE_CURVE_WITH_KNOTS('',3,(#39588,#39589,#39590,#39591,#39592,
#39593,#39594,#39595,#39596,#39597,#39598),.UNSPECIFIED.,.F.,.F.,(4,1,1,
1,1,1,1,1,4),(204.203522483337,204.997301900551,205.997063542088,206.996825183625,
207.496706004393,207.996586825162,208.996348466698,209.996110108235,210.486707790517),
 .UNSPECIFIED.);
#453=B_SPLINE_CURVE_WITH_KNOTS('',3,(#39599,#39600,#39601,#39602,#39603,
#39604,#39605,#39606,#39607,#39608,#39609),.UNSPECIFIED.,.F.,.F.,(4,1,1,
1,1,1,1,1,4),(204.203522483338,204.44097564668,204.940856467448,205.940618108985,
206.940379750521,207.940141392058,208.939903033595,209.939664675131,210.486707790518),
 .UNSPECIFIED.);
#454=B_SPLINE_CURVE_WITH_KNOTS('',3,(#39614,#39615,#39616,#39617,#39618,
#39619,#39620,#39621,#39622,#39623,#39624,#39625),.UNSPECIFIED.,.F.,.F.,
(4,1,1,1,1,1,1,1,1,4),(197.920337176158,197.998970409794,198.998732051331,
199.998493692868,200.498374513636,200.998255334405,201.998016975941,202.997778617478,
203.997540259015,204.203522483337),.UNSPECIFIED.);
#455=B_SPLINE_CURVE_WITH_KNOTS('',3,(#39626,#39627,#39628,#39629,#39630,
#39631,#39632,#39633,#39634,#39635,#39636),.UNSPECIFIED.,.F.,.F.,(4,1,1,
1,1,1,1,1,4),(197.920337176158,197.942524976691,198.942286618228,199.942048259764,
200.941809901301,201.941571542838,202.941333184374,203.941094825911,204.203522483338),
 .UNSPECIFIED.);
#456=B_SPLINE_CURVE_WITH_KNOTS('',3,(#39641,#39642,#39643,#39644,#39645,
#39646,#39647,#39648,#39649,#39650,#39651),.UNSPECIFIED.,.F.,.F.,(4,1,1,
1,1,1,1,1,4),(191.637151868978,192.000400560574,193.000162202111,193.500043022879,
193.999923843648,194.999685485184,195.999447126721,196.999208768258,197.920337176158),
 .UNSPECIFIED.);
#457=B_SPLINE_CURVE_WITH_KNOTS('',3,(#39652,#39653,#39654,#39655,#39656,
#39657,#39658,#39659,#39660,#39661,#39662),.UNSPECIFIED.,.F.,.F.,(4,1,1,
1,1,1,1,1,4),(191.637151868979,191.943955127471,192.943716769007,193.943478410544,
194.943240052081,195.943001693617,196.942763335154,197.442644155923,197.920337176158),
 .UNSPECIFIED.);
#458=B_SPLINE_CURVE_WITH_KNOTS('',3,(#39667,#39668,#39669,#39670,#39671,
#39672,#39673,#39674,#39675,#39676,#39677),.UNSPECIFIED.,.F.,.F.,(4,1,1,
1,1,1,1,1,4),(185.353966561799,186.001830711354,186.501711532122,187.001592352891,
188.001353994427,189.001115635964,190.000877277501,191.000638919037,191.637151868978),
 .UNSPECIFIED.);
#459=B_SPLINE_CURVE_WITH_KNOTS('',3,(#39678,#39679,#39680,#39681,#39682,
#39683,#39684,#39685,#39686,#39687,#39688),.UNSPECIFIED.,.F.,.F.,(4,1,1,
1,1,1,1,1,4),(185.353966561799,185.94538527825,186.945146919787,187.944908561324,
188.94467020286,189.944431844397,190.444312665166,190.944193485934,191.637151868979),
 .UNSPECIFIED.);
#460=B_SPLINE_CURVE_WITH_KNOTS('',3,(#39693,#39694,#39695,#39696,#39697,
#39698,#39699,#39700,#39701,#39702,#39703),.UNSPECIFIED.,.F.,.F.,(4,1,1,
1,1,1,1,1,4),(179.070781254619,179.503380041365,180.003260862133,181.00302250367,
182.002784145207,183.002545786744,184.00230742828,185.002069069817,185.353966561799),
 .UNSPECIFIED.);
#461=B_SPLINE_CURVE_WITH_KNOTS('',3,(#39704,#39705,#39706,#39707,#39708,
#39709,#39710,#39711,#39712,#39713,#39714),.UNSPECIFIED.,.F.,.F.,(4,1,1,
1,1,1,1,1,4),(179.07078125462,179.94681542903,180.946577070567,181.946338712103,
182.94610035364,183.445981174408,183.945861995177,184.945623636714,185.353966561799),
 .UNSPECIFIED.);
#462=B_SPLINE_CURVE_WITH_KNOTS('',3,(#39719,#39720,#39721,#39722,#39723,
#39724,#39725,#39726,#39727,#39728,#39729),.UNSPECIFIED.,.F.,.F.,(4,1,1,
1,1,1,1,1,4),(172.78759594744,173.004929371376,174.004691012913,175.00445265445,
176.004214295987,177.003975937523,178.00373757906,179.003499220597,179.070781254619),
 .UNSPECIFIED.);
#463=B_SPLINE_CURVE_WITH_KNOTS('',3,(#39730,#39731,#39732,#39733,#39734,
#39735,#39736,#39737,#39738,#39739,#39740,#39741),.UNSPECIFIED.,.F.,.F.,
(4,1,1,1,1,1,1,1,1,4),(172.78759594744,172.948483938273,173.94824557981,
174.948007221346,175.947768862883,176.447649683651,176.94753050442,177.947292145957,
178.947053787493,179.07078125462),.UNSPECIFIED.);
#464=B_SPLINE_CURVE_WITH_KNOTS('',3,(#39746,#39747,#39748,#39749,#39750,
#39751,#39752,#39753,#39754,#39755,#39756),.UNSPECIFIED.,.F.,.F.,(4,1,1,
1,1,1,1,1,4),(166.50441064026,167.006359522156,168.006121163693,169.00588280523,
170.005644446766,171.005406088303,172.00516772984,172.505048550608,172.78759594744),
 .UNSPECIFIED.);
#465=B_SPLINE_CURVE_WITH_KNOTS('',3,(#39757,#39758,#39759,#39760,#39761,
#39762,#39763,#39764,#39765,#39766,#39767),.UNSPECIFIED.,.F.,.F.,(4,1,1,
1,1,1,1,1,4),(166.504410640261,166.949914089053,167.949675730589,168.949437372126,
169.449318192894,169.949199013663,170.9489606552,171.948722296736,172.78759594744),
 .UNSPECIFIED.);
#466=B_SPLINE_CURVE_WITH_KNOTS('',3,(#39772,#39773,#39774,#39775,#39776,
#39777,#39778,#39779,#39780,#39781,#39782),.UNSPECIFIED.,.F.,.F.,(4,1,1,
1,1,1,1,1,4),(160.22122533308,161.007789672936,162.007551314473,163.007312956009,
164.007074597546,165.006836239083,165.506717059851,166.006597880619,166.50441064026),
 .UNSPECIFIED.);
#467=B_SPLINE_CURVE_WITH_KNOTS('',3,(#39783,#39784,#39785,#39786,#39787,
#39788,#39789,#39790,#39791,#39792,#39793,#39794,#39795,#39796,#39797,#39798,
#39799,#39800,#39801,#39802,#39803,#39804),.UNSPECIFIED.,.F.,.F.,(4,3,3,
3,3,3,3,4),(160.221225333081,161.129702406698,162.038179480315,162.946656553932,
163.855133627549,164.763610701166,165.672087774783,166.504410640261),
 .UNSPECIFIED.);
#468=B_SPLINE_CURVE_WITH_KNOTS('',3,(#39809,#39810,#39811,#39812,#39813,
#39814,#39815,#39816,#39817,#39818,#39819,#39820),.UNSPECIFIED.,.F.,.F.,
(4,1,1,1,1,1,1,1,1,4),(153.938040025901,154.009458182179,155.009219823716,
156.008981465252,157.008743106789,158.008504748326,158.508385569094,159.008266389862,
160.008028031399,160.22122533308),.UNSPECIFIED.);
#469=B_SPLINE_CURVE_WITH_KNOTS('',3,(#39821,#39822,#39823,#39824,#39825,
#39826,#39827,#39828,#39829,#39830,#39831,#39832),.UNSPECIFIED.,.F.,.F.,
(4,1,1,1,1,1,1,1,1,4),(153.938040025902,153.953012749075,154.952774390612,
155.45265521138,155.952536032149,156.952297673685,157.952059315222,158.951820956759,
159.951582598296,160.221225333081),.UNSPECIFIED.);
#470=B_SPLINE_CURVE_WITH_KNOTS('',3,(#39837,#39838,#39839,#39840,#39841,
#39842,#39843,#39844,#39845,#39846,#39847),.UNSPECIFIED.,.F.,.F.,(4,1,1,
1,1,1,1,1,4),(147.654854718721,148.010888332959,149.010649974495,150.010411616032,
151.010173257569,151.510054078337,152.009934899105,153.009696540642,153.938040025901),
 .UNSPECIFIED.);
#471=B_SPLINE_CURVE_WITH_KNOTS('',3,(#39848,#39849,#39850,#39851,#39852,
#39853,#39854,#39855,#39856,#39857,#39858),.UNSPECIFIED.,.F.,.F.,(4,1,1,
1,1,1,1,1,4),(147.654854718722,147.954442899855,148.454323720623,148.954204541392,
149.953966182928,150.953727824465,151.953489466002,152.953251107539,153.938040025902),
 .UNSPECIFIED.);
#472=B_SPLINE_CURVE_WITH_KNOTS('',3,(#39863,#39864,#39865,#39866,#39867,
#39868,#39869,#39870,#39871,#39872,#39873),.UNSPECIFIED.,.F.,.F.,(4,1,1,
1,1,1,1,1,4),(141.371669411542,142.012318483738,143.012080125275,144.011841766812,
144.51172258758,145.011603408348,146.011365049885,147.011126691422,147.654854718721),
 .UNSPECIFIED.);
#473=B_SPLINE_CURVE_WITH_KNOTS('',3,(#39874,#39875,#39876,#39877,#39878,
#39879,#39880,#39881,#39882,#39883,#39884),.UNSPECIFIED.,.F.,.F.,(4,1,1,
1,1,1,1,1,4),(141.371669411542,141.455992229866,141.955873050635,142.955634692171,
143.955396333708,144.955157975245,145.954919616782,146.954681258318,147.654854718722),
 .UNSPECIFIED.);
#474=B_SPLINE_CURVE_WITH_KNOTS('',3,(#39889,#39890,#39891,#39892,#39893,
#39894,#39895,#39896,#39897,#39898,#39899),.UNSPECIFIED.,.F.,.F.,(4,1,1,
1,1,1,1,1,4),(135.088484104362,136.013748634518,137.013510276055,137.513391096823,
138.013271917591,139.013033559128,140.012795200665,141.012556842202,141.371669411542),
 .UNSPECIFIED.);
#475=B_SPLINE_CURVE_WITH_KNOTS('',3,(#39900,#39901,#39902,#39903,#39904,
#39905,#39906,#39907,#39908,#39909),.UNSPECIFIED.,.F.,.F.,(4,1,1,1,1,1,
1,4),(135.088484104363,135.957303201414,136.957064842951,137.956826484488,
138.956588126025,139.956349767561,140.956111409098,141.371669411542),
 .UNSPECIFIED.);
#476=B_SPLINE_CURVE_WITH_KNOTS('',3,(#39914,#39915,#39916,#39917,#39918,
#39919,#39920,#39921,#39922,#39923,#39924,#39925),.UNSPECIFIED.,.F.,.F.,
(4,1,1,1,1,1,1,1,1,4),(128.805298797183,129.015417143761,130.015178785298,
130.515059606066,131.014940426834,132.014702068371,133.014463709908,134.014225351445,
135.013986992981,135.088484104362),.UNSPECIFIED.);
#477=B_SPLINE_CURVE_WITH_KNOTS('',3,(#39926,#39927,#39928,#39929,#39930,
#39931,#39932,#39933,#39934,#39935,#39936,#39937),.UNSPECIFIED.,.F.,.F.,
(4,1,1,1,1,1,1,1,1,4),(128.805298797183,128.958971710657,129.958733352194,
130.958494993731,131.958256635268,132.958018276804,133.957779918341,134.457660739109,
134.957541559878,135.088484104363),.UNSPECIFIED.);
#478=B_SPLINE_CURVE_WITH_KNOTS('',3,(#39942,#39943,#39944,#39945,#39946,
#39947,#39948,#39949,#39950,#39951,#39952),.UNSPECIFIED.,.F.,.F.,(4,1,1,
1,1,1,1,1,4),(122.522113490003,123.016847294541,123.516728115309,124.016608936077,
125.016370577614,126.016132219151,127.015893860688,128.015655502224,128.805298797183),
 .UNSPECIFIED.);
#479=B_SPLINE_CURVE_WITH_KNOTS('',3,(#39953,#39954,#39955,#39956,#39957,
#39958,#39959,#39960,#39961,#39962,#39963),.UNSPECIFIED.,.F.,.F.,(4,1,1,
1,1,1,1,1,4),(122.522113490004,122.960401861437,123.960163502974,124.95992514451,
125.959686786047,126.959448427584,127.459329248352,127.959210069121,128.805298797183),
 .UNSPECIFIED.);
#480=B_SPLINE_CURVE_WITH_KNOTS('',3,(#39968,#39969,#39970,#39971,#39972,
#39973,#39974,#39975,#39976,#39977,#39978),.UNSPECIFIED.,.F.,.F.,(4,1,1,
1,1,1,1,1,4),(116.238928182823,116.518396624552,117.01827744532,118.018039086857,
119.017800728394,120.01756236993,121.017324011467,122.017085653004,122.522113490003),
 .UNSPECIFIED.);
#481=B_SPLINE_CURVE_WITH_KNOTS('',3,(#39979,#39980,#39981,#39982,#39983,
#39984,#39985,#39986,#39987,#39988,#39989,#39990,#39991,#39992,#39993,#39994,
#39995,#39996,#39997,#39998,#39999,#40000),.UNSPECIFIED.,.F.,.F.,(4,3,3,
3,3,3,3,4),(116.238928182824,117.147405256441,118.055882330058,118.964359403675,
119.872836477292,120.781313550909,121.689790624526,122.522113490004),
 .UNSPECIFIED.);
#482=B_SPLINE_CURVE_WITH_KNOTS('',3,(#40005,#40006,#40007,#40008,#40009,
#40010,#40011,#40012,#40013,#40014,#40015),.UNSPECIFIED.,.F.,.F.,(4,1,1,
1,1,1,1,1,4),(109.955742875644,110.019945954563,111.0197075961,112.019469237637,
113.019230879173,114.01899252071,115.018754162247,116.018515803784,116.238928182823),
 .UNSPECIFIED.);
#483=B_SPLINE_CURVE_WITH_KNOTS('',3,(#40016,#40017,#40018,#40019,#40020,
#40021,#40022,#40023,#40024,#40025,#40026,#40027),.UNSPECIFIED.,.F.,.F.,
(4,1,1,1,1,1,1,1,1,4),(109.955742875644,109.96350052146,110.963262162996,
111.963023804533,112.96278544607,113.462666266838,113.962547087607,114.962308729143,
115.96207037068,116.238928182824),.UNSPECIFIED.);
#484=B_SPLINE_CURVE_WITH_KNOTS('',3,(#40032,#40033,#40034,#40035,#40036,
#40037,#40038,#40039,#40040,#40041,#40042),.UNSPECIFIED.,.F.,.F.,(4,1,1,
1,1,1,1,1,4),(103.672557568464,104.021376105343,105.02113774688,106.020899388416,
107.020661029953,108.02042267149,109.020184313027,109.520065133795,109.955742875644),
 .UNSPECIFIED.);
#485=B_SPLINE_CURVE_WITH_KNOTS('',3,(#40043,#40044,#40045,#40046,#40047,
#40048,#40049,#40050,#40051,#40052,#40053),.UNSPECIFIED.,.F.,.F.,(4,1,1,
1,1,1,1,1,4),(103.672557568465,103.964930672239,104.964692313776,105.964453955313,
106.464334776081,106.96421559685,107.963977238386,108.963738879923,109.955742875644),
 .UNSPECIFIED.);
#486=B_SPLINE_CURVE_WITH_KNOTS('',3,(#40058,#40059,#40060,#40061,#40062,
#40063,#40064,#40065,#40066,#40067,#40068),.UNSPECIFIED.,.F.,.F.,(4,1,1,
1,1,1,1,1,4),(97.3893722612846,98.0228062561227,99.0225678976594,100.022329539196,
101.022091180733,102.02185282227,102.521733643038,103.021614463806,103.672557568464),
 .UNSPECIFIED.);
#487=B_SPLINE_CURVE_WITH_KNOTS('',3,(#40069,#40070,#40071,#40072,#40073,
#40074,#40075,#40076,#40077,#40078,#40079,#40080,#40081,#40082,#40083,#40084,
#40085,#40086,#40087,#40088,#40089,#40090),.UNSPECIFIED.,.F.,.F.,(4,3,3,
3,3,3,3,4),(97.3893722612853,98.2978493349022,99.2063264085192,100.114803482136,
101.023280555753,101.93175762937,102.840234702987,103.672557568465),
 .UNSPECIFIED.);
#488=B_SPLINE_CURVE_WITH_KNOTS('',3,(#40095,#40096,#40097,#40098,#40099,
#40100,#40101,#40102,#40103,#40104,#40105),.UNSPECIFIED.,.F.,.F.,(4,1,1,
1,1,1,1,1,4),(91.1061869541049,92.0242364069024,93.0239980484391,94.0237596899758,
95.0235213315126,95.5234021522809,96.0232829730493,97.023044614586,97.3893722612846),
 .UNSPECIFIED.);
#489=B_SPLINE_CURVE_WITH_KNOTS('',3,(#40106,#40107,#40108,#40109,#40110,
#40111,#40112,#40113,#40114,#40115,#40116),.UNSPECIFIED.,.F.,.F.,(4,1,1,
1,1,1,1,1,4),(91.1061869541057,91.9677909737988,92.4676717945672,92.9675526153355,
93.9673142568722,94.967075898409,95.9668375399457,96.9665991814824,97.3893722612853),
 .UNSPECIFIED.);
#490=B_SPLINE_CURVE_WITH_KNOTS('',3,(#40121,#40122,#40123,#40124,#40125,
#40126,#40127,#40128,#40129,#40130,#40131,#40132),.UNSPECIFIED.,.F.,.F.,
(4,1,1,1,1,1,1,1,1,4),(84.8230016469254,85.0259049161454,86.0256665576821,
87.0254281992188,88.0251898407555,88.5250706615239,89.0249514822923,90.024713123829,
91.0244747653657,91.1061869541049),.UNSPECIFIED.);
#491=B_SPLINE_CURVE_WITH_KNOTS('',3,(#40133,#40134,#40135,#40136,#40137,
#40138,#40139,#40140,#40141,#40142,#40143,#40144),.UNSPECIFIED.,.F.,.F.,
(4,1,1,1,1,1,1,1,1,4),(84.8230016469261,84.9694594830418,85.4693403038102,
85.9692211245785,86.9689827661152,87.9687444076519,88.9685060491887,89.9682676907254,
90.9680293322621,91.1061869541057),.UNSPECIFIED.);
#492=B_SPLINE_CURVE_WITH_KNOTS('',3,(#40149,#40150,#40151,#40152,#40153,
#40154,#40155,#40156,#40157,#40158,#40159),.UNSPECIFIED.,.F.,.F.,(4,1,1,
1,1,1,1,1,4),(78.5398163397458,79.0273350669251,80.0270967084618,81.0268583499985,
81.5267391707669,82.0266199915352,83.026381633072,84.0261432746087,84.8230016469254),
 .UNSPECIFIED.);
#493=B_SPLINE_CURVE_WITH_KNOTS('',3,(#40160,#40161,#40162,#40163,#40164,
#40165,#40166,#40167,#40168,#40169),.UNSPECIFIED.,.F.,.F.,(4,1,1,1,1,1,
1,4),(78.5398163397465,78.9708896338215,79.9706512753582,80.9704129168949,
81.9701745584316,82.9699361999684,83.9696978415051,84.8230016469261),
 .UNSPECIFIED.);
#494=B_SPLINE_CURVE_WITH_KNOTS('',3,(#40174,#40175,#40176,#40177,#40178,
#40179,#40180,#40181,#40182,#40183,#40184),.UNSPECIFIED.,.F.,.F.,(4,1,1,
1,1,1,1,1,4),(72.2566310325663,73.0287652177048,74.0285268592415,74.5284076800099,
75.0282885007782,76.028050142315,77.0278117838517,78.0275734253884,78.5398163397458),
 .UNSPECIFIED.);
#495=B_SPLINE_CURVE_WITH_KNOTS('',3,(#40185,#40186,#40187,#40188,#40189,
#40190,#40191,#40192,#40193,#40194,#40195),.UNSPECIFIED.,.F.,.F.,(4,1,1,
1,1,1,1,1,4),(72.2566310325669,72.9723197846012,73.9720814261379,74.9718430676746,
75.9716047092113,76.971366350748,77.9711279922848,78.4710088130531,78.5398163397465),
 .UNSPECIFIED.);
#496=B_SPLINE_CURVE_WITH_KNOTS('',3,(#40200,#40201,#40202,#40203,#40204,
#40205,#40206,#40207,#40208,#40209,#40210,#40211),.UNSPECIFIED.,.F.,.F.,
(4,1,1,1,1,1,1,1,1,4),(65.9734457253866,66.0304337269478,67.0301953684845,
67.5300761892529,68.0299570100212,69.0297186515579,70.0294802930947,71.0292419346314,
72.0290035761681,72.2566310325663),.UNSPECIFIED.);
#497=B_SPLINE_CURVE_WITH_KNOTS('',3,(#40212,#40213,#40214,#40215,#40216,
#40217,#40218,#40219,#40220,#40221,#40222,#40223),.UNSPECIFIED.,.F.,.F.,
(4,1,1,1,1,1,1,1,1,4),(65.9734457253873,65.9739882938441,66.9737499353809,
67.9735115769176,68.9732732184543,69.973034859991,70.9727965015277,71.4726773222961,
71.9725581430645,72.2566310325669),.UNSPECIFIED.);
#498=B_SPLINE_CURVE_WITH_KNOTS('',3,(#40228,#40229,#40230,#40231,#40232,
#40233,#40234,#40235,#40236,#40237,#40238),.UNSPECIFIED.,.F.,.F.,(4,1,1,
1,1,1,1,1,4),(59.690260418207,60.0318638777275,60.5317446984958,61.0316255192642,
62.0313871608009,63.0311488023376,64.0309104438743,65.0306720854111,65.9734457253866),
 .UNSPECIFIED.);
#499=B_SPLINE_CURVE_WITH_KNOTS('',3,(#40239,#40240,#40241,#40242,#40243,
#40244,#40245,#40246,#40247,#40248,#40249),.UNSPECIFIED.,.F.,.F.,(4,1,1,
1,1,1,1,1,4),(59.6902604182077,59.9754184446238,60.9751800861606,61.9749417276973,
62.974703369234,63.9744650107707,64.4743458315391,64.9742266523074,65.9734457253873),
 .UNSPECIFIED.);
#500=B_SPLINE_CURVE_WITH_KNOTS('',3,(#40254,#40255,#40256,#40257,#40258,
#40259,#40260,#40261,#40262,#40263,#40264),.UNSPECIFIED.,.F.,.F.,(4,1,1,
1,1,1,1,1,4),(53.4070751110275,53.5334132077388,54.0332940285072,55.0330556700439,
56.0328173115806,57.0325789531173,58.0323405946541,59.0321022361908,59.690260418207),
 .UNSPECIFIED.);
#501=B_SPLINE_CURVE_WITH_KNOTS('',3,(#40265,#40266,#40267,#40268,#40269,
#40270,#40271,#40272,#40273,#40274,#40275,#40276,#40277,#40278,#40279,#40280,
#40281,#40282,#40283,#40284,#40285,#40286),.UNSPECIFIED.,.F.,.F.,(4,3,3,
3,3,3,3,4),(53.4070751110281,54.315552184645,55.224029258262,56.1325063318789,
57.0409834054958,57.9494604791127,58.8579375527296,59.6902604182077),
 .UNSPECIFIED.);
#502=B_SPLINE_CURVE_WITH_KNOTS('',3,(#40291,#40292,#40293,#40294,#40295,
#40296,#40297,#40298,#40299,#40300),.UNSPECIFIED.,.F.,.F.,(4,1,1,1,1,1,
1,4),(47.1238898038478,48.0347241792869,49.0344858208236,50.0342474623603,
51.034009103897,52.0337707454337,53.0335323869705,53.4070751110275),
 .UNSPECIFIED.);
#503=B_SPLINE_CURVE_WITH_KNOTS('',3,(#40301,#40302,#40303,#40304,#40305,
#40306,#40307,#40308,#40309,#40310,#40311),.UNSPECIFIED.,.F.,.F.,(4,1,1,
1,1,1,1,1,4),(47.1238898038486,47.9782787461832,48.9780403877199,49.9778020292567,
50.477682850025,50.9775636707934,51.9773253123301,52.9770869538668,53.4070751110281),
 .UNSPECIFIED.);
#504=B_SPLINE_CURVE_WITH_KNOTS('',3,(#40316,#40317,#40318,#40319,#40320,
#40321,#40322,#40323,#40324,#40325,#40326,#40327),.UNSPECIFIED.,.F.,.F.,
(4,1,1,1,1,1,1,1,1,4),(40.8407044966682,41.0363926885299,42.0361543300666,
43.0359159716033,44.03567761314,45.0354392546767,46.0352008962134,46.5350817169818,
47.0349625377502,47.1238898038478),.UNSPECIFIED.);
#505=B_SPLINE_CURVE_WITH_KNOTS('',3,(#40328,#40329,#40330,#40331,#40332,
#40333,#40334,#40335,#40336,#40337,#40338,#40339),.UNSPECIFIED.,.F.,.F.,
(4,1,1,1,1,1,1,1,1,4),(40.8407044966689,40.9799472554262,41.9797088969629,
42.9794705384996,43.479351359268,43.9792321800364,44.9789938215731,45.9787554631098,
46.9785171046465,47.1238898038486),.UNSPECIFIED.);
#506=B_SPLINE_CURVE_WITH_KNOTS('',3,(#40344,#40345,#40346,#40347,#40348,
#40349,#40350,#40351,#40352,#40353,#40354),.UNSPECIFIED.,.F.,.F.,(4,1,1,
1,1,1,1,1,4),(34.5575191894887,35.0378228393096,36.0375844808463,37.037346122383,
38.0371077639197,39.0368694054564,39.5367502262248,40.0366310469931,40.8407044966682),
 .UNSPECIFIED.);
#507=B_SPLINE_CURVE_WITH_KNOTS('',3,(#40355,#40356,#40357,#40358,#40359,
#40360,#40361,#40362,#40363,#40364,#40365),.UNSPECIFIED.,.F.,.F.,(4,1,1,
1,1,1,1,1,4),(34.5575191894893,34.9813774062059,35.9811390477426,36.481019868511,
36.9809006892793,37.980662330816,38.9804239723528,39.9801856138895,40.8407044966689),
 .UNSPECIFIED.);
#508=B_SPLINE_CURVE_WITH_KNOTS('',3,(#40370,#40371,#40372,#40373,#40374,
#40375,#40376,#40377,#40378,#40379,#40380),.UNSPECIFIED.,.F.,.F.,(4,1,1,
1,1,1,1,1,4),(28.2743338823091,29.0392529900893,30.039014631626,31.0387762731627,
32.0385379146994,32.5384187354678,33.0382995562361,34.0380611977728,34.5575191894887),
 .UNSPECIFIED.);
#509=B_SPLINE_CURVE_WITH_KNOTS('',3,(#40381,#40382,#40383,#40384,#40385,
#40386,#40387,#40388,#40389,#40390,#40391),.UNSPECIFIED.,.F.,.F.,(4,1,1,
1,1,1,1,1,4),(28.2743338823098,28.9828075569856,29.4826883777539,29.9825691985223,
30.982330840059,31.9820924815957,32.9818541231325,33.9816157646692,34.5575191894893),
 .UNSPECIFIED.);
#510=B_SPLINE_CURVE_WITH_KNOTS('',3,(#40396,#40397,#40398,#40399,#40400,
#40401,#40402,#40403,#40404,#40405,#40406,#40407),.UNSPECIFIED.,.F.,.F.,
(4,1,1,1,1,1,1,1,1,4),(21.9911485751295,22.0409214993322,23.040683140869,
24.0404447824057,25.0402064239424,25.5400872447107,26.0399680654791,27.0397297070158,
28.0394913485525,28.2743338823091),.UNSPECIFIED.);
#511=B_SPLINE_CURVE_WITH_KNOTS('',3,(#40408,#40409,#40410,#40411,#40412,
#40413,#40414,#40415,#40416,#40417,#40418),.UNSPECIFIED.,.F.,.F.,(4,1,1,
1,1,1,1,1,4),(21.9911485751302,22.4843568869969,22.9842377077653,23.983999349302,
24.9837609908387,25.9835226323754,26.9832842739122,27.9830459154489,28.2743338823098),
 .UNSPECIFIED.);
#512=B_SPLINE_CURVE_WITH_KNOTS('',3,(#40423,#40424,#40425,#40426,#40427,
#40428,#40429,#40430,#40431,#40432,#40433),.UNSPECIFIED.,.F.,.F.,(4,1,1,
1,1,1,1,1,4),(15.7079632679499,16.0423516501119,17.0421132916487,18.0418749331854,
18.5417557539537,19.0416365747221,20.0413982162588,21.0411598577955,21.9911485751295),
 .UNSPECIFIED.);
#513=B_SPLINE_CURVE_WITH_KNOTS('',3,(#40434,#40435,#40436,#40437,#40438,
#40439,#40440,#40441,#40442,#40443,#40444),.UNSPECIFIED.,.F.,.F.,(4,1,1,
1,1,1,1,1,4),(15.7079632679505,15.9859062170083,16.985667858545,17.9854295000817,
18.9851911416184,19.9849527831551,20.9847144246918,21.9844760662286,21.9911485751302),
 .UNSPECIFIED.);
#514=B_SPLINE_CURVE_WITH_KNOTS('',3,(#40469,#40470,#40471,#40472,#40473,
#40474,#40475,#40476,#40477,#40478,#40479,#40480,#40481,#40482,#40483,#40484,
#40485,#40486,#40487,#40488,#40489,#40490,#40491,#40492,#40493,#40494,#40495,
#40496,#40497,#40498,#40499,#40500,#40501,#40502,#40503,#40504,#40505,#40506,
#40507,#40508,#40509,#40510,#40511,#40512,#40513,#40514,#40515,#40516,#40517,
#40518,#40519,#40520,#40521,#40522,#40523,#40524,#40525,#40526),
 .UNSPECIFIED.,.F.,.F.,(4,3,3,3,3,3,3,3,3,3,3,3,3,3,3,3,3,3,3,4),(-0.694415684853046,
-0.651517903549149,-0.607914821239224,-0.56365275566676,-0.518801975968359,
-0.5037477542567,-0.493849355084242,-0.446277542502629,-0.397620428148984,
-0.35840958277914,-0.313608384931747,-0.294007860873513,-0.285041234230192,
-0.276619367837676,-0.224941839812129,-0.172301174308133,-0.118270567804678,
-0.0635860442762699,-0.00841504377438129,0.),.UNSPECIFIED.);
#515=B_SPLINE_CURVE_WITH_KNOTS('',3,(#40527,#40528,#40529,#40530,#40531,
#40532,#40533,#40534,#40535,#40536,#40537,#40538,#40539,#40540,#40541,#40542,
#40543,#40544,#40545,#40546,#40547,#40548,#40549,#40550,#40551,#40552,#40553,
#40554,#40555,#40556,#40557,#40558,#40559,#40560,#40561,#40562,#40563,#40564,
#40565,#40566,#40567,#40568,#40569,#40570,#40571,#40572,#40573,#40574,#40575,
#40576,#40577,#40578),.UNSPECIFIED.,.F.,.F.,(4,3,3,3,3,3,3,3,3,3,3,3,3,
3,3,3,3,4),(-0.689375724006324,-0.634260226335645,-0.579590449708639,-0.525633818728872,
-0.470565042052615,-0.44680280770273,-0.438973044842247,-0.388760986671672,
-0.339371186895675,-0.305358712023844,-0.25794484133391,-0.22489097506966,
-0.215263201343678,-0.170398777370464,-0.126568635661146,-0.0833490831487066,
-0.0410882702651496,0.),.UNSPECIFIED.);
#516=B_SPLINE_CURVE_WITH_KNOTS('',3,(#43481,#43482,#43483,#43484,#43485,
#43486,#43487,#43488),.UNSPECIFIED.,.F.,.F.,(4,1,1,1,1,4),(12.0433050839651,
12.5431859047334,13.0430667255018,14.0428283670385,15.0425900085752,15.7079632679499),
 .UNSPECIFIED.);
#517=B_SPLINE_CURVE_WITH_KNOTS('',3,(#43489,#43490,#43491,#43492,#43493,
#43494,#43495,#43496,#43497,#43498,#43499,#43500,#43501,#43502,#43503,#43504,
#43505,#43506,#43507,#43508,#43509,#43510,#43511,#43512,#43513,#43514,#43515,
#43516,#43517,#43518,#43519,#43520,#43521,#43522,#43523,#43524,#43525,#43526,
#43527,#43528,#43529,#43530,#43531,#43532,#43533,#43534,#43535,#43536,#43537,
#43538,#43539,#43540,#43541,#43542,#43543,#43544,#43545,#43546,#43547,#43548,
#43549),.UNSPECIFIED.,.F.,.F.,(4,3,3,3,3,3,3,3,3,3,3,3,3,3,3,3,3,3,3,3,
4),(0.,0.0551258591420952,0.109754210237386,0.163556354459871,0.21588036197585,
0.25151266717677,0.280554162019188,0.289557091917646,0.338951994283204,
0.35840958277953,0.407098532341802,0.454999930760489,0.484939548121938,
0.498910397309242,0.507155395896732,0.557573774787132,0.59180954850337,
0.613641770187594,0.63416209310979,0.680471724035206,0.694516869652084),
 .UNSPECIFIED.);
#518=B_SPLINE_CURVE_WITH_KNOTS('',3,(#43552,#43553,#43554,#43555,#43556,
#43557,#43558,#43559,#43560,#43561,#43562),.UNSPECIFIED.,.F.,.F.,(4,1,1,
1,1,1,1,1,4),(9.9478434911665,9.98733636778795,10.9870980093247,11.9868596508614,
12.9866212923981,13.9863829339348,14.9861445754715,15.4860253962399,15.7079632679505),
 .UNSPECIFIED.);
#519=B_SPLINE_CURVE_WITH_KNOTS('',3,(#43565,#43566,#43567,#43568,#43569,
#43570,#43571,#43572,#43573,#43574),.UNSPECIFIED.,.F.,.F.,(4,3,3,4),(-0.104077581167986,
-0.0617457737573955,-0.0189375188380278,-0.000362254369400641),
 .UNSPECIFIED.);
#520=B_SPLINE_CURVE_WITH_KNOTS('',3,(#43577,#43578,#43579,#43580,#43581,
#43582,#43583,#43584,#43585,#43586),.UNSPECIFIED.,.F.,.F.,(4,3,3,4),(1.13119827306084,
1.17364379143339,1.21521247145906,1.23499833094825),.UNSPECIFIED.);
#521=B_SPLINE_CURVE_WITH_KNOTS('',3,(#44096,#44097,#44098,#44099,#44100,
#44101,#44102),.UNSPECIFIED.,.F.,.F.,(4,1,1,1,4),(13.9661186601203,14.4600465471847,
14.9539744342492,15.4479023213137,15.707963267949),.UNSPECIFIED.);
#522=B_SPLINE_CURVE_WITH_KNOTS('',3,(#44103,#44104,#44105,#44106,#44107,
#44108,#44109,#44110,#44111,#44112,#44113,#44114,#44115,#44116,#44117,#44118,
#44119,#44120,#44121),.UNSPECIFIED.,.F.,.F.,(4,3,3,3,3,3,4),(-75.213176656116,
-74.7192487690515,-74.2253208819871,-73.7313929949226,-73.2374651078581,
-72.7435372207936,-72.2566310325651),.UNSPECIFIED.);
#523=B_SPLINE_CURVE_WITH_KNOTS('',3,(#44122,#44123,#44124,#44125,#44126,
#44127,#44128,#44129,#44130,#44131),.UNSPECIFIED.,.F.,.F.,(4,3,3,4),(-1.2345266614268,
-1.18927506134227,-1.14422754617811,-1.13094109509773),.UNSPECIFIED.);
#524=B_SPLINE_CURVE_WITH_KNOTS('',3,(#44134,#44135,#44136,#44137,#44138,
#44139,#44140,#44141,#44142,#44143),.UNSPECIFIED.,.F.,.F.,(4,3,3,4),(0.,
0.0450425198133127,0.0896231119338811,0.103234008807617),.UNSPECIFIED.);
#525=B_SPLINE_CURVE_WITH_KNOTS('',3,(#44146,#44147,#44148,#44149,#44150),
 .UNSPECIFIED.,.F.,.F.,(4,1,4),(15.2058131232128,15.4893404554446,15.707963267949),
 .UNSPECIFIED.);
#526=B_SPLINE_CURVE_WITH_KNOTS('',3,(#44661,#44662,#44663,#44664,#44665,
#44666,#44667,#44668,#44669,#44670,#44671,#44672,#44673,#44674,#44675,#44676,
#44677,#44678,#44679,#44680,#44681,#44682,#44683,#44684,#44685,#44686,#44687,
#44688,#44689,#44690,#44691,#44692,#44693,#44694,#44695,#44696,#44697,#44698,
#44699,#44700,#44701,#44702,#44703,#44704,#44705,#44706,#44707,#44708,#44709,
#44710,#44711,#44712,#44713,#44714,#44715,#44716,#44717,#44718),
 .UNSPECIFIED.,.F.,.F.,(4,3,3,3,3,3,3,3,3,3,3,3,3,3,3,3,3,3,3,4),(-0.000126486984424551,
0.0380591628916226,0.0717539043258247,0.087077502336768,0.108257623455665,
0.157532895597737,0.194489349704291,0.21378887858042,0.225593456009171,
0.272971435314458,0.305358712023953,0.354854209826148,0.404963477880151,
0.440515008646049,0.449592202308796,0.502330952057729,0.556359025569192,
0.610979682449441,0.666132005565916,0.689375724007338),.UNSPECIFIED.);
#527=B_SPLINE_CURVE_WITH_KNOTS('',3,(#47619,#47620,#47621,#47622,#47623,
#47624,#47625),.UNSPECIFIED.,.F.,.F.,(4,3,4),(628.755733952479,629.586155179399,
629.889327044754),.UNSPECIFIED.);
#528=SPHERICAL_SURFACE('',#20866,3.828125);
#529=SPHERICAL_SURFACE('',#20923,3.828125);
#530=SPHERICAL_SURFACE('',#20925,3.828125);
#531=SPHERICAL_SURFACE('',#20927,3.828125);
#532=SPHERICAL_SURFACE('',#20929,3.828125);
#533=SPHERICAL_SURFACE('',#20931,3.828125);
#534=SPHERICAL_SURFACE('',#20933,3.828125);
#535=SPHERICAL_SURFACE('',#20935,3.828125);
#536=CONICAL_SURFACE('',#20738,13.867180376262,0.891067654753264);
#537=CONICAL_SURFACE('',#20759,12.7315647249454,0.891067654753261);
#538=CONICAL_SURFACE('',#20800,14.7602281873362,1.22173047639603);
#539=CONICAL_SURFACE('',#20802,14.7602281873362,1.22173047639603);
#540=CONICAL_SURFACE('',#20804,14.7602281873362,1.22173047639603);
#541=CONICAL_SURFACE('',#20806,14.7602281873362,1.22173047639603);
#542=CONICAL_SURFACE('',#20808,14.7602281873362,1.22173047639603);
#543=CONICAL_SURFACE('',#20810,14.7602281873362,1.22173047639603);
#544=CONICAL_SURFACE('',#20812,14.7602281873362,1.22173047639603);
#545=CONICAL_SURFACE('',#20814,14.7602281873362,1.22173047639603);
#546=CONICAL_SURFACE('',#20816,14.5602281873362,0.349065850398871);
#547=CONICAL_SURFACE('',#20818,14.5602281873362,0.349065850398871);
#548=CONICAL_SURFACE('',#20820,14.5602281873362,0.349065850398871);
#549=CONICAL_SURFACE('',#20822,14.5602281873362,0.349065850398871);
#550=CONICAL_SURFACE('',#20824,14.5602281873362,0.349065850398871);
#551=CONICAL_SURFACE('',#20826,14.5602281873362,0.349065850398871);
#552=CONICAL_SURFACE('',#20828,14.5602281873362,0.349065850398871);
#553=CONICAL_SURFACE('',#20830,14.5602281873362,0.349065850398871);
#554=CONICAL_SURFACE('',#20832,14.4779295903485,0.610865238198015);
#555=CONICAL_SURFACE('',#20833,14.4779295903485,0.610865238198015);
#556=CONICAL_SURFACE('',#20834,14.4779295903485,0.610865238198015);
#557=CONICAL_SURFACE('',#20835,14.4779295903485,0.610865238198015);
#558=CONICAL_SURFACE('',#20836,14.4779295903485,0.610865238198015);
#559=CONICAL_SURFACE('',#20837,14.4779295903485,0.610865238198015);
#560=CONICAL_SURFACE('',#20838,14.4779295903485,0.610865238198015);
#561=CONICAL_SURFACE('',#20839,14.4779295903485,0.610865238198015);
#562=CONICAL_SURFACE('',#20877,5.,0.122173047639596);
#563=CONICAL_SURFACE('',#20882,5.10805041359455,0.122173047639596);
#564=CONICAL_SURFACE('',#20909,16.796875,1.44862327915528);
#565=CONICAL_SURFACE('',#20911,17.0170281388728,1.44862327915529);
#566=CONICAL_SURFACE('',#20953,13.867180376262,0.891067654753264);
#567=CONICAL_SURFACE('',#20978,12.7315647249454,0.891067654753261);
#568=CONICAL_SURFACE('',#21014,14.7602281873362,1.22173047639603);
#569=CONICAL_SURFACE('',#21016,14.7602281873362,1.22173047639603);
#570=CONICAL_SURFACE('',#21018,14.7602281873362,1.22173047639603);
#571=CONICAL_SURFACE('',#21020,14.7602281873362,1.22173047639603);
#572=CONICAL_SURFACE('',#21022,14.7602281873362,1.22173047639603);
#573=CONICAL_SURFACE('',#21024,14.7602281873362,1.22173047639603);
#574=CONICAL_SURFACE('',#21026,14.7602281873362,1.22173047639603);
#575=CONICAL_SURFACE('',#21028,14.7602281873362,1.22173047639603);
#576=CONICAL_SURFACE('',#21030,14.5602281873362,0.349065850398871);
#577=CONICAL_SURFACE('',#21032,14.5602281873362,0.349065850398871);
#578=CONICAL_SURFACE('',#21034,14.5602281873362,0.349065850398871);
#579=CONICAL_SURFACE('',#21036,14.5602281873362,0.349065850398871);
#580=CONICAL_SURFACE('',#21038,14.5602281873362,0.349065850398871);
#581=CONICAL_SURFACE('',#21040,14.5602281873362,0.349065850398871);
#582=CONICAL_SURFACE('',#21042,14.5602281873362,0.349065850398871);
#583=CONICAL_SURFACE('',#21044,14.5602281873362,0.349065850398871);
#584=CONICAL_SURFACE('',#21046,14.4779295903485,0.610865238198015);
#585=CONICAL_SURFACE('',#21047,14.4779295903485,0.610865238198015);
#586=CONICAL_SURFACE('',#21048,14.4779295903485,0.610865238198015);
#587=CONICAL_SURFACE('',#21049,14.4779295903485,0.610865238198015);
#588=CONICAL_SURFACE('',#21050,14.4779295903485,0.610865238198015);
#589=CONICAL_SURFACE('',#21051,14.4779295903485,0.610865238198015);
#590=CONICAL_SURFACE('',#21052,14.4779295903485,0.610865238198015);
#591=CONICAL_SURFACE('',#21053,14.4779295903485,0.610865238198015);
#592=CONICAL_SURFACE('',#21639,4.50000000000001,0.785398163397439);
#593=CONICAL_SURFACE('',#21645,4.5,0.785398163397447);
#594=TOROIDAL_SURFACE('',#20731,8.781875,0.110000000000001);
#595=TOROIDAL_SURFACE('',#20734,9.6875,5.39274861573998);
#596=TOROIDAL_SURFACE('',#20740,14.3237119736335,0.726288026366507);
#597=TOROIDAL_SURFACE('',#20762,9.6875,4.84274861573998);
#598=TOROIDAL_SURFACE('',#20765,14.3237119736335,1.27628802636651);
#599=TOROIDAL_SURFACE('',#20868,12.03125,3.828125);
#600=TOROIDAL_SURFACE('',#20872,5.65395079699728,0.550000000000001);
#601=TOROIDAL_SURFACE('',#20884,5.65395079699728,0.550000000000001);
#602=TOROIDAL_SURFACE('',#20887,7.8875,0.55);
#603=TOROIDAL_SURFACE('',#20891,7.8875,0.55);
#604=TOROIDAL_SURFACE('',#20899,12.03125,3.828125);
#605=TOROIDAL_SURFACE('',#20906,16.95,0.55);
#606=TOROIDAL_SURFACE('',#20915,16.95,0.55);
#607=TOROIDAL_SURFACE('',#20937,12.03125,3.828125);
#608=TOROIDAL_SURFACE('',#20946,8.781875,0.110000000000001);
#609=TOROIDAL_SURFACE('',#20949,9.6875,5.39274861573998);
#610=TOROIDAL_SURFACE('',#20955,14.3237119736335,0.726288026366507);
#611=TOROIDAL_SURFACE('',#20974,9.6875,4.84274861573998);
#612=TOROIDAL_SURFACE('',#20979,14.3237119736335,1.27628802636651);
#613=SHAPE_REPRESENTATION_RELATIONSHIP('SRR','None',#48413,#624);
#614=SHAPE_REPRESENTATION_RELATIONSHIP('SRR','None',#48414,#625);
#615=SHAPE_REPRESENTATION_RELATIONSHIP('SRR','None',#48415,#626);
#616=SHAPE_REPRESENTATION_RELATIONSHIP('SRR','None',#48416,#627);
#617=SHAPE_REPRESENTATION_RELATIONSHIP('SRR','None',#48417,#628);
#618=SHAPE_REPRESENTATION_RELATIONSHIP('SRR','None',#48418,#629);
#619=SHAPE_REPRESENTATION_RELATIONSHIP('SRR','None',#48419,#630);
#620=SHAPE_REPRESENTATION_RELATIONSHIP('SRR','None',#48420,#631);
#621=SHAPE_REPRESENTATION_RELATIONSHIP('SRR','None',#48421,#632);
#622=SHAPE_REPRESENTATION_RELATIONSHIP('SRR','None',#48422,#633);
#623=SHAPE_REPRESENTATION_RELATIONSHIP('SRR','None',#48423,#634);
#624=ADVANCED_BREP_SHAPE_REPRESENTATION('',(#755,#756,#757),#48358);
#625=ADVANCED_BREP_SHAPE_REPRESENTATION('',(#758,#759,#760),#48359);
#626=ADVANCED_BREP_SHAPE_REPRESENTATION('',(#761,#762,#763,#764,#765,#766,
#767,#768,#769,#770,#771,#772),#48360);
#627=ADVANCED_BREP_SHAPE_REPRESENTATION('',(#773),#48361);
#628=ADVANCED_BREP_SHAPE_REPRESENTATION('',(#774),#48362);
#629=ADVANCED_BREP_SHAPE_REPRESENTATION('',(#775),#48363);
#630=ADVANCED_BREP_SHAPE_REPRESENTATION('',(#776),#48364);
#631=ADVANCED_BREP_SHAPE_REPRESENTATION('',(#777),#48365);
#632=ADVANCED_BREP_SHAPE_REPRESENTATION('',(#778),#48366);
#633=ADVANCED_BREP_SHAPE_REPRESENTATION('',(#779),#48367);
#634=ADVANCED_BREP_SHAPE_REPRESENTATION('',(#780),#48368);
#635=FACE_BOUND('',#2301,.T.);
#636=FACE_BOUND('',#2302,.T.);
#637=FACE_BOUND('',#2310,.T.);
#638=FACE_BOUND('',#2311,.T.);
#639=FACE_BOUND('',#2320,.T.);
#640=FACE_BOUND('',#2321,.T.);
#641=FACE_BOUND('',#2331,.T.);
#642=FACE_BOUND('',#2332,.T.);
#643=FACE_BOUND('',#2435,.T.);
#644=FACE_BOUND('',#2436,.T.);
#645=FACE_BOUND('',#2444,.T.);
#646=FACE_BOUND('',#2445,.T.);
#647=FACE_BOUND('',#2454,.T.);
#648=FACE_BOUND('',#2455,.T.);
#649=FACE_BOUND('',#2465,.T.);
#650=FACE_BOUND('',#2466,.T.);
#651=FACE_BOUND('',#2552,.T.);
#652=FACE_BOUND('',#2554,.T.);
#653=FACE_BOUND('',#2591,.T.);
#654=FACE_BOUND('',#2593,.T.);
#655=FACE_BOUND('',#2603,.T.);
#656=FACE_BOUND('',#2605,.T.);
#657=FACE_BOUND('',#2647,.T.);
#658=FACE_BOUND('',#2649,.T.);
#659=FACE_BOUND('',#2914,.T.);
#660=FACE_BOUND('',#2915,.T.);
#661=FACE_BOUND('',#2916,.T.);
#662=FACE_BOUND('',#2917,.T.);
#663=FACE_BOUND('',#2918,.T.);
#664=FACE_BOUND('',#2919,.T.);
#665=FACE_BOUND('',#2920,.T.);
#666=FACE_BOUND('',#2921,.T.);
#667=FACE_BOUND('',#2922,.T.);
#668=FACE_BOUND('',#2923,.T.);
#669=FACE_BOUND('',#2924,.T.);
#670=FACE_BOUND('',#2925,.T.);
#671=FACE_BOUND('',#2926,.T.);
#672=FACE_BOUND('',#2966,.T.);
#673=FACE_BOUND('',#2967,.T.);
#674=FACE_BOUND('',#2968,.T.);
#675=FACE_BOUND('',#2969,.T.);
#676=FACE_BOUND('',#2970,.T.);
#677=FACE_BOUND('',#2971,.T.);
#678=FACE_BOUND('',#2972,.T.);
#679=FACE_BOUND('',#2973,.T.);
#680=FACE_BOUND('',#2974,.T.);
#681=FACE_BOUND('',#2975,.T.);
#682=FACE_BOUND('',#2976,.T.);
#683=FACE_BOUND('',#2977,.T.);
#684=FACE_BOUND('',#2978,.T.);
#685=FACE_BOUND('',#3207,.T.);
#686=FACE_BOUND('',#3211,.T.);
#687=FACE_BOUND('',#3218,.T.);
#688=FACE_BOUND('',#3222,.T.);
#689=FACE_BOUND('',#3245,.T.);
#690=FACE_BOUND('',#3249,.T.);
#691=FACE_BOUND('',#3252,.T.);
#692=FACE_BOUND('',#3253,.T.);
#693=FACE_BOUND('',#3254,.T.);
#694=FACE_BOUND('',#3255,.T.);
#695=FACE_BOUND('',#3256,.T.);
#696=FACE_BOUND('',#3257,.T.);
#697=FACE_BOUND('',#3258,.T.);
#698=FACE_BOUND('',#3259,.T.);
#699=FACE_BOUND('',#3261,.T.);
#700=FACE_BOUND('',#3262,.T.);
#701=FACE_BOUND('',#3263,.T.);
#702=FACE_BOUND('',#3264,.T.);
#703=FACE_BOUND('',#3265,.T.);
#704=FACE_BOUND('',#3266,.T.);
#705=FACE_BOUND('',#3267,.T.);
#706=FACE_BOUND('',#3268,.T.);
#707=FACE_BOUND('',#3274,.T.);
#708=FACE_BOUND('',#3275,.T.);
#709=FACE_BOUND('',#3276,.T.);
#710=FACE_BOUND('',#3277,.T.);
#711=FACE_BOUND('',#3278,.T.);
#712=FACE_BOUND('',#3279,.T.);
#713=FACE_BOUND('',#3280,.T.);
#714=FACE_BOUND('',#3281,.T.);
#715=FACE_BOUND('',#3282,.T.);
#716=FACE_BOUND('',#3283,.T.);
#717=FACE_BOUND('',#3284,.T.);
#718=FACE_BOUND('',#3285,.T.);
#719=FACE_BOUND('',#3286,.T.);
#720=FACE_BOUND('',#3287,.T.);
#721=FACE_BOUND('',#3288,.T.);
#722=FACE_BOUND('',#3289,.T.);
#723=FACE_BOUND('',#3332,.T.);
#724=FACE_BOUND('',#3334,.T.);
#725=FACE_BOUND('',#3341,.T.);
#726=FACE_BOUND('',#3343,.T.);
#727=FACE_BOUND('',#3350,.T.);
#728=FACE_BOUND('',#3352,.T.);
#729=STYLED_ITEM('',(#48510),#755);
#730=STYLED_ITEM('',(#48510),#756);
#731=STYLED_ITEM('',(#48510),#757);
#732=STYLED_ITEM('',(#48531),#758);
#733=STYLED_ITEM('',(#48531),#759);
#734=STYLED_ITEM('',(#48531),#760);
#735=STYLED_ITEM('',(#48517),#761);
#736=STYLED_ITEM('',(#48517),#762);
#737=STYLED_ITEM('',(#48517),#763);
#738=STYLED_ITEM('',(#48517),#764);
#739=STYLED_ITEM('',(#48517),#765);
#740=STYLED_ITEM('',(#48517),#766);
#741=STYLED_ITEM('',(#48517),#767);
#742=STYLED_ITEM('',(#48517),#768);
#743=STYLED_ITEM('',(#48517),#769);
#744=STYLED_ITEM('',(#48517),#770);
#745=STYLED_ITEM('',(#48517),#771);
#746=STYLED_ITEM('',(#48517),#772);
#747=STYLED_ITEM('',(#48531),#773);
#748=STYLED_ITEM('',(#48524),#774);
#749=STYLED_ITEM('',(#48496),#775);
#750=STYLED_ITEM('',(#48531),#776);
#751=STYLED_ITEM('',(#48496),#777);
#752=STYLED_ITEM('',(#48496),#778);
#753=STYLED_ITEM('',(#48524),#779);
#754=STYLED_ITEM('',(#48510),#780);
#755=MANIFOLD_SOLID_BREP('Body1',#20108);
#756=MANIFOLD_SOLID_BREP('Body2',#20109);
#757=MANIFOLD_SOLID_BREP('Body3',#20110);
#758=MANIFOLD_SOLID_BREP('Body1',#20111);
#759=MANIFOLD_SOLID_BREP('Body2',#20112);
#760=MANIFOLD_SOLID_BREP('Body3',#20113);
#761=MANIFOLD_SOLID_BREP('Body1',#20114);
#762=MANIFOLD_SOLID_BREP('Body2',#20115);
#763=MANIFOLD_SOLID_BREP('Body3',#20116);
#764=MANIFOLD_SOLID_BREP('Body4',#20117);
#765=MANIFOLD_SOLID_BREP('Body5',#20118);
#766=MANIFOLD_SOLID_BREP('Body6',#20119);
#767=MANIFOLD_SOLID_BREP('Body7',#20120);
#768=MANIFOLD_SOLID_BREP('Body8',#20121);
#769=MANIFOLD_SOLID_BREP('Body9',#20122);
#770=MANIFOLD_SOLID_BREP('Body10',#20123);
#771=MANIFOLD_SOLID_BREP('Body11',#20124);
#772=MANIFOLD_SOLID_BREP('Body12',#20125);
#773=MANIFOLD_SOLID_BREP('V_Slot',#20126);
#774=MANIFOLD_SOLID_BREP('Screw',#20127);
#775=MANIFOLD_SOLID_BREP('Middle_Block',#20128);
#776=MANIFOLD_SOLID_BREP('Rail_02',#20129);
#777=MANIFOLD_SOLID_BREP('Front_Block',#20130);
#778=MANIFOLD_SOLID_BREP('Back_Block',#20131);
#779=MANIFOLD_SOLID_BREP('Screw_Holder',#20132);
#780=MANIFOLD_SOLID_BREP('Rail_01',#20133);
#781=CYLINDRICAL_SURFACE('',#20276,0.45000000000016);
#782=CYLINDRICAL_SURFACE('',#20278,2.46743797397104);
#783=CYLINDRICAL_SURFACE('',#20280,0.724999999999998);
#784=CYLINDRICAL_SURFACE('',#20283,0.59999999999997);
#785=CYLINDRICAL_SURFACE('',#20285,2.36402292474775);
#786=CYLINDRICAL_SURFACE('',#20287,1.39999999999995);
#787=CYLINDRICAL_SURFACE('',#20290,1.04999999999995);
#788=CYLINDRICAL_SURFACE('',#20293,1.04999999999981);
#789=CYLINDRICAL_SURFACE('',#20303,1.04999999999996);
#790=CYLINDRICAL_SURFACE('',#20311,0.450000000000123);
#791=CYLINDRICAL_SURFACE('',#20313,2.46743797397101);
#792=CYLINDRICAL_SURFACE('',#20315,0.72500000000001);
#793=CYLINDRICAL_SURFACE('',#20318,0.599999999999987);
#794=CYLINDRICAL_SURFACE('',#20320,2.3640229247478);
#795=CYLINDRICAL_SURFACE('',#20322,1.39999999999978);
#796=CYLINDRICAL_SURFACE('',#20325,1.05);
#797=CYLINDRICAL_SURFACE('',#20329,0.45000000000016);
#798=CYLINDRICAL_SURFACE('',#20332,2.46743797397104);
#799=CYLINDRICAL_SURFACE('',#20335,0.724999999999998);
#800=CYLINDRICAL_SURFACE('',#20339,0.59999999999997);
#801=CYLINDRICAL_SURFACE('',#20342,2.36402292474775);
#802=CYLINDRICAL_SURFACE('',#20365,2.16656587073651);
#803=CYLINDRICAL_SURFACE('',#20387,2.16656587073651);
#804=CYLINDRICAL_SURFACE('',#20388,3.00000000000001);
#805=CYLINDRICAL_SURFACE('',#20390,3.00000000000001);
#806=CYLINDRICAL_SURFACE('',#20392,3.00000000000001);
#807=CYLINDRICAL_SURFACE('',#20394,3.00000000000001);
#808=CYLINDRICAL_SURFACE('',#20400,1.04999999999981);
#809=CYLINDRICAL_SURFACE('',#20402,1.04999999999995);
#810=CYLINDRICAL_SURFACE('',#20404,1.39999999999995);
#811=CYLINDRICAL_SURFACE('',#20409,1.04999999999996);
#812=CYLINDRICAL_SURFACE('',#20411,1.05);
#813=CYLINDRICAL_SURFACE('',#20413,1.39999999999978);
#814=CYLINDRICAL_SURFACE('',#20414,2.3640229247478);
#815=CYLINDRICAL_SURFACE('',#20415,0.599999999999987);
#816=CYLINDRICAL_SURFACE('',#20417,0.72500000000001);
#817=CYLINDRICAL_SURFACE('',#20418,2.46743797397101);
#818=CYLINDRICAL_SURFACE('',#20419,0.450000000000123);
#819=CYLINDRICAL_SURFACE('',#20422,1.39999999999995);
#820=CYLINDRICAL_SURFACE('',#20426,1.04999999999995);
#821=CYLINDRICAL_SURFACE('',#20430,1.04999999999981);
#822=CYLINDRICAL_SURFACE('',#20443,1.04999999999996);
#823=CYLINDRICAL_SURFACE('',#20461,1.05);
#824=CYLINDRICAL_SURFACE('',#20464,1.39999999999978);
#825=CYLINDRICAL_SURFACE('',#20466,2.3640229247478);
#826=CYLINDRICAL_SURFACE('',#20468,0.599999999999987);
#827=CYLINDRICAL_SURFACE('',#20471,0.72500000000001);
#828=CYLINDRICAL_SURFACE('',#20473,2.46743797397101);
#829=CYLINDRICAL_SURFACE('',#20475,0.450000000000123);
#830=CYLINDRICAL_SURFACE('',#20480,0.45000000000016);
#831=CYLINDRICAL_SURFACE('',#20482,2.46743797397104);
#832=CYLINDRICAL_SURFACE('',#20484,0.724999999999998);
#833=CYLINDRICAL_SURFACE('',#20487,0.59999999999997);
#834=CYLINDRICAL_SURFACE('',#20489,2.36402292474775);
#835=CYLINDRICAL_SURFACE('',#20511,0.45000000000016);
#836=CYLINDRICAL_SURFACE('',#20513,2.46743797397104);
#837=CYLINDRICAL_SURFACE('',#20515,0.724999999999998);
#838=CYLINDRICAL_SURFACE('',#20518,0.59999999999997);
#839=CYLINDRICAL_SURFACE('',#20520,2.36402292474775);
#840=CYLINDRICAL_SURFACE('',#20522,1.39999999999995);
#841=CYLINDRICAL_SURFACE('',#20525,1.04999999999995);
#842=CYLINDRICAL_SURFACE('',#20528,1.04999999999981);
#843=CYLINDRICAL_SURFACE('',#20538,1.04999999999996);
#844=CYLINDRICAL_SURFACE('',#20546,0.450000000000123);
#845=CYLINDRICAL_SURFACE('',#20548,2.46743797397101);
#846=CYLINDRICAL_SURFACE('',#20550,0.72500000000001);
#847=CYLINDRICAL_SURFACE('',#20553,0.599999999999987);
#848=CYLINDRICAL_SURFACE('',#20555,2.3640229247478);
#849=CYLINDRICAL_SURFACE('',#20557,1.39999999999978);
#850=CYLINDRICAL_SURFACE('',#20560,1.05);
#851=CYLINDRICAL_SURFACE('',#20564,0.45000000000016);
#852=CYLINDRICAL_SURFACE('',#20567,2.46743797397104);
#853=CYLINDRICAL_SURFACE('',#20570,0.724999999999998);
#854=CYLINDRICAL_SURFACE('',#20574,0.59999999999997);
#855=CYLINDRICAL_SURFACE('',#20577,2.36402292474775);
#856=CYLINDRICAL_SURFACE('',#20600,2.16656587073651);
#857=CYLINDRICAL_SURFACE('',#20622,2.16656587073651);
#858=CYLINDRICAL_SURFACE('',#20623,3.00000000000001);
#859=CYLINDRICAL_SURFACE('',#20625,3.00000000000001);
#860=CYLINDRICAL_SURFACE('',#20627,3.00000000000001);
#861=CYLINDRICAL_SURFACE('',#20629,3.00000000000001);
#862=CYLINDRICAL_SURFACE('',#20635,1.04999999999981);
#863=CYLINDRICAL_SURFACE('',#20637,1.04999999999995);
#864=CYLINDRICAL_SURFACE('',#20639,1.39999999999995);
#865=CYLINDRICAL_SURFACE('',#20644,1.04999999999996);
#866=CYLINDRICAL_SURFACE('',#20646,1.05);
#867=CYLINDRICAL_SURFACE('',#20648,1.39999999999978);
#868=CYLINDRICAL_SURFACE('',#20649,2.3640229247478);
#869=CYLINDRICAL_SURFACE('',#20650,0.599999999999987);
#870=CYLINDRICAL_SURFACE('',#20652,0.72500000000001);
#871=CYLINDRICAL_SURFACE('',#20653,2.46743797397101);
#872=CYLINDRICAL_SURFACE('',#20654,0.450000000000123);
#873=CYLINDRICAL_SURFACE('',#20657,1.39999999999995);
#874=CYLINDRICAL_SURFACE('',#20661,1.04999999999995);
#875=CYLINDRICAL_SURFACE('',#20665,1.04999999999981);
#876=CYLINDRICAL_SURFACE('',#20678,1.04999999999996);
#877=CYLINDRICAL_SURFACE('',#20696,1.05);
#878=CYLINDRICAL_SURFACE('',#20699,1.39999999999978);
#879=CYLINDRICAL_SURFACE('',#20701,2.3640229247478);
#880=CYLINDRICAL_SURFACE('',#20703,0.599999999999987);
#881=CYLINDRICAL_SURFACE('',#20706,0.72500000000001);
#882=CYLINDRICAL_SURFACE('',#20708,2.46743797397101);
#883=CYLINDRICAL_SURFACE('',#20710,0.450000000000123);
#884=CYLINDRICAL_SURFACE('',#20715,0.45000000000016);
#885=CYLINDRICAL_SURFACE('',#20717,2.46743797397104);
#886=CYLINDRICAL_SURFACE('',#20719,0.724999999999998);
#887=CYLINDRICAL_SURFACE('',#20722,0.59999999999997);
#888=CYLINDRICAL_SURFACE('',#20724,2.36402292474775);
#889=CYLINDRICAL_SURFACE('',#20728,8.671875);
#890=CYLINDRICAL_SURFACE('',#20880,5.);
#891=CYLINDRICAL_SURFACE('',#20895,8.4375);
#892=CYLINDRICAL_SURFACE('',#20896,8.4375);
#893=CYLINDRICAL_SURFACE('',#20903,17.5);
#894=CYLINDRICAL_SURFACE('',#20917,15.625);
#895=CYLINDRICAL_SURFACE('',#20919,15.625);
#896=CYLINDRICAL_SURFACE('',#20943,8.671875);
#897=CYLINDRICAL_SURFACE('',#21114,3.25);
#898=CYLINDRICAL_SURFACE('',#21125,0.499999999999999);
#899=CYLINDRICAL_SURFACE('',#21129,0.499999999999998);
#900=CYLINDRICAL_SURFACE('',#21143,0.499999999999998);
#901=CYLINDRICAL_SURFACE('',#21147,0.499999999999999);
#902=CYLINDRICAL_SURFACE('',#21159,2.);
#903=CYLINDRICAL_SURFACE('',#21170,0.499999999999999);
#904=CYLINDRICAL_SURFACE('',#21174,0.499999999999998);
#905=CYLINDRICAL_SURFACE('',#21189,3.25);
#906=CYLINDRICAL_SURFACE('',#21193,0.499999999999998);
#907=CYLINDRICAL_SURFACE('',#21197,0.499999999999999);
#908=CYLINDRICAL_SURFACE('',#21209,2.);
#909=CYLINDRICAL_SURFACE('',#21255,3.25);
#910=CYLINDRICAL_SURFACE('',#21302,3.25);
#911=CYLINDRICAL_SURFACE('',#21314,0.499999999999999);
#912=CYLINDRICAL_SURFACE('',#21318,0.499999999999998);
#913=CYLINDRICAL_SURFACE('',#21332,0.499999999999998);
#914=CYLINDRICAL_SURFACE('',#21336,0.499999999999999);
#915=CYLINDRICAL_SURFACE('',#21348,2.);
#916=CYLINDRICAL_SURFACE('',#21366,0.499999999999999);
#917=CYLINDRICAL_SURFACE('',#21369,0.499999999999998);
#918=CYLINDRICAL_SURFACE('',#21383,3.25);
#919=CYLINDRICAL_SURFACE('',#21386,0.499999999999998);
#920=CYLINDRICAL_SURFACE('',#21389,0.499999999999999);
#921=CYLINDRICAL_SURFACE('',#21400,2.);
#922=CYLINDRICAL_SURFACE('',#21411,7.925);
#923=CYLINDRICAL_SURFACE('',#21413,7.925);
#924=CYLINDRICAL_SURFACE('',#21414,7.925);
#925=CYLINDRICAL_SURFACE('',#21415,7.925);
#926=CYLINDRICAL_SURFACE('',#21416,7.925);
#927=CYLINDRICAL_SURFACE('',#21417,7.925);
#928=CYLINDRICAL_SURFACE('',#21418,7.925);
#929=CYLINDRICAL_SURFACE('',#21419,7.925);
#930=CYLINDRICAL_SURFACE('',#21420,7.925);
#931=CYLINDRICAL_SURFACE('',#21421,7.925);
#932=CYLINDRICAL_SURFACE('',#21422,7.925);
#933=CYLINDRICAL_SURFACE('',#21423,7.925);
#934=CYLINDRICAL_SURFACE('',#21424,7.925);
#935=CYLINDRICAL_SURFACE('',#21425,7.925);
#936=CYLINDRICAL_SURFACE('',#21426,7.925);
#937=CYLINDRICAL_SURFACE('',#21427,7.925);
#938=CYLINDRICAL_SURFACE('',#21428,7.925);
#939=CYLINDRICAL_SURFACE('',#21429,7.925);
#940=CYLINDRICAL_SURFACE('',#21430,7.925);
#941=CYLINDRICAL_SURFACE('',#21431,7.925);
#942=CYLINDRICAL_SURFACE('',#21432,7.925);
#943=CYLINDRICAL_SURFACE('',#21433,7.925);
#944=CYLINDRICAL_SURFACE('',#21434,7.925);
#945=CYLINDRICAL_SURFACE('',#21435,7.925);
#946=CYLINDRICAL_SURFACE('',#21436,7.925);
#947=CYLINDRICAL_SURFACE('',#21437,7.925);
#948=CYLINDRICAL_SURFACE('',#21438,7.925);
#949=CYLINDRICAL_SURFACE('',#21439,7.925);
#950=CYLINDRICAL_SURFACE('',#21440,7.925);
#951=CYLINDRICAL_SURFACE('',#21441,7.925);
#952=CYLINDRICAL_SURFACE('',#21442,7.925);
#953=CYLINDRICAL_SURFACE('',#21443,7.925);
#954=CYLINDRICAL_SURFACE('',#21444,7.925);
#955=CYLINDRICAL_SURFACE('',#21445,7.925);
#956=CYLINDRICAL_SURFACE('',#21446,7.925);
#957=CYLINDRICAL_SURFACE('',#21447,7.925);
#958=CYLINDRICAL_SURFACE('',#21448,7.925);
#959=CYLINDRICAL_SURFACE('',#21449,7.925);
#960=CYLINDRICAL_SURFACE('',#21450,7.925);
#961=CYLINDRICAL_SURFACE('',#21451,7.925);
#962=CYLINDRICAL_SURFACE('',#21452,7.925);
#963=CYLINDRICAL_SURFACE('',#21453,7.925);
#964=CYLINDRICAL_SURFACE('',#21454,7.925);
#965=CYLINDRICAL_SURFACE('',#21455,7.925);
#966=CYLINDRICAL_SURFACE('',#21456,7.925);
#967=CYLINDRICAL_SURFACE('',#21457,7.925);
#968=CYLINDRICAL_SURFACE('',#21458,7.925);
#969=CYLINDRICAL_SURFACE('',#21459,7.925);
#970=CYLINDRICAL_SURFACE('',#21460,7.925);
#971=CYLINDRICAL_SURFACE('',#21461,7.925);
#972=CYLINDRICAL_SURFACE('',#21462,7.925);
#973=CYLINDRICAL_SURFACE('',#21463,7.925);
#974=CYLINDRICAL_SURFACE('',#21464,7.925);
#975=CYLINDRICAL_SURFACE('',#21465,7.925);
#976=CYLINDRICAL_SURFACE('',#21466,7.925);
#977=CYLINDRICAL_SURFACE('',#21467,7.925);
#978=CYLINDRICAL_SURFACE('',#21468,7.925);
#979=CYLINDRICAL_SURFACE('',#21469,7.925);
#980=CYLINDRICAL_SURFACE('',#21470,7.925);
#981=CYLINDRICAL_SURFACE('',#21471,7.925);
#982=CYLINDRICAL_SURFACE('',#21472,7.925);
#983=CYLINDRICAL_SURFACE('',#21473,7.925);
#984=CYLINDRICAL_SURFACE('',#21474,7.925);
#985=CYLINDRICAL_SURFACE('',#21475,7.925);
#986=CYLINDRICAL_SURFACE('',#21476,7.925);
#987=CYLINDRICAL_SURFACE('',#21477,7.925);
#988=CYLINDRICAL_SURFACE('',#21478,7.925);
#989=CYLINDRICAL_SURFACE('',#21479,7.925);
#990=CYLINDRICAL_SURFACE('',#21480,7.925);
#991=CYLINDRICAL_SURFACE('',#21481,7.925);
#992=CYLINDRICAL_SURFACE('',#21482,7.925);
#993=CYLINDRICAL_SURFACE('',#21483,7.925);
#994=CYLINDRICAL_SURFACE('',#21484,7.925);
#995=CYLINDRICAL_SURFACE('',#21485,7.925);
#996=CYLINDRICAL_SURFACE('',#21486,7.925);
#997=CYLINDRICAL_SURFACE('',#21487,7.925);
#998=CYLINDRICAL_SURFACE('',#21488,7.925);
#999=CYLINDRICAL_SURFACE('',#21489,7.925);
#1000=CYLINDRICAL_SURFACE('',#21490,7.925);
#1001=CYLINDRICAL_SURFACE('',#21491,7.925);
#1002=CYLINDRICAL_SURFACE('',#21492,7.925);
#1003=CYLINDRICAL_SURFACE('',#21493,7.925);
#1004=CYLINDRICAL_SURFACE('',#21494,7.925);
#1005=CYLINDRICAL_SURFACE('',#21495,7.925);
#1006=CYLINDRICAL_SURFACE('',#21496,7.925);
#1007=CYLINDRICAL_SURFACE('',#21497,7.925);
#1008=CYLINDRICAL_SURFACE('',#21498,7.925);
#1009=CYLINDRICAL_SURFACE('',#21499,7.925);
#1010=CYLINDRICAL_SURFACE('',#21500,7.925);
#1011=CYLINDRICAL_SURFACE('',#21501,7.925);
#1012=CYLINDRICAL_SURFACE('',#21502,7.925);
#1013=CYLINDRICAL_SURFACE('',#21503,7.925);
#1014=CYLINDRICAL_SURFACE('',#21504,7.925);
#1015=CYLINDRICAL_SURFACE('',#21505,7.925);
#1016=CYLINDRICAL_SURFACE('',#21506,7.925);
#1017=CYLINDRICAL_SURFACE('',#21507,7.925);
#1018=CYLINDRICAL_SURFACE('',#21508,7.925);
#1019=CYLINDRICAL_SURFACE('',#21509,7.925);
#1020=CYLINDRICAL_SURFACE('',#21510,7.925);
#1021=CYLINDRICAL_SURFACE('',#21511,7.925);
#1022=CYLINDRICAL_SURFACE('',#21512,7.925);
#1023=CYLINDRICAL_SURFACE('',#21514,4.81675);
#1024=CYLINDRICAL_SURFACE('',#21517,4.81675);
#1025=CYLINDRICAL_SURFACE('',#21518,4.81675);
#1026=CYLINDRICAL_SURFACE('',#21519,4.81675);
#1027=CYLINDRICAL_SURFACE('',#21520,4.81675);
#1028=CYLINDRICAL_SURFACE('',#21521,4.81675);
#1029=CYLINDRICAL_SURFACE('',#21522,4.81675);
#1030=CYLINDRICAL_SURFACE('',#21523,4.81675);
#1031=CYLINDRICAL_SURFACE('',#21524,4.81675);
#1032=CYLINDRICAL_SURFACE('',#21525,4.81675);
#1033=CYLINDRICAL_SURFACE('',#21527,4.91825);
#1034=CYLINDRICAL_SURFACE('',#21529,4.91825);
#1035=CYLINDRICAL_SURFACE('',#21530,4.91825);
#1036=CYLINDRICAL_SURFACE('',#21531,4.91825);
#1037=CYLINDRICAL_SURFACE('',#21532,4.91825);
#1038=CYLINDRICAL_SURFACE('',#21533,4.91825);
#1039=CYLINDRICAL_SURFACE('',#21534,4.91825);
#1040=CYLINDRICAL_SURFACE('',#21535,4.91825);
#1041=CYLINDRICAL_SURFACE('',#21536,4.91825);
#1042=CYLINDRICAL_SURFACE('',#21537,4.91825);
#1043=CYLINDRICAL_SURFACE('',#21538,5.6435);
#1044=CYLINDRICAL_SURFACE('',#21540,5.6435);
#1045=CYLINDRICAL_SURFACE('',#21541,5.6435);
#1046=CYLINDRICAL_SURFACE('',#21542,5.6435);
#1047=CYLINDRICAL_SURFACE('',#21543,5.6435);
#1048=CYLINDRICAL_SURFACE('',#21544,5.6435);
#1049=CYLINDRICAL_SURFACE('',#21545,5.6435);
#1050=CYLINDRICAL_SURFACE('',#21546,5.6435);
#1051=CYLINDRICAL_SURFACE('',#21547,5.6435);
#1052=CYLINDRICAL_SURFACE('',#21548,5.6435);
#1053=CYLINDRICAL_SURFACE('',#21549,5.6435);
#1054=CYLINDRICAL_SURFACE('',#21550,5.6435);
#1055=CYLINDRICAL_SURFACE('',#21551,5.6435);
#1056=CYLINDRICAL_SURFACE('',#21552,5.6435);
#1057=CYLINDRICAL_SURFACE('',#21553,5.6435);
#1058=CYLINDRICAL_SURFACE('',#21554,5.6435);
#1059=CYLINDRICAL_SURFACE('',#21555,5.6435);
#1060=CYLINDRICAL_SURFACE('',#21556,5.6435);
#1061=CYLINDRICAL_SURFACE('',#21557,5.6435);
#1062=CYLINDRICAL_SURFACE('',#21558,5.6435);
#1063=CYLINDRICAL_SURFACE('',#21559,5.6435);
#1064=CYLINDRICAL_SURFACE('',#21560,5.6435);
#1065=CYLINDRICAL_SURFACE('',#21561,5.6435);
#1066=CYLINDRICAL_SURFACE('',#21562,5.6435);
#1067=CYLINDRICAL_SURFACE('',#21563,5.6435);
#1068=CYLINDRICAL_SURFACE('',#21564,5.6435);
#1069=CYLINDRICAL_SURFACE('',#21565,5.6435);
#1070=CYLINDRICAL_SURFACE('',#21566,5.6435);
#1071=CYLINDRICAL_SURFACE('',#21567,5.6435);
#1072=CYLINDRICAL_SURFACE('',#21568,5.6435);
#1073=CYLINDRICAL_SURFACE('',#21569,5.6435);
#1074=CYLINDRICAL_SURFACE('',#21570,5.6435);
#1075=CYLINDRICAL_SURFACE('',#21571,5.6435);
#1076=CYLINDRICAL_SURFACE('',#21572,5.6435);
#1077=CYLINDRICAL_SURFACE('',#21573,5.6435);
#1078=CYLINDRICAL_SURFACE('',#21574,5.6435);
#1079=CYLINDRICAL_SURFACE('',#21575,5.6435);
#1080=CYLINDRICAL_SURFACE('',#21576,5.6435);
#1081=CYLINDRICAL_SURFACE('',#21577,5.6435);
#1082=CYLINDRICAL_SURFACE('',#21578,5.6435);
#1083=CYLINDRICAL_SURFACE('',#21579,5.6435);
#1084=CYLINDRICAL_SURFACE('',#21580,5.6435);
#1085=CYLINDRICAL_SURFACE('',#21581,5.6435);
#1086=CYLINDRICAL_SURFACE('',#21582,5.6435);
#1087=CYLINDRICAL_SURFACE('',#21583,5.6435);
#1088=CYLINDRICAL_SURFACE('',#21584,5.6435);
#1089=CYLINDRICAL_SURFACE('',#21585,5.6435);
#1090=CYLINDRICAL_SURFACE('',#21586,5.6435);
#1091=CYLINDRICAL_SURFACE('',#21587,5.6435);
#1092=CYLINDRICAL_SURFACE('',#21588,5.6435);
#1093=CYLINDRICAL_SURFACE('',#21589,5.6435);
#1094=CYLINDRICAL_SURFACE('',#21590,5.6435);
#1095=CYLINDRICAL_SURFACE('',#21591,5.6435);
#1096=CYLINDRICAL_SURFACE('',#21592,5.6435);
#1097=CYLINDRICAL_SURFACE('',#21593,5.6435);
#1098=CYLINDRICAL_SURFACE('',#21594,5.6435);
#1099=CYLINDRICAL_SURFACE('',#21595,5.6435);
#1100=CYLINDRICAL_SURFACE('',#21596,5.6435);
#1101=CYLINDRICAL_SURFACE('',#21597,5.6435);
#1102=CYLINDRICAL_SURFACE('',#21598,5.6435);
#1103=CYLINDRICAL_SURFACE('',#21599,5.6435);
#1104=CYLINDRICAL_SURFACE('',#21600,5.6435);
#1105=CYLINDRICAL_SURFACE('',#21601,5.6435);
#1106=CYLINDRICAL_SURFACE('',#21602,5.6435);
#1107=CYLINDRICAL_SURFACE('',#21603,5.6435);
#1108=CYLINDRICAL_SURFACE('',#21604,5.6435);
#1109=CYLINDRICAL_SURFACE('',#21605,5.6435);
#1110=CYLINDRICAL_SURFACE('',#21606,5.6435);
#1111=CYLINDRICAL_SURFACE('',#21607,5.6435);
#1112=CYLINDRICAL_SURFACE('',#21608,5.6435);
#1113=CYLINDRICAL_SURFACE('',#21609,5.6435);
#1114=CYLINDRICAL_SURFACE('',#21610,5.6435);
#1115=CYLINDRICAL_SURFACE('',#21611,5.6435);
#1116=CYLINDRICAL_SURFACE('',#21612,5.6435);
#1117=CYLINDRICAL_SURFACE('',#21613,5.6435);
#1118=CYLINDRICAL_SURFACE('',#21614,5.6435);
#1119=CYLINDRICAL_SURFACE('',#21615,5.6435);
#1120=CYLINDRICAL_SURFACE('',#21616,5.6435);
#1121=CYLINDRICAL_SURFACE('',#21617,5.6435);
#1122=CYLINDRICAL_SURFACE('',#21618,5.6435);
#1123=CYLINDRICAL_SURFACE('',#21619,5.6435);
#1124=CYLINDRICAL_SURFACE('',#21620,5.6435);
#1125=CYLINDRICAL_SURFACE('',#21621,5.6435);
#1126=CYLINDRICAL_SURFACE('',#21622,5.6435);
#1127=CYLINDRICAL_SURFACE('',#21623,5.6435);
#1128=CYLINDRICAL_SURFACE('',#21624,5.6435);
#1129=CYLINDRICAL_SURFACE('',#21625,5.6435);
#1130=CYLINDRICAL_SURFACE('',#21626,5.6435);
#1131=CYLINDRICAL_SURFACE('',#21627,5.6435);
#1132=CYLINDRICAL_SURFACE('',#21628,5.6435);
#1133=CYLINDRICAL_SURFACE('',#21629,5.6435);
#1134=CYLINDRICAL_SURFACE('',#21630,5.6435);
#1135=CYLINDRICAL_SURFACE('',#21631,5.6435);
#1136=CYLINDRICAL_SURFACE('',#21632,5.6435);
#1137=CYLINDRICAL_SURFACE('',#21633,5.6435);
#1138=CYLINDRICAL_SURFACE('',#21634,5.6435);
#1139=CYLINDRICAL_SURFACE('',#21635,5.6435);
#1140=CYLINDRICAL_SURFACE('',#21636,5.6435);
#1141=CYLINDRICAL_SURFACE('',#21637,5.6435);
#1142=CYLINDRICAL_SURFACE('',#21638,5.6435);
#1143=CYLINDRICAL_SURFACE('',#21642,5.00000000000001);
#1144=CYLINDRICAL_SURFACE('',#21648,5.);
#1145=CYLINDRICAL_SURFACE('',#21653,5.6435);
#1146=CYLINDRICAL_SURFACE('',#21659,4.91825);
#1147=CYLINDRICAL_SURFACE('',#21660,4.81675);
#1148=CYLINDRICAL_SURFACE('',#21662,7.925);
#1149=CYLINDRICAL_SURFACE('',#21668,3.00000000000001);
#1150=CYLINDRICAL_SURFACE('',#21671,3.00000000000001);
#1151=CYLINDRICAL_SURFACE('',#21674,3.);
#1152=CYLINDRICAL_SURFACE('',#21677,3.);
#1153=CYLINDRICAL_SURFACE('',#21680,3.);
#1154=CYLINDRICAL_SURFACE('',#21683,3.);
#1155=CYLINDRICAL_SURFACE('',#21686,3.00000000000001);
#1156=CYLINDRICAL_SURFACE('',#21689,3.00000000000001);
#1157=CYLINDRICAL_SURFACE('',#21692,3.00000000000001);
#1158=CYLINDRICAL_SURFACE('',#21695,3.00000000000001);
#1159=CYLINDRICAL_SURFACE('',#21698,3.);
#1160=CYLINDRICAL_SURFACE('',#21701,3.);
#1161=CYLINDRICAL_SURFACE('',#21704,3.);
#1162=CYLINDRICAL_SURFACE('',#21707,3.);
#1163=CYLINDRICAL_SURFACE('',#21710,3.00000000000001);
#1164=CYLINDRICAL_SURFACE('',#21713,3.00000000000001);
#1165=CYLINDRICAL_SURFACE('',#21716,8.09375);
#1166=CYLINDRICAL_SURFACE('',#21718,5.);
#1167=CYLINDRICAL_SURFACE('',#21721,5.);
#1168=CYLINDRICAL_SURFACE('',#21738,0.450000000000145);
#1169=CYLINDRICAL_SURFACE('',#21741,2.46743797397102);
#1170=CYLINDRICAL_SURFACE('',#21744,0.725000000000007);
#1171=CYLINDRICAL_SURFACE('',#21748,0.599999999999981);
#1172=CYLINDRICAL_SURFACE('',#21751,2.3640229247478);
#1173=CYLINDRICAL_SURFACE('',#21754,1.39999999999995);
#1174=CYLINDRICAL_SURFACE('',#21758,1.05000000000001);
#1175=CYLINDRICAL_SURFACE('',#21762,1.04999999999996);
#1176=CYLINDRICAL_SURFACE('',#21766,1.09999999999999);
#1177=CYLINDRICAL_SURFACE('',#21782,0.450000000000145);
#1178=CYLINDRICAL_SURFACE('',#21784,2.46743797397102);
#1179=CYLINDRICAL_SURFACE('',#21786,0.725000000000007);
#1180=CYLINDRICAL_SURFACE('',#21789,0.599999999999981);
#1181=CYLINDRICAL_SURFACE('',#21791,2.3640229247478);
#1182=CYLINDRICAL_SURFACE('',#21793,1.39999999999995);
#1183=CYLINDRICAL_SURFACE('',#21796,1.05000000000001);
#1184=CYLINDRICAL_SURFACE('',#21799,1.04999999999996);
#1185=CYLINDRICAL_SURFACE('',#21802,1.09999999999999);
#1186=CYLINDRICAL_SURFACE('',#21810,17.5);
#1187=CYLINDRICAL_SURFACE('',#21820,5.);
#1188=CYLINDRICAL_SURFACE('',#21830,17.5);
#1189=CYLINDRICAL_SURFACE('',#21841,0.450000000000145);
#1190=CYLINDRICAL_SURFACE('',#21844,2.46743797397102);
#1191=CYLINDRICAL_SURFACE('',#21847,0.725000000000007);
#1192=CYLINDRICAL_SURFACE('',#21851,0.599999999999981);
#1193=CYLINDRICAL_SURFACE('',#21854,2.3640229247478);
#1194=CYLINDRICAL_SURFACE('',#21857,1.39999999999995);
#1195=CYLINDRICAL_SURFACE('',#21861,1.05000000000001);
#1196=CYLINDRICAL_SURFACE('',#21865,1.04999999999996);
#1197=CYLINDRICAL_SURFACE('',#21869,1.09999999999999);
#1198=CYLINDRICAL_SURFACE('',#21885,0.450000000000145);
#1199=CYLINDRICAL_SURFACE('',#21887,2.46743797397102);
#1200=CYLINDRICAL_SURFACE('',#21889,0.725000000000007);
#1201=CYLINDRICAL_SURFACE('',#21892,0.599999999999981);
#1202=CYLINDRICAL_SURFACE('',#21894,2.3640229247478);
#1203=CYLINDRICAL_SURFACE('',#21896,1.39999999999995);
#1204=CYLINDRICAL_SURFACE('',#21899,1.05000000000001);
#1205=CYLINDRICAL_SURFACE('',#21902,1.04999999999996);
#1206=CYLINDRICAL_SURFACE('',#21905,1.09999999999999);
#1207=FACE_OUTER_BOUND('',#2251,.T.);
#1208=FACE_OUTER_BOUND('',#2252,.T.);
#1209=FACE_OUTER_BOUND('',#2253,.T.);
#1210=FACE_OUTER_BOUND('',#2254,.T.);
#1211=FACE_OUTER_BOUND('',#2255,.T.);
#1212=FACE_OUTER_BOUND('',#2256,.T.);
#1213=FACE_OUTER_BOUND('',#2257,.T.);
#1214=FACE_OUTER_BOUND('',#2258,.T.);
#1215=FACE_OUTER_BOUND('',#2259,.T.);
#1216=FACE_OUTER_BOUND('',#2260,.T.);
#1217=FACE_OUTER_BOUND('',#2261,.T.);
#1218=FACE_OUTER_BOUND('',#2262,.T.);
#1219=FACE_OUTER_BOUND('',#2263,.T.);
#1220=FACE_OUTER_BOUND('',#2264,.T.);
#1221=FACE_OUTER_BOUND('',#2265,.T.);
#1222=FACE_OUTER_BOUND('',#2266,.T.);
#1223=FACE_OUTER_BOUND('',#2267,.T.);
#1224=FACE_OUTER_BOUND('',#2268,.T.);
#1225=FACE_OUTER_BOUND('',#2269,.T.);
#1226=FACE_OUTER_BOUND('',#2270,.T.);
#1227=FACE_OUTER_BOUND('',#2271,.T.);
#1228=FACE_OUTER_BOUND('',#2272,.T.);
#1229=FACE_OUTER_BOUND('',#2273,.T.);
#1230=FACE_OUTER_BOUND('',#2274,.T.);
#1231=FACE_OUTER_BOUND('',#2275,.T.);
#1232=FACE_OUTER_BOUND('',#2276,.T.);
#1233=FACE_OUTER_BOUND('',#2277,.T.);
#1234=FACE_OUTER_BOUND('',#2278,.T.);
#1235=FACE_OUTER_BOUND('',#2279,.T.);
#1236=FACE_OUTER_BOUND('',#2280,.T.);
#1237=FACE_OUTER_BOUND('',#2281,.T.);
#1238=FACE_OUTER_BOUND('',#2282,.T.);
#1239=FACE_OUTER_BOUND('',#2283,.T.);
#1240=FACE_OUTER_BOUND('',#2284,.T.);
#1241=FACE_OUTER_BOUND('',#2285,.T.);
#1242=FACE_OUTER_BOUND('',#2286,.T.);
#1243=FACE_OUTER_BOUND('',#2287,.T.);
#1244=FACE_OUTER_BOUND('',#2288,.T.);
#1245=FACE_OUTER_BOUND('',#2289,.T.);
#1246=FACE_OUTER_BOUND('',#2290,.T.);
#1247=FACE_OUTER_BOUND('',#2291,.T.);
#1248=FACE_OUTER_BOUND('',#2292,.T.);
#1249=FACE_OUTER_BOUND('',#2293,.T.);
#1250=FACE_OUTER_BOUND('',#2294,.T.);
#1251=FACE_OUTER_BOUND('',#2295,.T.);
#1252=FACE_OUTER_BOUND('',#2296,.T.);
#1253=FACE_OUTER_BOUND('',#2297,.T.);
#1254=FACE_OUTER_BOUND('',#2298,.T.);
#1255=FACE_OUTER_BOUND('',#2299,.T.);
#1256=FACE_OUTER_BOUND('',#2300,.T.);
#1257=FACE_OUTER_BOUND('',#2303,.T.);
#1258=FACE_OUTER_BOUND('',#2304,.T.);
#1259=FACE_OUTER_BOUND('',#2305,.T.);
#1260=FACE_OUTER_BOUND('',#2306,.T.);
#1261=FACE_OUTER_BOUND('',#2307,.T.);
#1262=FACE_OUTER_BOUND('',#2308,.T.);
#1263=FACE_OUTER_BOUND('',#2309,.T.);
#1264=FACE_OUTER_BOUND('',#2312,.T.);
#1265=FACE_OUTER_BOUND('',#2313,.T.);
#1266=FACE_OUTER_BOUND('',#2314,.T.);
#1267=FACE_OUTER_BOUND('',#2315,.T.);
#1268=FACE_OUTER_BOUND('',#2316,.T.);
#1269=FACE_OUTER_BOUND('',#2317,.T.);
#1270=FACE_OUTER_BOUND('',#2318,.T.);
#1271=FACE_OUTER_BOUND('',#2319,.T.);
#1272=FACE_OUTER_BOUND('',#2322,.T.);
#1273=FACE_OUTER_BOUND('',#2323,.T.);
#1274=FACE_OUTER_BOUND('',#2324,.T.);
#1275=FACE_OUTER_BOUND('',#2325,.T.);
#1276=FACE_OUTER_BOUND('',#2326,.T.);
#1277=FACE_OUTER_BOUND('',#2327,.T.);
#1278=FACE_OUTER_BOUND('',#2328,.T.);
#1279=FACE_OUTER_BOUND('',#2329,.T.);
#1280=FACE_OUTER_BOUND('',#2330,.T.);
#1281=FACE_OUTER_BOUND('',#2333,.T.);
#1282=FACE_OUTER_BOUND('',#2334,.T.);
#1283=FACE_OUTER_BOUND('',#2335,.T.);
#1284=FACE_OUTER_BOUND('',#2336,.T.);
#1285=FACE_OUTER_BOUND('',#2337,.T.);
#1286=FACE_OUTER_BOUND('',#2338,.T.);
#1287=FACE_OUTER_BOUND('',#2339,.T.);
#1288=FACE_OUTER_BOUND('',#2340,.T.);
#1289=FACE_OUTER_BOUND('',#2341,.T.);
#1290=FACE_OUTER_BOUND('',#2342,.T.);
#1291=FACE_OUTER_BOUND('',#2343,.T.);
#1292=FACE_OUTER_BOUND('',#2344,.T.);
#1293=FACE_OUTER_BOUND('',#2345,.T.);
#1294=FACE_OUTER_BOUND('',#2346,.T.);
#1295=FACE_OUTER_BOUND('',#2347,.T.);
#1296=FACE_OUTER_BOUND('',#2348,.T.);
#1297=FACE_OUTER_BOUND('',#2349,.T.);
#1298=FACE_OUTER_BOUND('',#2350,.T.);
#1299=FACE_OUTER_BOUND('',#2351,.T.);
#1300=FACE_OUTER_BOUND('',#2352,.T.);
#1301=FACE_OUTER_BOUND('',#2353,.T.);
#1302=FACE_OUTER_BOUND('',#2354,.T.);
#1303=FACE_OUTER_BOUND('',#2355,.T.);
#1304=FACE_OUTER_BOUND('',#2356,.T.);
#1305=FACE_OUTER_BOUND('',#2357,.T.);
#1306=FACE_OUTER_BOUND('',#2358,.T.);
#1307=FACE_OUTER_BOUND('',#2359,.T.);
#1308=FACE_OUTER_BOUND('',#2360,.T.);
#1309=FACE_OUTER_BOUND('',#2361,.T.);
#1310=FACE_OUTER_BOUND('',#2362,.T.);
#1311=FACE_OUTER_BOUND('',#2363,.T.);
#1312=FACE_OUTER_BOUND('',#2364,.T.);
#1313=FACE_OUTER_BOUND('',#2365,.T.);
#1314=FACE_OUTER_BOUND('',#2366,.T.);
#1315=FACE_OUTER_BOUND('',#2367,.T.);
#1316=FACE_OUTER_BOUND('',#2368,.T.);
#1317=FACE_OUTER_BOUND('',#2369,.T.);
#1318=FACE_OUTER_BOUND('',#2370,.T.);
#1319=FACE_OUTER_BOUND('',#2371,.T.);
#1320=FACE_OUTER_BOUND('',#2372,.T.);
#1321=FACE_OUTER_BOUND('',#2373,.T.);
#1322=FACE_OUTER_BOUND('',#2374,.T.);
#1323=FACE_OUTER_BOUND('',#2375,.T.);
#1324=FACE_OUTER_BOUND('',#2376,.T.);
#1325=FACE_OUTER_BOUND('',#2377,.T.);
#1326=FACE_OUTER_BOUND('',#2378,.T.);
#1327=FACE_OUTER_BOUND('',#2379,.T.);
#1328=FACE_OUTER_BOUND('',#2380,.T.);
#1329=FACE_OUTER_BOUND('',#2381,.T.);
#1330=FACE_OUTER_BOUND('',#2382,.T.);
#1331=FACE_OUTER_BOUND('',#2383,.T.);
#1332=FACE_OUTER_BOUND('',#2384,.T.);
#1333=FACE_OUTER_BOUND('',#2385,.T.);
#1334=FACE_OUTER_BOUND('',#2386,.T.);
#1335=FACE_OUTER_BOUND('',#2387,.T.);
#1336=FACE_OUTER_BOUND('',#2388,.T.);
#1337=FACE_OUTER_BOUND('',#2389,.T.);
#1338=FACE_OUTER_BOUND('',#2390,.T.);
#1339=FACE_OUTER_BOUND('',#2391,.T.);
#1340=FACE_OUTER_BOUND('',#2392,.T.);
#1341=FACE_OUTER_BOUND('',#2393,.T.);
#1342=FACE_OUTER_BOUND('',#2394,.T.);
#1343=FACE_OUTER_BOUND('',#2395,.T.);
#1344=FACE_OUTER_BOUND('',#2396,.T.);
#1345=FACE_OUTER_BOUND('',#2397,.T.);
#1346=FACE_OUTER_BOUND('',#2398,.T.);
#1347=FACE_OUTER_BOUND('',#2399,.T.);
#1348=FACE_OUTER_BOUND('',#2400,.T.);
#1349=FACE_OUTER_BOUND('',#2401,.T.);
#1350=FACE_OUTER_BOUND('',#2402,.T.);
#1351=FACE_OUTER_BOUND('',#2403,.T.);
#1352=FACE_OUTER_BOUND('',#2404,.T.);
#1353=FACE_OUTER_BOUND('',#2405,.T.);
#1354=FACE_OUTER_BOUND('',#2406,.T.);
#1355=FACE_OUTER_BOUND('',#2407,.T.);
#1356=FACE_OUTER_BOUND('',#2408,.T.);
#1357=FACE_OUTER_BOUND('',#2409,.T.);
#1358=FACE_OUTER_BOUND('',#2410,.T.);
#1359=FACE_OUTER_BOUND('',#2411,.T.);
#1360=FACE_OUTER_BOUND('',#2412,.T.);
#1361=FACE_OUTER_BOUND('',#2413,.T.);
#1362=FACE_OUTER_BOUND('',#2414,.T.);
#1363=FACE_OUTER_BOUND('',#2415,.T.);
#1364=FACE_OUTER_BOUND('',#2416,.T.);
#1365=FACE_OUTER_BOUND('',#2417,.T.);
#1366=FACE_OUTER_BOUND('',#2418,.T.);
#1367=FACE_OUTER_BOUND('',#2419,.T.);
#1368=FACE_OUTER_BOUND('',#2420,.T.);
#1369=FACE_OUTER_BOUND('',#2421,.T.);
#1370=FACE_OUTER_BOUND('',#2422,.T.);
#1371=FACE_OUTER_BOUND('',#2423,.T.);
#1372=FACE_OUTER_BOUND('',#2424,.T.);
#1373=FACE_OUTER_BOUND('',#2425,.T.);
#1374=FACE_OUTER_BOUND('',#2426,.T.);
#1375=FACE_OUTER_BOUND('',#2427,.T.);
#1376=FACE_OUTER_BOUND('',#2428,.T.);
#1377=FACE_OUTER_BOUND('',#2429,.T.);
#1378=FACE_OUTER_BOUND('',#2430,.T.);
#1379=FACE_OUTER_BOUND('',#2431,.T.);
#1380=FACE_OUTER_BOUND('',#2432,.T.);
#1381=FACE_OUTER_BOUND('',#2433,.T.);
#1382=FACE_OUTER_BOUND('',#2434,.T.);
#1383=FACE_OUTER_BOUND('',#2437,.T.);
#1384=FACE_OUTER_BOUND('',#2438,.T.);
#1385=FACE_OUTER_BOUND('',#2439,.T.);
#1386=FACE_OUTER_BOUND('',#2440,.T.);
#1387=FACE_OUTER_BOUND('',#2441,.T.);
#1388=FACE_OUTER_BOUND('',#2442,.T.);
#1389=FACE_OUTER_BOUND('',#2443,.T.);
#1390=FACE_OUTER_BOUND('',#2446,.T.);
#1391=FACE_OUTER_BOUND('',#2447,.T.);
#1392=FACE_OUTER_BOUND('',#2448,.T.);
#1393=FACE_OUTER_BOUND('',#2449,.T.);
#1394=FACE_OUTER_BOUND('',#2450,.T.);
#1395=FACE_OUTER_BOUND('',#2451,.T.);
#1396=FACE_OUTER_BOUND('',#2452,.T.);
#1397=FACE_OUTER_BOUND('',#2453,.T.);
#1398=FACE_OUTER_BOUND('',#2456,.T.);
#1399=FACE_OUTER_BOUND('',#2457,.T.);
#1400=FACE_OUTER_BOUND('',#2458,.T.);
#1401=FACE_OUTER_BOUND('',#2459,.T.);
#1402=FACE_OUTER_BOUND('',#2460,.T.);
#1403=FACE_OUTER_BOUND('',#2461,.T.);
#1404=FACE_OUTER_BOUND('',#2462,.T.);
#1405=FACE_OUTER_BOUND('',#2463,.T.);
#1406=FACE_OUTER_BOUND('',#2464,.T.);
#1407=FACE_OUTER_BOUND('',#2467,.T.);
#1408=FACE_OUTER_BOUND('',#2468,.T.);
#1409=FACE_OUTER_BOUND('',#2469,.T.);
#1410=FACE_OUTER_BOUND('',#2470,.T.);
#1411=FACE_OUTER_BOUND('',#2471,.T.);
#1412=FACE_OUTER_BOUND('',#2472,.T.);
#1413=FACE_OUTER_BOUND('',#2473,.T.);
#1414=FACE_OUTER_BOUND('',#2474,.T.);
#1415=FACE_OUTER_BOUND('',#2475,.T.);
#1416=FACE_OUTER_BOUND('',#2476,.T.);
#1417=FACE_OUTER_BOUND('',#2477,.T.);
#1418=FACE_OUTER_BOUND('',#2478,.T.);
#1419=FACE_OUTER_BOUND('',#2479,.T.);
#1420=FACE_OUTER_BOUND('',#2480,.T.);
#1421=FACE_OUTER_BOUND('',#2481,.T.);
#1422=FACE_OUTER_BOUND('',#2482,.T.);
#1423=FACE_OUTER_BOUND('',#2483,.T.);
#1424=FACE_OUTER_BOUND('',#2484,.T.);
#1425=FACE_OUTER_BOUND('',#2485,.T.);
#1426=FACE_OUTER_BOUND('',#2486,.T.);
#1427=FACE_OUTER_BOUND('',#2487,.T.);
#1428=FACE_OUTER_BOUND('',#2488,.T.);
#1429=FACE_OUTER_BOUND('',#2489,.T.);
#1430=FACE_OUTER_BOUND('',#2490,.T.);
#1431=FACE_OUTER_BOUND('',#2491,.T.);
#1432=FACE_OUTER_BOUND('',#2492,.T.);
#1433=FACE_OUTER_BOUND('',#2493,.T.);
#1434=FACE_OUTER_BOUND('',#2494,.T.);
#1435=FACE_OUTER_BOUND('',#2495,.T.);
#1436=FACE_OUTER_BOUND('',#2496,.T.);
#1437=FACE_OUTER_BOUND('',#2497,.T.);
#1438=FACE_OUTER_BOUND('',#2498,.T.);
#1439=FACE_OUTER_BOUND('',#2499,.T.);
#1440=FACE_OUTER_BOUND('',#2500,.T.);
#1441=FACE_OUTER_BOUND('',#2501,.T.);
#1442=FACE_OUTER_BOUND('',#2502,.T.);
#1443=FACE_OUTER_BOUND('',#2503,.T.);
#1444=FACE_OUTER_BOUND('',#2504,.T.);
#1445=FACE_OUTER_BOUND('',#2505,.T.);
#1446=FACE_OUTER_BOUND('',#2506,.T.);
#1447=FACE_OUTER_BOUND('',#2507,.T.);
#1448=FACE_OUTER_BOUND('',#2508,.T.);
#1449=FACE_OUTER_BOUND('',#2509,.T.);
#1450=FACE_OUTER_BOUND('',#2510,.T.);
#1451=FACE_OUTER_BOUND('',#2511,.T.);
#1452=FACE_OUTER_BOUND('',#2512,.T.);
#1453=FACE_OUTER_BOUND('',#2513,.T.);
#1454=FACE_OUTER_BOUND('',#2514,.T.);
#1455=FACE_OUTER_BOUND('',#2515,.T.);
#1456=FACE_OUTER_BOUND('',#2516,.T.);
#1457=FACE_OUTER_BOUND('',#2517,.T.);
#1458=FACE_OUTER_BOUND('',#2518,.T.);
#1459=FACE_OUTER_BOUND('',#2519,.T.);
#1460=FACE_OUTER_BOUND('',#2520,.T.);
#1461=FACE_OUTER_BOUND('',#2521,.T.);
#1462=FACE_OUTER_BOUND('',#2522,.T.);
#1463=FACE_OUTER_BOUND('',#2523,.T.);
#1464=FACE_OUTER_BOUND('',#2524,.T.);
#1465=FACE_OUTER_BOUND('',#2525,.T.);
#1466=FACE_OUTER_BOUND('',#2526,.T.);
#1467=FACE_OUTER_BOUND('',#2527,.T.);
#1468=FACE_OUTER_BOUND('',#2528,.T.);
#1469=FACE_OUTER_BOUND('',#2529,.T.);
#1470=FACE_OUTER_BOUND('',#2530,.T.);
#1471=FACE_OUTER_BOUND('',#2531,.T.);
#1472=FACE_OUTER_BOUND('',#2532,.T.);
#1473=FACE_OUTER_BOUND('',#2533,.T.);
#1474=FACE_OUTER_BOUND('',#2534,.T.);
#1475=FACE_OUTER_BOUND('',#2535,.T.);
#1476=FACE_OUTER_BOUND('',#2536,.T.);
#1477=FACE_OUTER_BOUND('',#2537,.T.);
#1478=FACE_OUTER_BOUND('',#2538,.T.);
#1479=FACE_OUTER_BOUND('',#2539,.T.);
#1480=FACE_OUTER_BOUND('',#2540,.T.);
#1481=FACE_OUTER_BOUND('',#2541,.T.);
#1482=FACE_OUTER_BOUND('',#2542,.T.);
#1483=FACE_OUTER_BOUND('',#2543,.T.);
#1484=FACE_OUTER_BOUND('',#2544,.T.);
#1485=FACE_OUTER_BOUND('',#2545,.T.);
#1486=FACE_OUTER_BOUND('',#2546,.T.);
#1487=FACE_OUTER_BOUND('',#2547,.T.);
#1488=FACE_OUTER_BOUND('',#2548,.T.);
#1489=FACE_OUTER_BOUND('',#2549,.T.);
#1490=FACE_OUTER_BOUND('',#2550,.T.);
#1491=FACE_OUTER_BOUND('',#2551,.T.);
#1492=FACE_OUTER_BOUND('',#2553,.T.);
#1493=FACE_OUTER_BOUND('',#2555,.T.);
#1494=FACE_OUTER_BOUND('',#2556,.T.);
#1495=FACE_OUTER_BOUND('',#2557,.T.);
#1496=FACE_OUTER_BOUND('',#2558,.T.);
#1497=FACE_OUTER_BOUND('',#2559,.T.);
#1498=FACE_OUTER_BOUND('',#2560,.T.);
#1499=FACE_OUTER_BOUND('',#2561,.T.);
#1500=FACE_OUTER_BOUND('',#2562,.T.);
#1501=FACE_OUTER_BOUND('',#2563,.T.);
#1502=FACE_OUTER_BOUND('',#2564,.T.);
#1503=FACE_OUTER_BOUND('',#2565,.T.);
#1504=FACE_OUTER_BOUND('',#2566,.T.);
#1505=FACE_OUTER_BOUND('',#2567,.T.);
#1506=FACE_OUTER_BOUND('',#2568,.T.);
#1507=FACE_OUTER_BOUND('',#2569,.T.);
#1508=FACE_OUTER_BOUND('',#2570,.T.);
#1509=FACE_OUTER_BOUND('',#2571,.T.);
#1510=FACE_OUTER_BOUND('',#2572,.T.);
#1511=FACE_OUTER_BOUND('',#2573,.T.);
#1512=FACE_OUTER_BOUND('',#2574,.T.);
#1513=FACE_OUTER_BOUND('',#2575,.T.);
#1514=FACE_OUTER_BOUND('',#2576,.T.);
#1515=FACE_OUTER_BOUND('',#2577,.T.);
#1516=FACE_OUTER_BOUND('',#2578,.T.);
#1517=FACE_OUTER_BOUND('',#2579,.T.);
#1518=FACE_OUTER_BOUND('',#2580,.T.);
#1519=FACE_OUTER_BOUND('',#2581,.T.);
#1520=FACE_OUTER_BOUND('',#2582,.T.);
#1521=FACE_OUTER_BOUND('',#2583,.T.);
#1522=FACE_OUTER_BOUND('',#2584,.T.);
#1523=FACE_OUTER_BOUND('',#2585,.T.);
#1524=FACE_OUTER_BOUND('',#2586,.T.);
#1525=FACE_OUTER_BOUND('',#2587,.T.);
#1526=FACE_OUTER_BOUND('',#2588,.T.);
#1527=FACE_OUTER_BOUND('',#2589,.T.);
#1528=FACE_OUTER_BOUND('',#2590,.T.);
#1529=FACE_OUTER_BOUND('',#2592,.T.);
#1530=FACE_OUTER_BOUND('',#2594,.T.);
#1531=FACE_OUTER_BOUND('',#2595,.T.);
#1532=FACE_OUTER_BOUND('',#2596,.T.);
#1533=FACE_OUTER_BOUND('',#2597,.T.);
#1534=FACE_OUTER_BOUND('',#2598,.T.);
#1535=FACE_OUTER_BOUND('',#2599,.T.);
#1536=FACE_OUTER_BOUND('',#2600,.T.);
#1537=FACE_OUTER_BOUND('',#2601,.T.);
#1538=FACE_OUTER_BOUND('',#2602,.T.);
#1539=FACE_OUTER_BOUND('',#2604,.T.);
#1540=FACE_OUTER_BOUND('',#2606,.T.);
#1541=FACE_OUTER_BOUND('',#2607,.T.);
#1542=FACE_OUTER_BOUND('',#2608,.T.);
#1543=FACE_OUTER_BOUND('',#2609,.T.);
#1544=FACE_OUTER_BOUND('',#2610,.T.);
#1545=FACE_OUTER_BOUND('',#2611,.T.);
#1546=FACE_OUTER_BOUND('',#2612,.T.);
#1547=FACE_OUTER_BOUND('',#2613,.T.);
#1548=FACE_OUTER_BOUND('',#2614,.T.);
#1549=FACE_OUTER_BOUND('',#2615,.T.);
#1550=FACE_OUTER_BOUND('',#2616,.T.);
#1551=FACE_OUTER_BOUND('',#2617,.T.);
#1552=FACE_OUTER_BOUND('',#2618,.T.);
#1553=FACE_OUTER_BOUND('',#2619,.T.);
#1554=FACE_OUTER_BOUND('',#2620,.T.);
#1555=FACE_OUTER_BOUND('',#2621,.T.);
#1556=FACE_OUTER_BOUND('',#2622,.T.);
#1557=FACE_OUTER_BOUND('',#2623,.T.);
#1558=FACE_OUTER_BOUND('',#2624,.T.);
#1559=FACE_OUTER_BOUND('',#2625,.T.);
#1560=FACE_OUTER_BOUND('',#2626,.T.);
#1561=FACE_OUTER_BOUND('',#2627,.T.);
#1562=FACE_OUTER_BOUND('',#2628,.T.);
#1563=FACE_OUTER_BOUND('',#2629,.T.);
#1564=FACE_OUTER_BOUND('',#2630,.T.);
#1565=FACE_OUTER_BOUND('',#2631,.T.);
#1566=FACE_OUTER_BOUND('',#2632,.T.);
#1567=FACE_OUTER_BOUND('',#2633,.T.);
#1568=FACE_OUTER_BOUND('',#2634,.T.);
#1569=FACE_OUTER_BOUND('',#2635,.T.);
#1570=FACE_OUTER_BOUND('',#2636,.T.);
#1571=FACE_OUTER_BOUND('',#2637,.T.);
#1572=FACE_OUTER_BOUND('',#2638,.T.);
#1573=FACE_OUTER_BOUND('',#2639,.T.);
#1574=FACE_OUTER_BOUND('',#2640,.T.);
#1575=FACE_OUTER_BOUND('',#2641,.T.);
#1576=FACE_OUTER_BOUND('',#2642,.T.);
#1577=FACE_OUTER_BOUND('',#2643,.T.);
#1578=FACE_OUTER_BOUND('',#2644,.T.);
#1579=FACE_OUTER_BOUND('',#2645,.T.);
#1580=FACE_OUTER_BOUND('',#2646,.T.);
#1581=FACE_OUTER_BOUND('',#2648,.T.);
#1582=FACE_OUTER_BOUND('',#2650,.T.);
#1583=FACE_OUTER_BOUND('',#2651,.T.);
#1584=FACE_OUTER_BOUND('',#2652,.T.);
#1585=FACE_OUTER_BOUND('',#2653,.T.);
#1586=FACE_OUTER_BOUND('',#2654,.T.);
#1587=FACE_OUTER_BOUND('',#2655,.T.);
#1588=FACE_OUTER_BOUND('',#2656,.T.);
#1589=FACE_OUTER_BOUND('',#2657,.T.);
#1590=FACE_OUTER_BOUND('',#2658,.T.);
#1591=FACE_OUTER_BOUND('',#2659,.T.);
#1592=FACE_OUTER_BOUND('',#2660,.T.);
#1593=FACE_OUTER_BOUND('',#2661,.T.);
#1594=FACE_OUTER_BOUND('',#2662,.T.);
#1595=FACE_OUTER_BOUND('',#2663,.T.);
#1596=FACE_OUTER_BOUND('',#2664,.T.);
#1597=FACE_OUTER_BOUND('',#2665,.T.);
#1598=FACE_OUTER_BOUND('',#2666,.T.);
#1599=FACE_OUTER_BOUND('',#2667,.T.);
#1600=FACE_OUTER_BOUND('',#2668,.T.);
#1601=FACE_OUTER_BOUND('',#2669,.T.);
#1602=FACE_OUTER_BOUND('',#2670,.T.);
#1603=FACE_OUTER_BOUND('',#2671,.T.);
#1604=FACE_OUTER_BOUND('',#2672,.T.);
#1605=FACE_OUTER_BOUND('',#2673,.T.);
#1606=FACE_OUTER_BOUND('',#2674,.T.);
#1607=FACE_OUTER_BOUND('',#2675,.T.);
#1608=FACE_OUTER_BOUND('',#2676,.T.);
#1609=FACE_OUTER_BOUND('',#2677,.T.);
#1610=FACE_OUTER_BOUND('',#2678,.T.);
#1611=FACE_OUTER_BOUND('',#2679,.T.);
#1612=FACE_OUTER_BOUND('',#2680,.T.);
#1613=FACE_OUTER_BOUND('',#2681,.T.);
#1614=FACE_OUTER_BOUND('',#2682,.T.);
#1615=FACE_OUTER_BOUND('',#2683,.T.);
#1616=FACE_OUTER_BOUND('',#2684,.T.);
#1617=FACE_OUTER_BOUND('',#2685,.T.);
#1618=FACE_OUTER_BOUND('',#2686,.T.);
#1619=FACE_OUTER_BOUND('',#2687,.T.);
#1620=FACE_OUTER_BOUND('',#2688,.T.);
#1621=FACE_OUTER_BOUND('',#2689,.T.);
#1622=FACE_OUTER_BOUND('',#2690,.T.);
#1623=FACE_OUTER_BOUND('',#2691,.T.);
#1624=FACE_OUTER_BOUND('',#2692,.T.);
#1625=FACE_OUTER_BOUND('',#2693,.T.);
#1626=FACE_OUTER_BOUND('',#2694,.T.);
#1627=FACE_OUTER_BOUND('',#2695,.T.);
#1628=FACE_OUTER_BOUND('',#2696,.T.);
#1629=FACE_OUTER_BOUND('',#2697,.T.);
#1630=FACE_OUTER_BOUND('',#2698,.T.);
#1631=FACE_OUTER_BOUND('',#2699,.T.);
#1632=FACE_OUTER_BOUND('',#2700,.T.);
#1633=FACE_OUTER_BOUND('',#2701,.T.);
#1634=FACE_OUTER_BOUND('',#2702,.T.);
#1635=FACE_OUTER_BOUND('',#2703,.T.);
#1636=FACE_OUTER_BOUND('',#2704,.T.);
#1637=FACE_OUTER_BOUND('',#2705,.T.);
#1638=FACE_OUTER_BOUND('',#2706,.T.);
#1639=FACE_OUTER_BOUND('',#2707,.T.);
#1640=FACE_OUTER_BOUND('',#2708,.T.);
#1641=FACE_OUTER_BOUND('',#2709,.T.);
#1642=FACE_OUTER_BOUND('',#2710,.T.);
#1643=FACE_OUTER_BOUND('',#2711,.T.);
#1644=FACE_OUTER_BOUND('',#2712,.T.);
#1645=FACE_OUTER_BOUND('',#2713,.T.);
#1646=FACE_OUTER_BOUND('',#2714,.T.);
#1647=FACE_OUTER_BOUND('',#2715,.T.);
#1648=FACE_OUTER_BOUND('',#2716,.T.);
#1649=FACE_OUTER_BOUND('',#2717,.T.);
#1650=FACE_OUTER_BOUND('',#2718,.T.);
#1651=FACE_OUTER_BOUND('',#2719,.T.);
#1652=FACE_OUTER_BOUND('',#2720,.T.);
#1653=FACE_OUTER_BOUND('',#2721,.T.);
#1654=FACE_OUTER_BOUND('',#2722,.T.);
#1655=FACE_OUTER_BOUND('',#2723,.T.);
#1656=FACE_OUTER_BOUND('',#2724,.T.);
#1657=FACE_OUTER_BOUND('',#2725,.T.);
#1658=FACE_OUTER_BOUND('',#2726,.T.);
#1659=FACE_OUTER_BOUND('',#2727,.T.);
#1660=FACE_OUTER_BOUND('',#2728,.T.);
#1661=FACE_OUTER_BOUND('',#2729,.T.);
#1662=FACE_OUTER_BOUND('',#2730,.T.);
#1663=FACE_OUTER_BOUND('',#2731,.T.);
#1664=FACE_OUTER_BOUND('',#2732,.T.);
#1665=FACE_OUTER_BOUND('',#2733,.T.);
#1666=FACE_OUTER_BOUND('',#2734,.T.);
#1667=FACE_OUTER_BOUND('',#2735,.T.);
#1668=FACE_OUTER_BOUND('',#2736,.T.);
#1669=FACE_OUTER_BOUND('',#2737,.T.);
#1670=FACE_OUTER_BOUND('',#2738,.T.);
#1671=FACE_OUTER_BOUND('',#2739,.T.);
#1672=FACE_OUTER_BOUND('',#2740,.T.);
#1673=FACE_OUTER_BOUND('',#2741,.T.);
#1674=FACE_OUTER_BOUND('',#2742,.T.);
#1675=FACE_OUTER_BOUND('',#2743,.T.);
#1676=FACE_OUTER_BOUND('',#2744,.T.);
#1677=FACE_OUTER_BOUND('',#2745,.T.);
#1678=FACE_OUTER_BOUND('',#2746,.T.);
#1679=FACE_OUTER_BOUND('',#2747,.T.);
#1680=FACE_OUTER_BOUND('',#2748,.T.);
#1681=FACE_OUTER_BOUND('',#2749,.T.);
#1682=FACE_OUTER_BOUND('',#2750,.T.);
#1683=FACE_OUTER_BOUND('',#2751,.T.);
#1684=FACE_OUTER_BOUND('',#2752,.T.);
#1685=FACE_OUTER_BOUND('',#2753,.T.);
#1686=FACE_OUTER_BOUND('',#2754,.T.);
#1687=FACE_OUTER_BOUND('',#2755,.T.);
#1688=FACE_OUTER_BOUND('',#2756,.T.);
#1689=FACE_OUTER_BOUND('',#2757,.T.);
#1690=FACE_OUTER_BOUND('',#2758,.T.);
#1691=FACE_OUTER_BOUND('',#2759,.T.);
#1692=FACE_OUTER_BOUND('',#2760,.T.);
#1693=FACE_OUTER_BOUND('',#2761,.T.);
#1694=FACE_OUTER_BOUND('',#2762,.T.);
#1695=FACE_OUTER_BOUND('',#2763,.T.);
#1696=FACE_OUTER_BOUND('',#2764,.T.);
#1697=FACE_OUTER_BOUND('',#2765,.T.);
#1698=FACE_OUTER_BOUND('',#2766,.T.);
#1699=FACE_OUTER_BOUND('',#2767,.T.);
#1700=FACE_OUTER_BOUND('',#2768,.T.);
#1701=FACE_OUTER_BOUND('',#2769,.T.);
#1702=FACE_OUTER_BOUND('',#2770,.T.);
#1703=FACE_OUTER_BOUND('',#2771,.T.);
#1704=FACE_OUTER_BOUND('',#2772,.T.);
#1705=FACE_OUTER_BOUND('',#2773,.T.);
#1706=FACE_OUTER_BOUND('',#2774,.T.);
#1707=FACE_OUTER_BOUND('',#2775,.T.);
#1708=FACE_OUTER_BOUND('',#2776,.T.);
#1709=FACE_OUTER_BOUND('',#2777,.T.);
#1710=FACE_OUTER_BOUND('',#2778,.T.);
#1711=FACE_OUTER_BOUND('',#2779,.T.);
#1712=FACE_OUTER_BOUND('',#2780,.T.);
#1713=FACE_OUTER_BOUND('',#2781,.T.);
#1714=FACE_OUTER_BOUND('',#2782,.T.);
#1715=FACE_OUTER_BOUND('',#2783,.T.);
#1716=FACE_OUTER_BOUND('',#2784,.T.);
#1717=FACE_OUTER_BOUND('',#2785,.T.);
#1718=FACE_OUTER_BOUND('',#2786,.T.);
#1719=FACE_OUTER_BOUND('',#2787,.T.);
#1720=FACE_OUTER_BOUND('',#2788,.T.);
#1721=FACE_OUTER_BOUND('',#2789,.T.);
#1722=FACE_OUTER_BOUND('',#2790,.T.);
#1723=FACE_OUTER_BOUND('',#2791,.T.);
#1724=FACE_OUTER_BOUND('',#2792,.T.);
#1725=FACE_OUTER_BOUND('',#2793,.T.);
#1726=FACE_OUTER_BOUND('',#2794,.T.);
#1727=FACE_OUTER_BOUND('',#2795,.T.);
#1728=FACE_OUTER_BOUND('',#2796,.T.);
#1729=FACE_OUTER_BOUND('',#2797,.T.);
#1730=FACE_OUTER_BOUND('',#2798,.T.);
#1731=FACE_OUTER_BOUND('',#2799,.T.);
#1732=FACE_OUTER_BOUND('',#2800,.T.);
#1733=FACE_OUTER_BOUND('',#2801,.T.);
#1734=FACE_OUTER_BOUND('',#2802,.T.);
#1735=FACE_OUTER_BOUND('',#2803,.T.);
#1736=FACE_OUTER_BOUND('',#2804,.T.);
#1737=FACE_OUTER_BOUND('',#2805,.T.);
#1738=FACE_OUTER_BOUND('',#2806,.T.);
#1739=FACE_OUTER_BOUND('',#2807,.T.);
#1740=FACE_OUTER_BOUND('',#2808,.T.);
#1741=FACE_OUTER_BOUND('',#2809,.T.);
#1742=FACE_OUTER_BOUND('',#2810,.T.);
#1743=FACE_OUTER_BOUND('',#2811,.T.);
#1744=FACE_OUTER_BOUND('',#2812,.T.);
#1745=FACE_OUTER_BOUND('',#2813,.T.);
#1746=FACE_OUTER_BOUND('',#2814,.T.);
#1747=FACE_OUTER_BOUND('',#2815,.T.);
#1748=FACE_OUTER_BOUND('',#2816,.T.);
#1749=FACE_OUTER_BOUND('',#2817,.T.);
#1750=FACE_OUTER_BOUND('',#2818,.T.);
#1751=FACE_OUTER_BOUND('',#2819,.T.);
#1752=FACE_OUTER_BOUND('',#2820,.T.);
#1753=FACE_OUTER_BOUND('',#2821,.T.);
#1754=FACE_OUTER_BOUND('',#2822,.T.);
#1755=FACE_OUTER_BOUND('',#2823,.T.);
#1756=FACE_OUTER_BOUND('',#2824,.T.);
#1757=FACE_OUTER_BOUND('',#2825,.T.);
#1758=FACE_OUTER_BOUND('',#2826,.T.);
#1759=FACE_OUTER_BOUND('',#2827,.T.);
#1760=FACE_OUTER_BOUND('',#2828,.T.);
#1761=FACE_OUTER_BOUND('',#2829,.T.);
#1762=FACE_OUTER_BOUND('',#2830,.T.);
#1763=FACE_OUTER_BOUND('',#2831,.T.);
#1764=FACE_OUTER_BOUND('',#2832,.T.);
#1765=FACE_OUTER_BOUND('',#2833,.T.);
#1766=FACE_OUTER_BOUND('',#2834,.T.);
#1767=FACE_OUTER_BOUND('',#2835,.T.);
#1768=FACE_OUTER_BOUND('',#2836,.T.);
#1769=FACE_OUTER_BOUND('',#2837,.T.);
#1770=FACE_OUTER_BOUND('',#2838,.T.);
#1771=FACE_OUTER_BOUND('',#2839,.T.);
#1772=FACE_OUTER_BOUND('',#2840,.T.);
#1773=FACE_OUTER_BOUND('',#2841,.T.);
#1774=FACE_OUTER_BOUND('',#2842,.T.);
#1775=FACE_OUTER_BOUND('',#2843,.T.);
#1776=FACE_OUTER_BOUND('',#2844,.T.);
#1777=FACE_OUTER_BOUND('',#2845,.T.);
#1778=FACE_OUTER_BOUND('',#2846,.T.);
#1779=FACE_OUTER_BOUND('',#2847,.T.);
#1780=FACE_OUTER_BOUND('',#2848,.T.);
#1781=FACE_OUTER_BOUND('',#2849,.T.);
#1782=FACE_OUTER_BOUND('',#2850,.T.);
#1783=FACE_OUTER_BOUND('',#2851,.T.);
#1784=FACE_OUTER_BOUND('',#2852,.T.);
#1785=FACE_OUTER_BOUND('',#2853,.T.);
#1786=FACE_OUTER_BOUND('',#2854,.T.);
#1787=FACE_OUTER_BOUND('',#2855,.T.);
#1788=FACE_OUTER_BOUND('',#2856,.T.);
#1789=FACE_OUTER_BOUND('',#2857,.T.);
#1790=FACE_OUTER_BOUND('',#2858,.T.);
#1791=FACE_OUTER_BOUND('',#2859,.T.);
#1792=FACE_OUTER_BOUND('',#2860,.T.);
#1793=FACE_OUTER_BOUND('',#2861,.T.);
#1794=FACE_OUTER_BOUND('',#2862,.T.);
#1795=FACE_OUTER_BOUND('',#2863,.T.);
#1796=FACE_OUTER_BOUND('',#2864,.T.);
#1797=FACE_OUTER_BOUND('',#2865,.T.);
#1798=FACE_OUTER_BOUND('',#2866,.T.);
#1799=FACE_OUTER_BOUND('',#2867,.T.);
#1800=FACE_OUTER_BOUND('',#2868,.T.);
#1801=FACE_OUTER_BOUND('',#2869,.T.);
#1802=FACE_OUTER_BOUND('',#2870,.T.);
#1803=FACE_OUTER_BOUND('',#2871,.T.);
#1804=FACE_OUTER_BOUND('',#2872,.T.);
#1805=FACE_OUTER_BOUND('',#2873,.T.);
#1806=FACE_OUTER_BOUND('',#2874,.T.);
#1807=FACE_OUTER_BOUND('',#2875,.T.);
#1808=FACE_OUTER_BOUND('',#2876,.T.);
#1809=FACE_OUTER_BOUND('',#2877,.T.);
#1810=FACE_OUTER_BOUND('',#2878,.T.);
#1811=FACE_OUTER_BOUND('',#2879,.T.);
#1812=FACE_OUTER_BOUND('',#2880,.T.);
#1813=FACE_OUTER_BOUND('',#2881,.T.);
#1814=FACE_OUTER_BOUND('',#2882,.T.);
#1815=FACE_OUTER_BOUND('',#2883,.T.);
#1816=FACE_OUTER_BOUND('',#2884,.T.);
#1817=FACE_OUTER_BOUND('',#2885,.T.);
#1818=FACE_OUTER_BOUND('',#2886,.T.);
#1819=FACE_OUTER_BOUND('',#2887,.T.);
#1820=FACE_OUTER_BOUND('',#2888,.T.);
#1821=FACE_OUTER_BOUND('',#2889,.T.);
#1822=FACE_OUTER_BOUND('',#2890,.T.);
#1823=FACE_OUTER_BOUND('',#2891,.T.);
#1824=FACE_OUTER_BOUND('',#2892,.T.);
#1825=FACE_OUTER_BOUND('',#2893,.T.);
#1826=FACE_OUTER_BOUND('',#2894,.T.);
#1827=FACE_OUTER_BOUND('',#2895,.T.);
#1828=FACE_OUTER_BOUND('',#2896,.T.);
#1829=FACE_OUTER_BOUND('',#2897,.T.);
#1830=FACE_OUTER_BOUND('',#2898,.T.);
#1831=FACE_OUTER_BOUND('',#2899,.T.);
#1832=FACE_OUTER_BOUND('',#2900,.T.);
#1833=FACE_OUTER_BOUND('',#2901,.T.);
#1834=FACE_OUTER_BOUND('',#2902,.T.);
#1835=FACE_OUTER_BOUND('',#2903,.T.);
#1836=FACE_OUTER_BOUND('',#2904,.T.);
#1837=FACE_OUTER_BOUND('',#2905,.T.);
#1838=FACE_OUTER_BOUND('',#2906,.T.);
#1839=FACE_OUTER_BOUND('',#2907,.T.);
#1840=FACE_OUTER_BOUND('',#2908,.T.);
#1841=FACE_OUTER_BOUND('',#2909,.T.);
#1842=FACE_OUTER_BOUND('',#2910,.T.);
#1843=FACE_OUTER_BOUND('',#2911,.T.);
#1844=FACE_OUTER_BOUND('',#2912,.T.);
#1845=FACE_OUTER_BOUND('',#2913,.T.);
#1846=FACE_OUTER_BOUND('',#2927,.T.);
#1847=FACE_OUTER_BOUND('',#2928,.T.);
#1848=FACE_OUTER_BOUND('',#2929,.T.);
#1849=FACE_OUTER_BOUND('',#2930,.T.);
#1850=FACE_OUTER_BOUND('',#2931,.T.);
#1851=FACE_OUTER_BOUND('',#2932,.T.);
#1852=FACE_OUTER_BOUND('',#2933,.T.);
#1853=FACE_OUTER_BOUND('',#2934,.T.);
#1854=FACE_OUTER_BOUND('',#2935,.T.);
#1855=FACE_OUTER_BOUND('',#2936,.T.);
#1856=FACE_OUTER_BOUND('',#2937,.T.);
#1857=FACE_OUTER_BOUND('',#2938,.T.);
#1858=FACE_OUTER_BOUND('',#2939,.T.);
#1859=FACE_OUTER_BOUND('',#2940,.T.);
#1860=FACE_OUTER_BOUND('',#2941,.T.);
#1861=FACE_OUTER_BOUND('',#2942,.T.);
#1862=FACE_OUTER_BOUND('',#2943,.T.);
#1863=FACE_OUTER_BOUND('',#2944,.T.);
#1864=FACE_OUTER_BOUND('',#2945,.T.);
#1865=FACE_OUTER_BOUND('',#2946,.T.);
#1866=FACE_OUTER_BOUND('',#2947,.T.);
#1867=FACE_OUTER_BOUND('',#2948,.T.);
#1868=FACE_OUTER_BOUND('',#2949,.T.);
#1869=FACE_OUTER_BOUND('',#2950,.T.);
#1870=FACE_OUTER_BOUND('',#2951,.T.);
#1871=FACE_OUTER_BOUND('',#2952,.T.);
#1872=FACE_OUTER_BOUND('',#2953,.T.);
#1873=FACE_OUTER_BOUND('',#2954,.T.);
#1874=FACE_OUTER_BOUND('',#2955,.T.);
#1875=FACE_OUTER_BOUND('',#2956,.T.);
#1876=FACE_OUTER_BOUND('',#2957,.T.);
#1877=FACE_OUTER_BOUND('',#2958,.T.);
#1878=FACE_OUTER_BOUND('',#2959,.T.);
#1879=FACE_OUTER_BOUND('',#2960,.T.);
#1880=FACE_OUTER_BOUND('',#2961,.T.);
#1881=FACE_OUTER_BOUND('',#2962,.T.);
#1882=FACE_OUTER_BOUND('',#2963,.T.);
#1883=FACE_OUTER_BOUND('',#2964,.T.);
#1884=FACE_OUTER_BOUND('',#2965,.T.);
#1885=FACE_OUTER_BOUND('',#2979,.T.);
#1886=FACE_OUTER_BOUND('',#2980,.T.);
#1887=FACE_OUTER_BOUND('',#2981,.T.);
#1888=FACE_OUTER_BOUND('',#2982,.T.);
#1889=FACE_OUTER_BOUND('',#2983,.T.);
#1890=FACE_OUTER_BOUND('',#2984,.T.);
#1891=FACE_OUTER_BOUND('',#2985,.T.);
#1892=FACE_OUTER_BOUND('',#2986,.T.);
#1893=FACE_OUTER_BOUND('',#2987,.T.);
#1894=FACE_OUTER_BOUND('',#2988,.T.);
#1895=FACE_OUTER_BOUND('',#2989,.T.);
#1896=FACE_OUTER_BOUND('',#2990,.T.);
#1897=FACE_OUTER_BOUND('',#2991,.T.);
#1898=FACE_OUTER_BOUND('',#2992,.T.);
#1899=FACE_OUTER_BOUND('',#2993,.T.);
#1900=FACE_OUTER_BOUND('',#2994,.T.);
#1901=FACE_OUTER_BOUND('',#2995,.T.);
#1902=FACE_OUTER_BOUND('',#2996,.T.);
#1903=FACE_OUTER_BOUND('',#2997,.T.);
#1904=FACE_OUTER_BOUND('',#2998,.T.);
#1905=FACE_OUTER_BOUND('',#2999,.T.);
#1906=FACE_OUTER_BOUND('',#3000,.T.);
#1907=FACE_OUTER_BOUND('',#3001,.T.);
#1908=FACE_OUTER_BOUND('',#3002,.T.);
#1909=FACE_OUTER_BOUND('',#3003,.T.);
#1910=FACE_OUTER_BOUND('',#3004,.T.);
#1911=FACE_OUTER_BOUND('',#3005,.T.);
#1912=FACE_OUTER_BOUND('',#3006,.T.);
#1913=FACE_OUTER_BOUND('',#3007,.T.);
#1914=FACE_OUTER_BOUND('',#3008,.T.);
#1915=FACE_OUTER_BOUND('',#3009,.T.);
#1916=FACE_OUTER_BOUND('',#3010,.T.);
#1917=FACE_OUTER_BOUND('',#3011,.T.);
#1918=FACE_OUTER_BOUND('',#3012,.T.);
#1919=FACE_OUTER_BOUND('',#3013,.T.);
#1920=FACE_OUTER_BOUND('',#3014,.T.);
#1921=FACE_OUTER_BOUND('',#3015,.T.);
#1922=FACE_OUTER_BOUND('',#3016,.T.);
#1923=FACE_OUTER_BOUND('',#3017,.T.);
#1924=FACE_OUTER_BOUND('',#3018,.T.);
#1925=FACE_OUTER_BOUND('',#3019,.T.);
#1926=FACE_OUTER_BOUND('',#3020,.T.);
#1927=FACE_OUTER_BOUND('',#3021,.T.);
#1928=FACE_OUTER_BOUND('',#3022,.T.);
#1929=FACE_OUTER_BOUND('',#3023,.T.);
#1930=FACE_OUTER_BOUND('',#3024,.T.);
#1931=FACE_OUTER_BOUND('',#3025,.T.);
#1932=FACE_OUTER_BOUND('',#3026,.T.);
#1933=FACE_OUTER_BOUND('',#3027,.T.);
#1934=FACE_OUTER_BOUND('',#3028,.T.);
#1935=FACE_OUTER_BOUND('',#3029,.T.);
#1936=FACE_OUTER_BOUND('',#3030,.T.);
#1937=FACE_OUTER_BOUND('',#3031,.T.);
#1938=FACE_OUTER_BOUND('',#3032,.T.);
#1939=FACE_OUTER_BOUND('',#3033,.T.);
#1940=FACE_OUTER_BOUND('',#3034,.T.);
#1941=FACE_OUTER_BOUND('',#3035,.T.);
#1942=FACE_OUTER_BOUND('',#3036,.T.);
#1943=FACE_OUTER_BOUND('',#3037,.T.);
#1944=FACE_OUTER_BOUND('',#3038,.T.);
#1945=FACE_OUTER_BOUND('',#3039,.T.);
#1946=FACE_OUTER_BOUND('',#3040,.T.);
#1947=FACE_OUTER_BOUND('',#3041,.T.);
#1948=FACE_OUTER_BOUND('',#3042,.T.);
#1949=FACE_OUTER_BOUND('',#3043,.T.);
#1950=FACE_OUTER_BOUND('',#3044,.T.);
#1951=FACE_OUTER_BOUND('',#3045,.T.);
#1952=FACE_OUTER_BOUND('',#3046,.T.);
#1953=FACE_OUTER_BOUND('',#3047,.T.);
#1954=FACE_OUTER_BOUND('',#3048,.T.);
#1955=FACE_OUTER_BOUND('',#3049,.T.);
#1956=FACE_OUTER_BOUND('',#3050,.T.);
#1957=FACE_OUTER_BOUND('',#3051,.T.);
#1958=FACE_OUTER_BOUND('',#3052,.T.);
#1959=FACE_OUTER_BOUND('',#3053,.T.);
#1960=FACE_OUTER_BOUND('',#3054,.T.);
#1961=FACE_OUTER_BOUND('',#3055,.T.);
#1962=FACE_OUTER_BOUND('',#3056,.T.);
#1963=FACE_OUTER_BOUND('',#3057,.T.);
#1964=FACE_OUTER_BOUND('',#3058,.T.);
#1965=FACE_OUTER_BOUND('',#3059,.T.);
#1966=FACE_OUTER_BOUND('',#3060,.T.);
#1967=FACE_OUTER_BOUND('',#3061,.T.);
#1968=FACE_OUTER_BOUND('',#3062,.T.);
#1969=FACE_OUTER_BOUND('',#3063,.T.);
#1970=FACE_OUTER_BOUND('',#3064,.T.);
#1971=FACE_OUTER_BOUND('',#3065,.T.);
#1972=FACE_OUTER_BOUND('',#3066,.T.);
#1973=FACE_OUTER_BOUND('',#3067,.T.);
#1974=FACE_OUTER_BOUND('',#3068,.T.);
#1975=FACE_OUTER_BOUND('',#3069,.T.);
#1976=FACE_OUTER_BOUND('',#3070,.T.);
#1977=FACE_OUTER_BOUND('',#3071,.T.);
#1978=FACE_OUTER_BOUND('',#3072,.T.);
#1979=FACE_OUTER_BOUND('',#3073,.T.);
#1980=FACE_OUTER_BOUND('',#3074,.T.);
#1981=FACE_OUTER_BOUND('',#3075,.T.);
#1982=FACE_OUTER_BOUND('',#3076,.T.);
#1983=FACE_OUTER_BOUND('',#3077,.T.);
#1984=FACE_OUTER_BOUND('',#3078,.T.);
#1985=FACE_OUTER_BOUND('',#3079,.T.);
#1986=FACE_OUTER_BOUND('',#3080,.T.);
#1987=FACE_OUTER_BOUND('',#3081,.T.);
#1988=FACE_OUTER_BOUND('',#3082,.T.);
#1989=FACE_OUTER_BOUND('',#3083,.T.);
#1990=FACE_OUTER_BOUND('',#3084,.T.);
#1991=FACE_OUTER_BOUND('',#3085,.T.);
#1992=FACE_OUTER_BOUND('',#3086,.T.);
#1993=FACE_OUTER_BOUND('',#3087,.T.);
#1994=FACE_OUTER_BOUND('',#3088,.T.);
#1995=FACE_OUTER_BOUND('',#3089,.T.);
#1996=FACE_OUTER_BOUND('',#3090,.T.);
#1997=FACE_OUTER_BOUND('',#3091,.T.);
#1998=FACE_OUTER_BOUND('',#3092,.T.);
#1999=FACE_OUTER_BOUND('',#3093,.T.);
#2000=FACE_OUTER_BOUND('',#3094,.T.);
#2001=FACE_OUTER_BOUND('',#3095,.T.);
#2002=FACE_OUTER_BOUND('',#3096,.T.);
#2003=FACE_OUTER_BOUND('',#3097,.T.);
#2004=FACE_OUTER_BOUND('',#3098,.T.);
#2005=FACE_OUTER_BOUND('',#3099,.T.);
#2006=FACE_OUTER_BOUND('',#3100,.T.);
#2007=FACE_OUTER_BOUND('',#3101,.T.);
#2008=FACE_OUTER_BOUND('',#3102,.T.);
#2009=FACE_OUTER_BOUND('',#3103,.T.);
#2010=FACE_OUTER_BOUND('',#3104,.T.);
#2011=FACE_OUTER_BOUND('',#3105,.T.);
#2012=FACE_OUTER_BOUND('',#3106,.T.);
#2013=FACE_OUTER_BOUND('',#3107,.T.);
#2014=FACE_OUTER_BOUND('',#3108,.T.);
#2015=FACE_OUTER_BOUND('',#3109,.T.);
#2016=FACE_OUTER_BOUND('',#3110,.T.);
#2017=FACE_OUTER_BOUND('',#3111,.T.);
#2018=FACE_OUTER_BOUND('',#3112,.T.);
#2019=FACE_OUTER_BOUND('',#3113,.T.);
#2020=FACE_OUTER_BOUND('',#3114,.T.);
#2021=FACE_OUTER_BOUND('',#3115,.T.);
#2022=FACE_OUTER_BOUND('',#3116,.T.);
#2023=FACE_OUTER_BOUND('',#3117,.T.);
#2024=FACE_OUTER_BOUND('',#3118,.T.);
#2025=FACE_OUTER_BOUND('',#3119,.T.);
#2026=FACE_OUTER_BOUND('',#3120,.T.);
#2027=FACE_OUTER_BOUND('',#3121,.T.);
#2028=FACE_OUTER_BOUND('',#3122,.T.);
#2029=FACE_OUTER_BOUND('',#3123,.T.);
#2030=FACE_OUTER_BOUND('',#3124,.T.);
#2031=FACE_OUTER_BOUND('',#3125,.T.);
#2032=FACE_OUTER_BOUND('',#3126,.T.);
#2033=FACE_OUTER_BOUND('',#3127,.T.);
#2034=FACE_OUTER_BOUND('',#3128,.T.);
#2035=FACE_OUTER_BOUND('',#3129,.T.);
#2036=FACE_OUTER_BOUND('',#3130,.T.);
#2037=FACE_OUTER_BOUND('',#3131,.T.);
#2038=FACE_OUTER_BOUND('',#3132,.T.);
#2039=FACE_OUTER_BOUND('',#3133,.T.);
#2040=FACE_OUTER_BOUND('',#3134,.T.);
#2041=FACE_OUTER_BOUND('',#3135,.T.);
#2042=FACE_OUTER_BOUND('',#3136,.T.);
#2043=FACE_OUTER_BOUND('',#3137,.T.);
#2044=FACE_OUTER_BOUND('',#3138,.T.);
#2045=FACE_OUTER_BOUND('',#3139,.T.);
#2046=FACE_OUTER_BOUND('',#3140,.T.);
#2047=FACE_OUTER_BOUND('',#3141,.T.);
#2048=FACE_OUTER_BOUND('',#3142,.T.);
#2049=FACE_OUTER_BOUND('',#3143,.T.);
#2050=FACE_OUTER_BOUND('',#3144,.T.);
#2051=FACE_OUTER_BOUND('',#3145,.T.);
#2052=FACE_OUTER_BOUND('',#3146,.T.);
#2053=FACE_OUTER_BOUND('',#3147,.T.);
#2054=FACE_OUTER_BOUND('',#3148,.T.);
#2055=FACE_OUTER_BOUND('',#3149,.T.);
#2056=FACE_OUTER_BOUND('',#3150,.T.);
#2057=FACE_OUTER_BOUND('',#3151,.T.);
#2058=FACE_OUTER_BOUND('',#3152,.T.);
#2059=FACE_OUTER_BOUND('',#3153,.T.);
#2060=FACE_OUTER_BOUND('',#3154,.T.);
#2061=FACE_OUTER_BOUND('',#3155,.T.);
#2062=FACE_OUTER_BOUND('',#3156,.T.);
#2063=FACE_OUTER_BOUND('',#3157,.T.);
#2064=FACE_OUTER_BOUND('',#3158,.T.);
#2065=FACE_OUTER_BOUND('',#3159,.T.);
#2066=FACE_OUTER_BOUND('',#3160,.T.);
#2067=FACE_OUTER_BOUND('',#3161,.T.);
#2068=FACE_OUTER_BOUND('',#3162,.T.);
#2069=FACE_OUTER_BOUND('',#3163,.T.);
#2070=FACE_OUTER_BOUND('',#3164,.T.);
#2071=FACE_OUTER_BOUND('',#3165,.T.);
#2072=FACE_OUTER_BOUND('',#3166,.T.);
#2073=FACE_OUTER_BOUND('',#3167,.T.);
#2074=FACE_OUTER_BOUND('',#3168,.T.);
#2075=FACE_OUTER_BOUND('',#3169,.T.);
#2076=FACE_OUTER_BOUND('',#3170,.T.);
#2077=FACE_OUTER_BOUND('',#3171,.T.);
#2078=FACE_OUTER_BOUND('',#3172,.T.);
#2079=FACE_OUTER_BOUND('',#3173,.T.);
#2080=FACE_OUTER_BOUND('',#3174,.T.);
#2081=FACE_OUTER_BOUND('',#3175,.T.);
#2082=FACE_OUTER_BOUND('',#3176,.T.);
#2083=FACE_OUTER_BOUND('',#3177,.T.);
#2084=FACE_OUTER_BOUND('',#3178,.T.);
#2085=FACE_OUTER_BOUND('',#3179,.T.);
#2086=FACE_OUTER_BOUND('',#3180,.T.);
#2087=FACE_OUTER_BOUND('',#3181,.T.);
#2088=FACE_OUTER_BOUND('',#3182,.T.);
#2089=FACE_OUTER_BOUND('',#3183,.T.);
#2090=FACE_OUTER_BOUND('',#3184,.T.);
#2091=FACE_OUTER_BOUND('',#3185,.T.);
#2092=FACE_OUTER_BOUND('',#3186,.T.);
#2093=FACE_OUTER_BOUND('',#3187,.T.);
#2094=FACE_OUTER_BOUND('',#3188,.T.);
#2095=FACE_OUTER_BOUND('',#3189,.T.);
#2096=FACE_OUTER_BOUND('',#3190,.T.);
#2097=FACE_OUTER_BOUND('',#3191,.T.);
#2098=FACE_OUTER_BOUND('',#3192,.T.);
#2099=FACE_OUTER_BOUND('',#3193,.T.);
#2100=FACE_OUTER_BOUND('',#3194,.T.);
#2101=FACE_OUTER_BOUND('',#3195,.T.);
#2102=FACE_OUTER_BOUND('',#3196,.T.);
#2103=FACE_OUTER_BOUND('',#3197,.T.);
#2104=FACE_OUTER_BOUND('',#3198,.T.);
#2105=FACE_OUTER_BOUND('',#3199,.T.);
#2106=FACE_OUTER_BOUND('',#3200,.T.);
#2107=FACE_OUTER_BOUND('',#3201,.T.);
#2108=FACE_OUTER_BOUND('',#3202,.T.);
#2109=FACE_OUTER_BOUND('',#3203,.T.);
#2110=FACE_OUTER_BOUND('',#3204,.T.);
#2111=FACE_OUTER_BOUND('',#3205,.T.);
#2112=FACE_OUTER_BOUND('',#3206,.T.);
#2113=FACE_OUTER_BOUND('',#3208,.T.);
#2114=FACE_OUTER_BOUND('',#3209,.T.);
#2115=FACE_OUTER_BOUND('',#3210,.T.);
#2116=FACE_OUTER_BOUND('',#3212,.T.);
#2117=FACE_OUTER_BOUND('',#3213,.T.);
#2118=FACE_OUTER_BOUND('',#3214,.T.);
#2119=FACE_OUTER_BOUND('',#3215,.T.);
#2120=FACE_OUTER_BOUND('',#3216,.T.);
#2121=FACE_OUTER_BOUND('',#3217,.T.);
#2122=FACE_OUTER_BOUND('',#3219,.T.);
#2123=FACE_OUTER_BOUND('',#3220,.T.);
#2124=FACE_OUTER_BOUND('',#3221,.T.);
#2125=FACE_OUTER_BOUND('',#3223,.T.);
#2126=FACE_OUTER_BOUND('',#3224,.T.);
#2127=FACE_OUTER_BOUND('',#3225,.T.);
#2128=FACE_OUTER_BOUND('',#3226,.T.);
#2129=FACE_OUTER_BOUND('',#3227,.T.);
#2130=FACE_OUTER_BOUND('',#3228,.T.);
#2131=FACE_OUTER_BOUND('',#3229,.T.);
#2132=FACE_OUTER_BOUND('',#3230,.T.);
#2133=FACE_OUTER_BOUND('',#3231,.T.);
#2134=FACE_OUTER_BOUND('',#3232,.T.);
#2135=FACE_OUTER_BOUND('',#3233,.T.);
#2136=FACE_OUTER_BOUND('',#3234,.T.);
#2137=FACE_OUTER_BOUND('',#3235,.T.);
#2138=FACE_OUTER_BOUND('',#3236,.T.);
#2139=FACE_OUTER_BOUND('',#3237,.T.);
#2140=FACE_OUTER_BOUND('',#3238,.T.);
#2141=FACE_OUTER_BOUND('',#3239,.T.);
#2142=FACE_OUTER_BOUND('',#3240,.T.);
#2143=FACE_OUTER_BOUND('',#3241,.T.);
#2144=FACE_OUTER_BOUND('',#3242,.T.);
#2145=FACE_OUTER_BOUND('',#3243,.T.);
#2146=FACE_OUTER_BOUND('',#3244,.T.);
#2147=FACE_OUTER_BOUND('',#3246,.T.);
#2148=FACE_OUTER_BOUND('',#3247,.T.);
#2149=FACE_OUTER_BOUND('',#3248,.T.);
#2150=FACE_OUTER_BOUND('',#3250,.T.);
#2151=FACE_OUTER_BOUND('',#3251,.T.);
#2152=FACE_OUTER_BOUND('',#3260,.T.);
#2153=FACE_OUTER_BOUND('',#3269,.T.);
#2154=FACE_OUTER_BOUND('',#3270,.T.);
#2155=FACE_OUTER_BOUND('',#3271,.T.);
#2156=FACE_OUTER_BOUND('',#3272,.T.);
#2157=FACE_OUTER_BOUND('',#3273,.T.);
#2158=FACE_OUTER_BOUND('',#3290,.T.);
#2159=FACE_OUTER_BOUND('',#3291,.T.);
#2160=FACE_OUTER_BOUND('',#3292,.T.);
#2161=FACE_OUTER_BOUND('',#3293,.T.);
#2162=FACE_OUTER_BOUND('',#3294,.T.);
#2163=FACE_OUTER_BOUND('',#3295,.T.);
#2164=FACE_OUTER_BOUND('',#3296,.T.);
#2165=FACE_OUTER_BOUND('',#3297,.T.);
#2166=FACE_OUTER_BOUND('',#3298,.T.);
#2167=FACE_OUTER_BOUND('',#3299,.T.);
#2168=FACE_OUTER_BOUND('',#3300,.T.);
#2169=FACE_OUTER_BOUND('',#3301,.T.);
#2170=FACE_OUTER_BOUND('',#3302,.T.);
#2171=FACE_OUTER_BOUND('',#3303,.T.);
#2172=FACE_OUTER_BOUND('',#3304,.T.);
#2173=FACE_OUTER_BOUND('',#3305,.T.);
#2174=FACE_OUTER_BOUND('',#3306,.T.);
#2175=FACE_OUTER_BOUND('',#3307,.T.);
#2176=FACE_OUTER_BOUND('',#3308,.T.);
#2177=FACE_OUTER_BOUND('',#3309,.T.);
#2178=FACE_OUTER_BOUND('',#3310,.T.);
#2179=FACE_OUTER_BOUND('',#3311,.T.);
#2180=FACE_OUTER_BOUND('',#3312,.T.);
#2181=FACE_OUTER_BOUND('',#3313,.T.);
#2182=FACE_OUTER_BOUND('',#3314,.T.);
#2183=FACE_OUTER_BOUND('',#3315,.T.);
#2184=FACE_OUTER_BOUND('',#3316,.T.);
#2185=FACE_OUTER_BOUND('',#3317,.T.);
#2186=FACE_OUTER_BOUND('',#3318,.T.);
#2187=FACE_OUTER_BOUND('',#3319,.T.);
#2188=FACE_OUTER_BOUND('',#3320,.T.);
#2189=FACE_OUTER_BOUND('',#3321,.T.);
#2190=FACE_OUTER_BOUND('',#3322,.T.);
#2191=FACE_OUTER_BOUND('',#3323,.T.);
#2192=FACE_OUTER_BOUND('',#3324,.T.);
#2193=FACE_OUTER_BOUND('',#3325,.T.);
#2194=FACE_OUTER_BOUND('',#3326,.T.);
#2195=FACE_OUTER_BOUND('',#3327,.T.);
#2196=FACE_OUTER_BOUND('',#3328,.T.);
#2197=FACE_OUTER_BOUND('',#3329,.T.);
#2198=FACE_OUTER_BOUND('',#3330,.T.);
#2199=FACE_OUTER_BOUND('',#3331,.T.);
#2200=FACE_OUTER_BOUND('',#3333,.T.);
#2201=FACE_OUTER_BOUND('',#3335,.T.);
#2202=FACE_OUTER_BOUND('',#3336,.T.);
#2203=FACE_OUTER_BOUND('',#3337,.T.);
#2204=FACE_OUTER_BOUND('',#3338,.T.);
#2205=FACE_OUTER_BOUND('',#3339,.T.);
#2206=FACE_OUTER_BOUND('',#3340,.T.);
#2207=FACE_OUTER_BOUND('',#3342,.T.);
#2208=FACE_OUTER_BOUND('',#3344,.T.);
#2209=FACE_OUTER_BOUND('',#3345,.T.);
#2210=FACE_OUTER_BOUND('',#3346,.T.);
#2211=FACE_OUTER_BOUND('',#3347,.T.);
#2212=FACE_OUTER_BOUND('',#3348,.T.);
#2213=FACE_OUTER_BOUND('',#3349,.T.);
#2214=FACE_OUTER_BOUND('',#3351,.T.);
#2215=FACE_OUTER_BOUND('',#3353,.T.);
#2216=FACE_OUTER_BOUND('',#3354,.T.);
#2217=FACE_OUTER_BOUND('',#3355,.T.);
#2218=FACE_OUTER_BOUND('',#3356,.T.);
#2219=FACE_OUTER_BOUND('',#3357,.T.);
#2220=FACE_OUTER_BOUND('',#3358,.T.);
#2221=FACE_OUTER_BOUND('',#3359,.T.);
#2222=FACE_OUTER_BOUND('',#3360,.T.);
#2223=FACE_OUTER_BOUND('',#3361,.T.);
#2224=FACE_OUTER_BOUND('',#3362,.T.);
#2225=FACE_OUTER_BOUND('',#3363,.T.);
#2226=FACE_OUTER_BOUND('',#3364,.T.);
#2227=FACE_OUTER_BOUND('',#3365,.T.);
#2228=FACE_OUTER_BOUND('',#3366,.T.);
#2229=FACE_OUTER_BOUND('',#3367,.T.);
#2230=FACE_OUTER_BOUND('',#3368,.T.);
#2231=FACE_OUTER_BOUND('',#3369,.T.);
#2232=FACE_OUTER_BOUND('',#3370,.T.);
#2233=FACE_OUTER_BOUND('',#3371,.T.);
#2234=FACE_OUTER_BOUND('',#3372,.T.);
#2235=FACE_OUTER_BOUND('',#3373,.T.);
#2236=FACE_OUTER_BOUND('',#3374,.T.);
#2237=FACE_OUTER_BOUND('',#3375,.T.);
#2238=FACE_OUTER_BOUND('',#3376,.T.);
#2239=FACE_OUTER_BOUND('',#3377,.T.);
#2240=FACE_OUTER_BOUND('',#3378,.T.);
#2241=FACE_OUTER_BOUND('',#3379,.T.);
#2242=FACE_OUTER_BOUND('',#3380,.T.);
#2243=FACE_OUTER_BOUND('',#3381,.T.);
#2244=FACE_OUTER_BOUND('',#3382,.T.);
#2245=FACE_OUTER_BOUND('',#3383,.T.);
#2246=FACE_OUTER_BOUND('',#3384,.T.);
#2247=FACE_OUTER_BOUND('',#3385,.T.);
#2248=FACE_OUTER_BOUND('',#3386,.T.);
#2249=FACE_OUTER_BOUND('',#3387,.T.);
#2250=FACE_OUTER_BOUND('',#3388,.T.);
#2251=EDGE_LOOP('',(#12651,#12652,#12653,#12654,#12655,#12656,#12657,#12658,
#12659,#12660,#12661,#12662,#12663,#12664,#12665,#12666,#12667,#12668,#12669,
#12670,#12671,#12672,#12673,#12674,#12675,#12676,#12677,#12678,#12679,#12680,
#12681,#12682,#12683,#12684,#12685,#12686));
#2252=EDGE_LOOP('',(#12687,#12688,#12689,#12690));
#2253=EDGE_LOOP('',(#12691,#12692,#12693,#12694));
#2254=EDGE_LOOP('',(#12695,#12696,#12697,#12698));
#2255=EDGE_LOOP('',(#12699,#12700,#12701,#12702));
#2256=EDGE_LOOP('',(#12703,#12704,#12705,#12706));
#2257=EDGE_LOOP('',(#12707,#12708,#12709,#12710));
#2258=EDGE_LOOP('',(#12711,#12712,#12713,#12714));
#2259=EDGE_LOOP('',(#12715,#12716,#12717,#12718));
#2260=EDGE_LOOP('',(#12719,#12720,#12721,#12722));
#2261=EDGE_LOOP('',(#12723,#12724,#12725,#12726));
#2262=EDGE_LOOP('',(#12727,#12728,#12729,#12730));
#2263=EDGE_LOOP('',(#12731,#12732,#12733,#12734));
#2264=EDGE_LOOP('',(#12735,#12736,#12737,#12738));
#2265=EDGE_LOOP('',(#12739,#12740,#12741,#12742));
#2266=EDGE_LOOP('',(#12743,#12744,#12745,#12746));
#2267=EDGE_LOOP('',(#12747,#12748,#12749,#12750));
#2268=EDGE_LOOP('',(#12751,#12752,#12753,#12754));
#2269=EDGE_LOOP('',(#12755,#12756,#12757,#12758));
#2270=EDGE_LOOP('',(#12759,#12760,#12761,#12762));
#2271=EDGE_LOOP('',(#12763,#12764,#12765,#12766));
#2272=EDGE_LOOP('',(#12767,#12768,#12769,#12770));
#2273=EDGE_LOOP('',(#12771,#12772,#12773,#12774));
#2274=EDGE_LOOP('',(#12775,#12776,#12777,#12778));
#2275=EDGE_LOOP('',(#12779,#12780,#12781,#12782));
#2276=EDGE_LOOP('',(#12783,#12784,#12785,#12786));
#2277=EDGE_LOOP('',(#12787,#12788,#12789,#12790));
#2278=EDGE_LOOP('',(#12791,#12792,#12793,#12794));
#2279=EDGE_LOOP('',(#12795,#12796,#12797,#12798));
#2280=EDGE_LOOP('',(#12799,#12800,#12801,#12802));
#2281=EDGE_LOOP('',(#12803,#12804,#12805,#12806));
#2282=EDGE_LOOP('',(#12807,#12808,#12809,#12810));
#2283=EDGE_LOOP('',(#12811,#12812,#12813,#12814));
#2284=EDGE_LOOP('',(#12815,#12816,#12817,#12818));
#2285=EDGE_LOOP('',(#12819,#12820,#12821,#12822));
#2286=EDGE_LOOP('',(#12823,#12824,#12825,#12826));
#2287=EDGE_LOOP('',(#12827,#12828,#12829,#12830));
#2288=EDGE_LOOP('',(#12831,#12832,#12833,#12834,#12835,#12836,#12837,#12838,
#12839,#12840,#12841,#12842,#12843,#12844,#12845,#12846,#12847,#12848,#12849,
#12850,#12851,#12852,#12853,#12854,#12855,#12856,#12857,#12858,#12859,#12860,
#12861,#12862,#12863,#12864,#12865,#12866));
#2289=EDGE_LOOP('',(#12867,#12868,#12869,#12870));
#2290=EDGE_LOOP('',(#12871,#12872,#12873,#12874));
#2291=EDGE_LOOP('',(#12875,#12876,#12877,#12878));
#2292=EDGE_LOOP('',(#12879,#12880,#12881,#12882));
#2293=EDGE_LOOP('',(#12883,#12884,#12885,#12886));
#2294=EDGE_LOOP('',(#12887,#12888,#12889,#12890));
#2295=EDGE_LOOP('',(#12891,#12892,#12893,#12894));
#2296=EDGE_LOOP('',(#12895,#12896,#12897,#12898,#12899,#12900,#12901,#12902,
#12903,#12904,#12905,#12906,#12907,#12908,#12909,#12910,#12911,#12912,#12913,
#12914,#12915,#12916,#12917,#12918,#12919,#12920,#12921,#12922,#12923,#12924,
#12925,#12926,#12927,#12928,#12929,#12930,#12931,#12932,#12933,#12934,#12935,
#12936,#12937,#12938));
#2297=EDGE_LOOP('',(#12939,#12940,#12941,#12942));
#2298=EDGE_LOOP('',(#12943,#12944,#12945,#12946));
#2299=EDGE_LOOP('',(#12947,#12948,#12949,#12950));
#2300=EDGE_LOOP('',(#12951,#12952,#12953,#12954));
#2301=EDGE_LOOP('',(#12955));
#2302=EDGE_LOOP('',(#12956));
#2303=EDGE_LOOP('',(#12957,#12958,#12959,#12960));
#2304=EDGE_LOOP('',(#12961,#12962,#12963,#12964));
#2305=EDGE_LOOP('',(#12965,#12966,#12967,#12968,#12969,#12970,#12971,#12972,
#12973,#12974,#12975,#12976,#12977,#12978,#12979,#12980,#12981,#12982,#12983,
#12984,#12985,#12986,#12987,#12988,#12989,#12990,#12991,#12992,#12993,#12994,
#12995,#12996,#12997,#12998,#12999,#13000,#13001,#13002,#13003,#13004,#13005,
#13006,#13007,#13008));
#2306=EDGE_LOOP('',(#13009,#13010,#13011,#13012));
#2307=EDGE_LOOP('',(#13013,#13014,#13015,#13016));
#2308=EDGE_LOOP('',(#13017,#13018,#13019,#13020));
#2309=EDGE_LOOP('',(#13021,#13022,#13023,#13024));
#2310=EDGE_LOOP('',(#13025));
#2311=EDGE_LOOP('',(#13026));
#2312=EDGE_LOOP('',(#13027,#13028,#13029,#13030));
#2313=EDGE_LOOP('',(#13031,#13032,#13033,#13034));
#2314=EDGE_LOOP('',(#13035,#13036,#13037,#13038));
#2315=EDGE_LOOP('',(#13039,#13040,#13041,#13042));
#2316=EDGE_LOOP('',(#13043,#13044,#13045,#13046));
#2317=EDGE_LOOP('',(#13047,#13048,#13049,#13050));
#2318=EDGE_LOOP('',(#13051,#13052,#13053,#13054));
#2319=EDGE_LOOP('',(#13055,#13056,#13057,#13058));
#2320=EDGE_LOOP('',(#13059));
#2321=EDGE_LOOP('',(#13060));
#2322=EDGE_LOOP('',(#13061,#13062,#13063,#13064));
#2323=EDGE_LOOP('',(#13065,#13066,#13067,#13068));
#2324=EDGE_LOOP('',(#13069,#13070,#13071,#13072));
#2325=EDGE_LOOP('',(#13073,#13074,#13075,#13076));
#2326=EDGE_LOOP('',(#13077,#13078,#13079,#13080));
#2327=EDGE_LOOP('',(#13081,#13082,#13083,#13084));
#2328=EDGE_LOOP('',(#13085,#13086,#13087,#13088));
#2329=EDGE_LOOP('',(#13089,#13090,#13091,#13092));
#2330=EDGE_LOOP('',(#13093,#13094,#13095,#13096));
#2331=EDGE_LOOP('',(#13097));
#2332=EDGE_LOOP('',(#13098));
#2333=EDGE_LOOP('',(#13099,#13100,#13101,#13102));
#2334=EDGE_LOOP('',(#13103,#13104,#13105,#13106));
#2335=EDGE_LOOP('',(#13107,#13108,#13109,#13110));
#2336=EDGE_LOOP('',(#13111,#13112,#13113,#13114));
#2337=EDGE_LOOP('',(#13115,#13116,#13117,#13118));
#2338=EDGE_LOOP('',(#13119,#13120,#13121,#13122));
#2339=EDGE_LOOP('',(#13123,#13124,#13125,#13126));
#2340=EDGE_LOOP('',(#13127,#13128,#13129,#13130));
#2341=EDGE_LOOP('',(#13131,#13132,#13133,#13134));
#2342=EDGE_LOOP('',(#13135,#13136,#13137,#13138));
#2343=EDGE_LOOP('',(#13139,#13140,#13141,#13142));
#2344=EDGE_LOOP('',(#13143,#13144,#13145,#13146));
#2345=EDGE_LOOP('',(#13147,#13148,#13149,#13150));
#2346=EDGE_LOOP('',(#13151,#13152,#13153,#13154));
#2347=EDGE_LOOP('',(#13155,#13156,#13157,#13158));
#2348=EDGE_LOOP('',(#13159,#13160,#13161,#13162));
#2349=EDGE_LOOP('',(#13163,#13164,#13165,#13166));
#2350=EDGE_LOOP('',(#13167,#13168,#13169,#13170));
#2351=EDGE_LOOP('',(#13171,#13172,#13173,#13174));
#2352=EDGE_LOOP('',(#13175,#13176,#13177,#13178));
#2353=EDGE_LOOP('',(#13179,#13180,#13181,#13182));
#2354=EDGE_LOOP('',(#13183,#13184,#13185,#13186));
#2355=EDGE_LOOP('',(#13187,#13188,#13189,#13190));
#2356=EDGE_LOOP('',(#13191,#13192,#13193,#13194));
#2357=EDGE_LOOP('',(#13195,#13196,#13197,#13198));
#2358=EDGE_LOOP('',(#13199,#13200,#13201,#13202));
#2359=EDGE_LOOP('',(#13203,#13204,#13205,#13206));
#2360=EDGE_LOOP('',(#13207,#13208,#13209,#13210));
#2361=EDGE_LOOP('',(#13211,#13212,#13213,#13214));
#2362=EDGE_LOOP('',(#13215,#13216,#13217,#13218));
#2363=EDGE_LOOP('',(#13219,#13220,#13221,#13222,#13223,#13224,#13225,#13226,
#13227,#13228,#13229,#13230,#13231,#13232,#13233,#13234,#13235,#13236,#13237,
#13238,#13239,#13240,#13241,#13242,#13243,#13244,#13245,#13246,#13247,#13248,
#13249,#13250,#13251,#13252,#13253,#13254));
#2364=EDGE_LOOP('',(#13255,#13256,#13257,#13258));
#2365=EDGE_LOOP('',(#13259,#13260,#13261,#13262));
#2366=EDGE_LOOP('',(#13263,#13264,#13265,#13266));
#2367=EDGE_LOOP('',(#13267,#13268,#13269,#13270));
#2368=EDGE_LOOP('',(#13271,#13272,#13273,#13274));
#2369=EDGE_LOOP('',(#13275,#13276,#13277,#13278));
#2370=EDGE_LOOP('',(#13279,#13280,#13281,#13282));
#2371=EDGE_LOOP('',(#13283,#13284,#13285,#13286));
#2372=EDGE_LOOP('',(#13287,#13288,#13289,#13290));
#2373=EDGE_LOOP('',(#13291,#13292,#13293,#13294));
#2374=EDGE_LOOP('',(#13295,#13296,#13297,#13298));
#2375=EDGE_LOOP('',(#13299,#13300,#13301,#13302));
#2376=EDGE_LOOP('',(#13303,#13304,#13305,#13306));
#2377=EDGE_LOOP('',(#13307,#13308,#13309,#13310));
#2378=EDGE_LOOP('',(#13311,#13312,#13313,#13314));
#2379=EDGE_LOOP('',(#13315,#13316,#13317,#13318));
#2380=EDGE_LOOP('',(#13319,#13320,#13321,#13322));
#2381=EDGE_LOOP('',(#13323,#13324,#13325,#13326));
#2382=EDGE_LOOP('',(#13327,#13328,#13329,#13330));
#2383=EDGE_LOOP('',(#13331,#13332,#13333,#13334));
#2384=EDGE_LOOP('',(#13335,#13336,#13337,#13338,#13339,#13340,#13341,#13342,
#13343,#13344,#13345,#13346,#13347,#13348,#13349,#13350,#13351,#13352,#13353,
#13354,#13355,#13356,#13357,#13358,#13359,#13360,#13361,#13362,#13363,#13364,
#13365,#13366,#13367,#13368,#13369,#13370));
#2385=EDGE_LOOP('',(#13371,#13372,#13373,#13374,#13375,#13376,#13377,#13378,
#13379,#13380,#13381,#13382,#13383,#13384,#13385,#13386,#13387,#13388,#13389,
#13390,#13391,#13392,#13393,#13394,#13395,#13396,#13397,#13398,#13399,#13400,
#13401,#13402,#13403,#13404,#13405,#13406));
#2386=EDGE_LOOP('',(#13407,#13408,#13409,#13410));
#2387=EDGE_LOOP('',(#13411,#13412,#13413,#13414));
#2388=EDGE_LOOP('',(#13415,#13416,#13417,#13418));
#2389=EDGE_LOOP('',(#13419,#13420,#13421,#13422));
#2390=EDGE_LOOP('',(#13423,#13424,#13425,#13426));
#2391=EDGE_LOOP('',(#13427,#13428,#13429,#13430));
#2392=EDGE_LOOP('',(#13431,#13432,#13433,#13434));
#2393=EDGE_LOOP('',(#13435,#13436,#13437,#13438));
#2394=EDGE_LOOP('',(#13439,#13440,#13441,#13442));
#2395=EDGE_LOOP('',(#13443,#13444,#13445,#13446));
#2396=EDGE_LOOP('',(#13447,#13448,#13449,#13450));
#2397=EDGE_LOOP('',(#13451,#13452,#13453,#13454));
#2398=EDGE_LOOP('',(#13455,#13456,#13457,#13458));
#2399=EDGE_LOOP('',(#13459,#13460,#13461,#13462));
#2400=EDGE_LOOP('',(#13463,#13464,#13465,#13466));
#2401=EDGE_LOOP('',(#13467,#13468,#13469,#13470));
#2402=EDGE_LOOP('',(#13471,#13472,#13473,#13474));
#2403=EDGE_LOOP('',(#13475,#13476,#13477,#13478));
#2404=EDGE_LOOP('',(#13479,#13480,#13481,#13482));
#2405=EDGE_LOOP('',(#13483,#13484,#13485,#13486));
#2406=EDGE_LOOP('',(#13487,#13488,#13489,#13490));
#2407=EDGE_LOOP('',(#13491,#13492,#13493,#13494));
#2408=EDGE_LOOP('',(#13495,#13496,#13497,#13498));
#2409=EDGE_LOOP('',(#13499,#13500,#13501,#13502));
#2410=EDGE_LOOP('',(#13503,#13504,#13505,#13506));
#2411=EDGE_LOOP('',(#13507,#13508,#13509,#13510));
#2412=EDGE_LOOP('',(#13511,#13512,#13513,#13514));
#2413=EDGE_LOOP('',(#13515,#13516,#13517,#13518));
#2414=EDGE_LOOP('',(#13519,#13520,#13521,#13522));
#2415=EDGE_LOOP('',(#13523,#13524,#13525,#13526));
#2416=EDGE_LOOP('',(#13527,#13528,#13529,#13530));
#2417=EDGE_LOOP('',(#13531,#13532,#13533,#13534));
#2418=EDGE_LOOP('',(#13535,#13536,#13537,#13538));
#2419=EDGE_LOOP('',(#13539,#13540,#13541,#13542));
#2420=EDGE_LOOP('',(#13543,#13544,#13545,#13546));
#2421=EDGE_LOOP('',(#13547,#13548,#13549,#13550));
#2422=EDGE_LOOP('',(#13551,#13552,#13553,#13554,#13555,#13556,#13557,#13558,
#13559,#13560,#13561,#13562,#13563,#13564,#13565,#13566,#13567,#13568,#13569,
#13570,#13571,#13572,#13573,#13574,#13575,#13576,#13577,#13578,#13579,#13580,
#13581,#13582,#13583,#13584,#13585,#13586));
#2423=EDGE_LOOP('',(#13587,#13588,#13589,#13590));
#2424=EDGE_LOOP('',(#13591,#13592,#13593,#13594));
#2425=EDGE_LOOP('',(#13595,#13596,#13597,#13598));
#2426=EDGE_LOOP('',(#13599,#13600,#13601,#13602));
#2427=EDGE_LOOP('',(#13603,#13604,#13605,#13606));
#2428=EDGE_LOOP('',(#13607,#13608,#13609,#13610));
#2429=EDGE_LOOP('',(#13611,#13612,#13613,#13614));
#2430=EDGE_LOOP('',(#13615,#13616,#13617,#13618,#13619,#13620,#13621,#13622,
#13623,#13624,#13625,#13626,#13627,#13628,#13629,#13630,#13631,#13632,#13633,
#13634,#13635,#13636,#13637,#13638,#13639,#13640,#13641,#13642,#13643,#13644,
#13645,#13646,#13647,#13648,#13649,#13650,#13651,#13652,#13653,#13654,#13655,
#13656,#13657,#13658));
#2431=EDGE_LOOP('',(#13659,#13660,#13661,#13662));
#2432=EDGE_LOOP('',(#13663,#13664,#13665,#13666));
#2433=EDGE_LOOP('',(#13667,#13668,#13669,#13670));
#2434=EDGE_LOOP('',(#13671,#13672,#13673,#13674));
#2435=EDGE_LOOP('',(#13675));
#2436=EDGE_LOOP('',(#13676));
#2437=EDGE_LOOP('',(#13677,#13678,#13679,#13680));
#2438=EDGE_LOOP('',(#13681,#13682,#13683,#13684));
#2439=EDGE_LOOP('',(#13685,#13686,#13687,#13688,#13689,#13690,#13691,#13692,
#13693,#13694,#13695,#13696,#13697,#13698,#13699,#13700,#13701,#13702,#13703,
#13704,#13705,#13706,#13707,#13708,#13709,#13710,#13711,#13712,#13713,#13714,
#13715,#13716,#13717,#13718,#13719,#13720,#13721,#13722,#13723,#13724,#13725,
#13726,#13727,#13728));
#2440=EDGE_LOOP('',(#13729,#13730,#13731,#13732));
#2441=EDGE_LOOP('',(#13733,#13734,#13735,#13736));
#2442=EDGE_LOOP('',(#13737,#13738,#13739,#13740));
#2443=EDGE_LOOP('',(#13741,#13742,#13743,#13744));
#2444=EDGE_LOOP('',(#13745));
#2445=EDGE_LOOP('',(#13746));
#2446=EDGE_LOOP('',(#13747,#13748,#13749,#13750));
#2447=EDGE_LOOP('',(#13751,#13752,#13753,#13754));
#2448=EDGE_LOOP('',(#13755,#13756,#13757,#13758));
#2449=EDGE_LOOP('',(#13759,#13760,#13761,#13762));
#2450=EDGE_LOOP('',(#13763,#13764,#13765,#13766));
#2451=EDGE_LOOP('',(#13767,#13768,#13769,#13770));
#2452=EDGE_LOOP('',(#13771,#13772,#13773,#13774));
#2453=EDGE_LOOP('',(#13775,#13776,#13777,#13778));
#2454=EDGE_LOOP('',(#13779));
#2455=EDGE_LOOP('',(#13780));
#2456=EDGE_LOOP('',(#13781,#13782,#13783,#13784));
#2457=EDGE_LOOP('',(#13785,#13786,#13787,#13788));
#2458=EDGE_LOOP('',(#13789,#13790,#13791,#13792));
#2459=EDGE_LOOP('',(#13793,#13794,#13795,#13796));
#2460=EDGE_LOOP('',(#13797,#13798,#13799,#13800));
#2461=EDGE_LOOP('',(#13801,#13802,#13803,#13804));
#2462=EDGE_LOOP('',(#13805,#13806,#13807,#13808));
#2463=EDGE_LOOP('',(#13809,#13810,#13811,#13812));
#2464=EDGE_LOOP('',(#13813,#13814,#13815,#13816));
#2465=EDGE_LOOP('',(#13817));
#2466=EDGE_LOOP('',(#13818));
#2467=EDGE_LOOP('',(#13819,#13820,#13821,#13822));
#2468=EDGE_LOOP('',(#13823,#13824,#13825,#13826));
#2469=EDGE_LOOP('',(#13827,#13828,#13829,#13830));
#2470=EDGE_LOOP('',(#13831,#13832,#13833,#13834));
#2471=EDGE_LOOP('',(#13835,#13836,#13837,#13838));
#2472=EDGE_LOOP('',(#13839,#13840,#13841,#13842));
#2473=EDGE_LOOP('',(#13843,#13844,#13845,#13846));
#2474=EDGE_LOOP('',(#13847,#13848,#13849,#13850));
#2475=EDGE_LOOP('',(#13851,#13852,#13853,#13854));
#2476=EDGE_LOOP('',(#13855,#13856,#13857,#13858));
#2477=EDGE_LOOP('',(#13859,#13860,#13861,#13862));
#2478=EDGE_LOOP('',(#13863,#13864,#13865,#13866));
#2479=EDGE_LOOP('',(#13867,#13868,#13869,#13870));
#2480=EDGE_LOOP('',(#13871,#13872,#13873,#13874));
#2481=EDGE_LOOP('',(#13875,#13876,#13877,#13878));
#2482=EDGE_LOOP('',(#13879,#13880,#13881,#13882));
#2483=EDGE_LOOP('',(#13883,#13884,#13885,#13886));
#2484=EDGE_LOOP('',(#13887,#13888,#13889,#13890));
#2485=EDGE_LOOP('',(#13891,#13892,#13893,#13894));
#2486=EDGE_LOOP('',(#13895,#13896,#13897,#13898));
#2487=EDGE_LOOP('',(#13899,#13900,#13901,#13902));
#2488=EDGE_LOOP('',(#13903,#13904,#13905,#13906));
#2489=EDGE_LOOP('',(#13907,#13908,#13909,#13910));
#2490=EDGE_LOOP('',(#13911,#13912,#13913,#13914));
#2491=EDGE_LOOP('',(#13915,#13916,#13917,#13918));
#2492=EDGE_LOOP('',(#13919,#13920,#13921,#13922));
#2493=EDGE_LOOP('',(#13923,#13924,#13925,#13926));
#2494=EDGE_LOOP('',(#13927,#13928,#13929,#13930));
#2495=EDGE_LOOP('',(#13931,#13932,#13933,#13934));
#2496=EDGE_LOOP('',(#13935,#13936,#13937,#13938));
#2497=EDGE_LOOP('',(#13939,#13940,#13941,#13942,#13943,#13944,#13945,#13946,
#13947,#13948,#13949,#13950,#13951,#13952,#13953,#13954,#13955,#13956,#13957,
#13958,#13959,#13960,#13961,#13962,#13963,#13964,#13965,#13966,#13967,#13968,
#13969,#13970,#13971,#13972,#13973,#13974));
#2498=EDGE_LOOP('',(#13975,#13976,#13977,#13978));
#2499=EDGE_LOOP('',(#13979,#13980,#13981,#13982));
#2500=EDGE_LOOP('',(#13983,#13984,#13985,#13986));
#2501=EDGE_LOOP('',(#13987,#13988,#13989,#13990));
#2502=EDGE_LOOP('',(#13991,#13992,#13993,#13994));
#2503=EDGE_LOOP('',(#13995,#13996,#13997,#13998));
#2504=EDGE_LOOP('',(#13999,#14000,#14001,#14002));
#2505=EDGE_LOOP('',(#14003,#14004,#14005,#14006));
#2506=EDGE_LOOP('',(#14007,#14008,#14009,#14010));
#2507=EDGE_LOOP('',(#14011,#14012,#14013,#14014));
#2508=EDGE_LOOP('',(#14015,#14016,#14017,#14018));
#2509=EDGE_LOOP('',(#14019,#14020,#14021,#14022));
#2510=EDGE_LOOP('',(#14023,#14024,#14025,#14026));
#2511=EDGE_LOOP('',(#14027,#14028,#14029,#14030));
#2512=EDGE_LOOP('',(#14031,#14032,#14033,#14034));
#2513=EDGE_LOOP('',(#14035,#14036,#14037,#14038));
#2514=EDGE_LOOP('',(#14039,#14040,#14041,#14042));
#2515=EDGE_LOOP('',(#14043,#14044,#14045,#14046));
#2516=EDGE_LOOP('',(#14047,#14048,#14049,#14050));
#2517=EDGE_LOOP('',(#14051,#14052,#14053,#14054));
#2518=EDGE_LOOP('',(#14055,#14056,#14057,#14058,#14059,#14060,#14061,#14062,
#14063,#14064,#14065,#14066,#14067,#14068,#14069,#14070,#14071,#14072,#14073,
#14074,#14075,#14076,#14077,#14078,#14079,#14080,#14081,#14082,#14083,#14084,
#14085,#14086,#14087,#14088,#14089,#14090));
#2519=EDGE_LOOP('',(#14091,#14092,#14093,#14094));
#2520=EDGE_LOOP('',(#14095,#14096,#14097,#14098));
#2521=EDGE_LOOP('',(#14099,#14100,#14101,#14102));
#2522=EDGE_LOOP('',(#14103,#14104,#14105,#14106));
#2523=EDGE_LOOP('',(#14107,#14108,#14109,#14110,#14111,#14112,#14113,#14114,
#14115,#14116,#14117,#14118,#14119,#14120,#14121,#14122,#14123,#14124,#14125,
#14126));
#2524=EDGE_LOOP('',(#14127,#14128,#14129,#14130));
#2525=EDGE_LOOP('',(#14131,#14132,#14133,#14134));
#2526=EDGE_LOOP('',(#14135,#14136,#14137,#14138,#14139,#14140,#14141,#14142,
#14143,#14144,#14145,#14146,#14147,#14148,#14149,#14150,#14151,#14152,#14153,
#14154,#14155,#14156,#14157,#14158,#14159,#14160,#14161,#14162,#14163,#14164,
#14165,#14166,#14167,#14168,#14169,#14170));
#2527=EDGE_LOOP('',(#14171,#14172,#14173,#14174));
#2528=EDGE_LOOP('',(#14175,#14176,#14177,#14178));
#2529=EDGE_LOOP('',(#14179,#14180,#14181,#14182));
#2530=EDGE_LOOP('',(#14183,#14184,#14185,#14186));
#2531=EDGE_LOOP('',(#14187,#14188,#14189,#14190));
#2532=EDGE_LOOP('',(#14191,#14192,#14193,#14194));
#2533=EDGE_LOOP('',(#14195,#14196,#14197,#14198));
#2534=EDGE_LOOP('',(#14199,#14200,#14201,#14202));
#2535=EDGE_LOOP('',(#14203,#14204,#14205,#14206));
#2536=EDGE_LOOP('',(#14207,#14208,#14209,#14210));
#2537=EDGE_LOOP('',(#14211,#14212,#14213,#14214));
#2538=EDGE_LOOP('',(#14215,#14216,#14217,#14218));
#2539=EDGE_LOOP('',(#14219,#14220,#14221,#14222));
#2540=EDGE_LOOP('',(#14223,#14224,#14225,#14226));
#2541=EDGE_LOOP('',(#14227,#14228,#14229,#14230));
#2542=EDGE_LOOP('',(#14231,#14232,#14233,#14234));
#2543=EDGE_LOOP('',(#14235,#14236,#14237,#14238));
#2544=EDGE_LOOP('',(#14239,#14240,#14241,#14242));
#2545=EDGE_LOOP('',(#14243,#14244,#14245,#14246));
#2546=EDGE_LOOP('',(#14247,#14248,#14249,#14250));
#2547=EDGE_LOOP('',(#14251,#14252,#14253,#14254));
#2548=EDGE_LOOP('',(#14255,#14256,#14257,#14258));
#2549=EDGE_LOOP('',(#14259,#14260,#14261,#14262));
#2550=EDGE_LOOP('',(#14263,#14264,#14265,#14266));
#2551=EDGE_LOOP('',(#14267));
#2552=EDGE_LOOP('',(#14268));
#2553=EDGE_LOOP('',(#14269));
#2554=EDGE_LOOP('',(#14270));
#2555=EDGE_LOOP('',(#14271,#14272,#14273,#14274,#14275));
#2556=EDGE_LOOP('',(#14276,#14277,#14278,#14279,#14280));
#2557=EDGE_LOOP('',(#14281,#14282,#14283,#14284));
#2558=EDGE_LOOP('',(#14285,#14286,#14287,#14288,#14289));
#2559=EDGE_LOOP('',(#14290,#14291,#14292,#14293,#14294));
#2560=EDGE_LOOP('',(#14295,#14296,#14297,#14298));
#2561=EDGE_LOOP('',(#14299,#14300,#14301,#14302,#14303));
#2562=EDGE_LOOP('',(#14304,#14305,#14306,#14307,#14308));
#2563=EDGE_LOOP('',(#14309,#14310,#14311,#14312));
#2564=EDGE_LOOP('',(#14313,#14314,#14315,#14316,#14317));
#2565=EDGE_LOOP('',(#14318,#14319,#14320,#14321,#14322));
#2566=EDGE_LOOP('',(#14323,#14324,#14325,#14326));
#2567=EDGE_LOOP('',(#14327,#14328,#14329,#14330,#14331));
#2568=EDGE_LOOP('',(#14332,#14333,#14334,#14335,#14336));
#2569=EDGE_LOOP('',(#14337,#14338,#14339,#14340));
#2570=EDGE_LOOP('',(#14341,#14342,#14343,#14344,#14345));
#2571=EDGE_LOOP('',(#14346,#14347,#14348,#14349,#14350));
#2572=EDGE_LOOP('',(#14351,#14352,#14353,#14354));
#2573=EDGE_LOOP('',(#14355,#14356,#14357,#14358,#14359));
#2574=EDGE_LOOP('',(#14360,#14361,#14362,#14363,#14364));
#2575=EDGE_LOOP('',(#14365,#14366,#14367,#14368));
#2576=EDGE_LOOP('',(#14369,#14370,#14371,#14372,#14373));
#2577=EDGE_LOOP('',(#14374,#14375,#14376,#14377,#14378));
#2578=EDGE_LOOP('',(#14379,#14380,#14381,#14382,#14383,#14384));
#2579=EDGE_LOOP('',(#14385,#14386));
#2580=EDGE_LOOP('',(#14387,#14388,#14389,#14390));
#2581=EDGE_LOOP('',(#14391,#14392,#14393,#14394,#14395));
#2582=EDGE_LOOP('',(#14396,#14397,#14398,#14399,#14400,#14401));
#2583=EDGE_LOOP('',(#14402,#14403,#14404,#14405,#14406));
#2584=EDGE_LOOP('',(#14407,#14408,#14409,#14410));
#2585=EDGE_LOOP('',(#14411,#14412,#14413,#14414));
#2586=EDGE_LOOP('',(#14415,#14416,#14417,#14418));
#2587=EDGE_LOOP('',(#14419,#14420,#14421,#14422));
#2588=EDGE_LOOP('',(#14423,#14424,#14425,#14426));
#2589=EDGE_LOOP('',(#14427,#14428,#14429,#14430));
#2590=EDGE_LOOP('',(#14431));
#2591=EDGE_LOOP('',(#14432));
#2592=EDGE_LOOP('',(#14433));
#2593=EDGE_LOOP('',(#14434));
#2594=EDGE_LOOP('',(#14435,#14436,#14437,#14438));
#2595=EDGE_LOOP('',(#14439,#14440,#14441,#14442));
#2596=EDGE_LOOP('',(#14443,#14444,#14445,#14446));
#2597=EDGE_LOOP('',(#14447,#14448,#14449,#14450));
#2598=EDGE_LOOP('',(#14451,#14452,#14453,#14454,#14455));
#2599=EDGE_LOOP('',(#14456,#14457,#14458,#14459,#14460));
#2600=EDGE_LOOP('',(#14461,#14462,#14463,#14464));
#2601=EDGE_LOOP('',(#14465,#14466,#14467,#14468));
#2602=EDGE_LOOP('',(#14469));
#2603=EDGE_LOOP('',(#14470));
#2604=EDGE_LOOP('',(#14471));
#2605=EDGE_LOOP('',(#14472));
#2606=EDGE_LOOP('',(#14473,#14474));
#2607=EDGE_LOOP('',(#14475,#14476));
#2608=EDGE_LOOP('',(#14477,#14478));
#2609=EDGE_LOOP('',(#14479,#14480));
#2610=EDGE_LOOP('',(#14481,#14482));
#2611=EDGE_LOOP('',(#14483,#14484));
#2612=EDGE_LOOP('',(#14485,#14486));
#2613=EDGE_LOOP('',(#14487,#14488,#14489,#14490,#14491,#14492));
#2614=EDGE_LOOP('',(#14493,#14494,#14495,#14496));
#2615=EDGE_LOOP('',(#14497,#14498,#14499,#14500));
#2616=EDGE_LOOP('',(#14501,#14502,#14503,#14504));
#2617=EDGE_LOOP('',(#14505,#14506,#14507,#14508));
#2618=EDGE_LOOP('',(#14509,#14510,#14511,#14512,#14513,#14514,#14515,#14516,
#14517,#14518,#14519,#14520,#14521,#14522,#14523,#14524,#14525,#14526,#14527,
#14528));
#2619=EDGE_LOOP('',(#14529,#14530,#14531,#14532));
#2620=EDGE_LOOP('',(#14533,#14534,#14535,#14536,#14537));
#2621=EDGE_LOOP('',(#14538,#14539,#14540,#14541,#14542,#14543,#14544,#14545,
#14546,#14547,#14548,#14549,#14550,#14551,#14552,#14553,#14554,#14555,#14556,
#14557,#14558,#14559,#14560,#14561,#14562,#14563,#14564,#14565,#14566,#14567,
#14568,#14569,#14570,#14571,#14572,#14573,#14574));
#2622=EDGE_LOOP('',(#14575,#14576,#14577,#14578));
#2623=EDGE_LOOP('',(#14579,#14580,#14581,#14582));
#2624=EDGE_LOOP('',(#14583,#14584,#14585,#14586));
#2625=EDGE_LOOP('',(#14587,#14588,#14589,#14590));
#2626=EDGE_LOOP('',(#14591,#14592,#14593,#14594));
#2627=EDGE_LOOP('',(#14595,#14596,#14597,#14598));
#2628=EDGE_LOOP('',(#14599,#14600,#14601,#14602));
#2629=EDGE_LOOP('',(#14603,#14604,#14605,#14606));
#2630=EDGE_LOOP('',(#14607,#14608,#14609,#14610));
#2631=EDGE_LOOP('',(#14611,#14612,#14613,#14614));
#2632=EDGE_LOOP('',(#14615,#14616,#14617,#14618));
#2633=EDGE_LOOP('',(#14619,#14620,#14621,#14622));
#2634=EDGE_LOOP('',(#14623,#14624,#14625,#14626));
#2635=EDGE_LOOP('',(#14627,#14628,#14629,#14630));
#2636=EDGE_LOOP('',(#14631,#14632,#14633,#14634));
#2637=EDGE_LOOP('',(#14635,#14636,#14637,#14638));
#2638=EDGE_LOOP('',(#14639,#14640,#14641,#14642));
#2639=EDGE_LOOP('',(#14643,#14644,#14645,#14646));
#2640=EDGE_LOOP('',(#14647,#14648,#14649,#14650));
#2641=EDGE_LOOP('',(#14651,#14652,#14653,#14654));
#2642=EDGE_LOOP('',(#14655,#14656,#14657,#14658));
#2643=EDGE_LOOP('',(#14659,#14660,#14661,#14662));
#2644=EDGE_LOOP('',(#14663,#14664,#14665,#14666));
#2645=EDGE_LOOP('',(#14667,#14668,#14669,#14670));
#2646=EDGE_LOOP('',(#14671));
#2647=EDGE_LOOP('',(#14672));
#2648=EDGE_LOOP('',(#14673));
#2649=EDGE_LOOP('',(#14674));
#2650=EDGE_LOOP('',(#14675,#14676,#14677,#14678,#14679));
#2651=EDGE_LOOP('',(#14680,#14681,#14682,#14683,#14684));
#2652=EDGE_LOOP('',(#14685,#14686,#14687,#14688));
#2653=EDGE_LOOP('',(#14689,#14690,#14691,#14692,#14693));
#2654=EDGE_LOOP('',(#14694,#14695,#14696,#14697,#14698));
#2655=EDGE_LOOP('',(#14699,#14700,#14701,#14702));
#2656=EDGE_LOOP('',(#14703,#14704,#14705,#14706,#14707));
#2657=EDGE_LOOP('',(#14708,#14709,#14710,#14711,#14712));
#2658=EDGE_LOOP('',(#14713,#14714,#14715,#14716));
#2659=EDGE_LOOP('',(#14717,#14718,#14719,#14720,#14721));
#2660=EDGE_LOOP('',(#14722,#14723,#14724,#14725,#14726));
#2661=EDGE_LOOP('',(#14727,#14728,#14729,#14730));
#2662=EDGE_LOOP('',(#14731,#14732,#14733,#14734,#14735));
#2663=EDGE_LOOP('',(#14736,#14737,#14738,#14739,#14740));
#2664=EDGE_LOOP('',(#14741,#14742,#14743,#14744));
#2665=EDGE_LOOP('',(#14745,#14746,#14747,#14748,#14749));
#2666=EDGE_LOOP('',(#14750,#14751,#14752,#14753,#14754));
#2667=EDGE_LOOP('',(#14755,#14756,#14757,#14758));
#2668=EDGE_LOOP('',(#14759,#14760,#14761,#14762,#14763));
#2669=EDGE_LOOP('',(#14764,#14765,#14766,#14767,#14768));
#2670=EDGE_LOOP('',(#14769,#14770,#14771,#14772));
#2671=EDGE_LOOP('',(#14773,#14774,#14775,#14776,#14777));
#2672=EDGE_LOOP('',(#14778,#14779,#14780,#14781,#14782));
#2673=EDGE_LOOP('',(#14783,#14784,#14785,#14786,#14787,#14788));
#2674=EDGE_LOOP('',(#14789,#14790,#14791,#14792));
#2675=EDGE_LOOP('',(#14793,#14794,#14795,#14796));
#2676=EDGE_LOOP('',(#14797,#14798,#14799,#14800));
#2677=EDGE_LOOP('',(#14801,#14802,#14803,#14804));
#2678=EDGE_LOOP('',(#14805,#14806,#14807,#14808));
#2679=EDGE_LOOP('',(#14809,#14810,#14811,#14812));
#2680=EDGE_LOOP('',(#14813,#14814,#14815,#14816));
#2681=EDGE_LOOP('',(#14817,#14818,#14819,#14820));
#2682=EDGE_LOOP('',(#14821,#14822,#14823,#14824));
#2683=EDGE_LOOP('',(#14825,#14826,#14827,#14828));
#2684=EDGE_LOOP('',(#14829,#14830,#14831,#14832));
#2685=EDGE_LOOP('',(#14833,#14834,#14835,#14836));
#2686=EDGE_LOOP('',(#14837,#14838,#14839,#14840));
#2687=EDGE_LOOP('',(#14841,#14842,#14843,#14844));
#2688=EDGE_LOOP('',(#14845,#14846,#14847,#14848));
#2689=EDGE_LOOP('',(#14849,#14850,#14851,#14852));
#2690=EDGE_LOOP('',(#14853,#14854,#14855,#14856));
#2691=EDGE_LOOP('',(#14857,#14858,#14859,#14860));
#2692=EDGE_LOOP('',(#14861,#14862,#14863,#14864));
#2693=EDGE_LOOP('',(#14865,#14866,#14867,#14868));
#2694=EDGE_LOOP('',(#14869,#14870,#14871,#14872));
#2695=EDGE_LOOP('',(#14873,#14874,#14875,#14876));
#2696=EDGE_LOOP('',(#14877,#14878,#14879,#14880));
#2697=EDGE_LOOP('',(#14881,#14882,#14883,#14884));
#2698=EDGE_LOOP('',(#14885,#14886,#14887,#14888));
#2699=EDGE_LOOP('',(#14889,#14890,#14891,#14892));
#2700=EDGE_LOOP('',(#14893,#14894,#14895,#14896));
#2701=EDGE_LOOP('',(#14897,#14898,#14899,#14900));
#2702=EDGE_LOOP('',(#14901,#14902,#14903,#14904));
#2703=EDGE_LOOP('',(#14905,#14906,#14907,#14908));
#2704=EDGE_LOOP('',(#14909,#14910,#14911,#14912));
#2705=EDGE_LOOP('',(#14913,#14914,#14915,#14916));
#2706=EDGE_LOOP('',(#14917,#14918,#14919,#14920));
#2707=EDGE_LOOP('',(#14921,#14922,#14923,#14924));
#2708=EDGE_LOOP('',(#14925,#14926,#14927,#14928));
#2709=EDGE_LOOP('',(#14929,#14930,#14931,#14932));
#2710=EDGE_LOOP('',(#14933,#14934,#14935,#14936));
#2711=EDGE_LOOP('',(#14937,#14938,#14939,#14940));
#2712=EDGE_LOOP('',(#14941,#14942,#14943,#14944));
#2713=EDGE_LOOP('',(#14945,#14946,#14947,#14948));
#2714=EDGE_LOOP('',(#14949,#14950,#14951,#14952));
#2715=EDGE_LOOP('',(#14953,#14954,#14955,#14956));
#2716=EDGE_LOOP('',(#14957,#14958,#14959,#14960));
#2717=EDGE_LOOP('',(#14961,#14962,#14963,#14964));
#2718=EDGE_LOOP('',(#14965,#14966,#14967,#14968));
#2719=EDGE_LOOP('',(#14969,#14970,#14971,#14972));
#2720=EDGE_LOOP('',(#14973,#14974,#14975,#14976));
#2721=EDGE_LOOP('',(#14977,#14978,#14979,#14980));
#2722=EDGE_LOOP('',(#14981,#14982,#14983,#14984));
#2723=EDGE_LOOP('',(#14985,#14986,#14987,#14988));
#2724=EDGE_LOOP('',(#14989,#14990,#14991,#14992));
#2725=EDGE_LOOP('',(#14993,#14994,#14995,#14996));
#2726=EDGE_LOOP('',(#14997,#14998,#14999,#15000));
#2727=EDGE_LOOP('',(#15001,#15002,#15003,#15004));
#2728=EDGE_LOOP('',(#15005,#15006,#15007,#15008));
#2729=EDGE_LOOP('',(#15009,#15010,#15011,#15012));
#2730=EDGE_LOOP('',(#15013,#15014,#15015,#15016));
#2731=EDGE_LOOP('',(#15017,#15018,#15019,#15020));
#2732=EDGE_LOOP('',(#15021,#15022,#15023,#15024));
#2733=EDGE_LOOP('',(#15025,#15026,#15027,#15028));
#2734=EDGE_LOOP('',(#15029,#15030,#15031,#15032));
#2735=EDGE_LOOP('',(#15033,#15034,#15035,#15036));
#2736=EDGE_LOOP('',(#15037,#15038,#15039,#15040));
#2737=EDGE_LOOP('',(#15041,#15042,#15043,#15044));
#2738=EDGE_LOOP('',(#15045,#15046,#15047,#15048));
#2739=EDGE_LOOP('',(#15049,#15050,#15051,#15052));
#2740=EDGE_LOOP('',(#15053,#15054,#15055,#15056));
#2741=EDGE_LOOP('',(#15057,#15058,#15059,#15060));
#2742=EDGE_LOOP('',(#15061,#15062,#15063,#15064));
#2743=EDGE_LOOP('',(#15065,#15066,#15067,#15068));
#2744=EDGE_LOOP('',(#15069,#15070,#15071,#15072));
#2745=EDGE_LOOP('',(#15073,#15074,#15075,#15076));
#2746=EDGE_LOOP('',(#15077,#15078,#15079,#15080));
#2747=EDGE_LOOP('',(#15081,#15082,#15083,#15084));
#2748=EDGE_LOOP('',(#15085,#15086,#15087,#15088));
#2749=EDGE_LOOP('',(#15089,#15090,#15091,#15092));
#2750=EDGE_LOOP('',(#15093,#15094,#15095,#15096));
#2751=EDGE_LOOP('',(#15097,#15098,#15099,#15100));
#2752=EDGE_LOOP('',(#15101,#15102,#15103,#15104));
#2753=EDGE_LOOP('',(#15105,#15106,#15107,#15108));
#2754=EDGE_LOOP('',(#15109,#15110,#15111,#15112));
#2755=EDGE_LOOP('',(#15113,#15114,#15115,#15116));
#2756=EDGE_LOOP('',(#15117,#15118,#15119,#15120));
#2757=EDGE_LOOP('',(#15121,#15122,#15123,#15124));
#2758=EDGE_LOOP('',(#15125,#15126,#15127,#15128));
#2759=EDGE_LOOP('',(#15129,#15130,#15131,#15132));
#2760=EDGE_LOOP('',(#15133,#15134,#15135,#15136));
#2761=EDGE_LOOP('',(#15137,#15138,#15139,#15140));
#2762=EDGE_LOOP('',(#15141,#15142,#15143,#15144));
#2763=EDGE_LOOP('',(#15145,#15146,#15147,#15148));
#2764=EDGE_LOOP('',(#15149,#15150,#15151,#15152));
#2765=EDGE_LOOP('',(#15153,#15154,#15155,#15156));
#2766=EDGE_LOOP('',(#15157,#15158,#15159,#15160));
#2767=EDGE_LOOP('',(#15161,#15162,#15163,#15164));
#2768=EDGE_LOOP('',(#15165,#15166,#15167,#15168));
#2769=EDGE_LOOP('',(#15169,#15170,#15171,#15172));
#2770=EDGE_LOOP('',(#15173,#15174,#15175,#15176));
#2771=EDGE_LOOP('',(#15177,#15178,#15179,#15180));
#2772=EDGE_LOOP('',(#15181,#15182,#15183,#15184));
#2773=EDGE_LOOP('',(#15185,#15186,#15187,#15188));
#2774=EDGE_LOOP('',(#15189,#15190,#15191,#15192));
#2775=EDGE_LOOP('',(#15193,#15194,#15195,#15196));
#2776=EDGE_LOOP('',(#15197,#15198,#15199,#15200));
#2777=EDGE_LOOP('',(#15201,#15202,#15203,#15204));
#2778=EDGE_LOOP('',(#15205,#15206,#15207,#15208));
#2779=EDGE_LOOP('',(#15209,#15210,#15211,#15212));
#2780=EDGE_LOOP('',(#15213,#15214,#15215,#15216));
#2781=EDGE_LOOP('',(#15217,#15218,#15219,#15220));
#2782=EDGE_LOOP('',(#15221,#15222,#15223,#15224));
#2783=EDGE_LOOP('',(#15225,#15226,#15227,#15228));
#2784=EDGE_LOOP('',(#15229,#15230,#15231,#15232));
#2785=EDGE_LOOP('',(#15233,#15234,#15235,#15236));
#2786=EDGE_LOOP('',(#15237,#15238,#15239,#15240));
#2787=EDGE_LOOP('',(#15241,#15242,#15243,#15244));
#2788=EDGE_LOOP('',(#15245,#15246,#15247,#15248));
#2789=EDGE_LOOP('',(#15249,#15250,#15251,#15252));
#2790=EDGE_LOOP('',(#15253,#15254,#15255,#15256));
#2791=EDGE_LOOP('',(#15257,#15258,#15259,#15260));
#2792=EDGE_LOOP('',(#15261,#15262,#15263,#15264));
#2793=EDGE_LOOP('',(#15265,#15266,#15267,#15268));
#2794=EDGE_LOOP('',(#15269,#15270,#15271,#15272));
#2795=EDGE_LOOP('',(#15273,#15274,#15275,#15276));
#2796=EDGE_LOOP('',(#15277,#15278,#15279,#15280));
#2797=EDGE_LOOP('',(#15281,#15282,#15283,#15284));
#2798=EDGE_LOOP('',(#15285,#15286,#15287,#15288));
#2799=EDGE_LOOP('',(#15289,#15290,#15291,#15292));
#2800=EDGE_LOOP('',(#15293,#15294,#15295,#15296));
#2801=EDGE_LOOP('',(#15297,#15298,#15299,#15300));
#2802=EDGE_LOOP('',(#15301,#15302,#15303,#15304));
#2803=EDGE_LOOP('',(#15305,#15306,#15307,#15308));
#2804=EDGE_LOOP('',(#15309,#15310,#15311,#15312));
#2805=EDGE_LOOP('',(#15313,#15314,#15315,#15316));
#2806=EDGE_LOOP('',(#15317,#15318,#15319,#15320));
#2807=EDGE_LOOP('',(#15321,#15322,#15323,#15324));
#2808=EDGE_LOOP('',(#15325,#15326,#15327,#15328));
#2809=EDGE_LOOP('',(#15329,#15330,#15331,#15332));
#2810=EDGE_LOOP('',(#15333,#15334,#15335,#15336));
#2811=EDGE_LOOP('',(#15337,#15338,#15339,#15340));
#2812=EDGE_LOOP('',(#15341,#15342,#15343,#15344));
#2813=EDGE_LOOP('',(#15345,#15346,#15347,#15348));
#2814=EDGE_LOOP('',(#15349,#15350,#15351,#15352));
#2815=EDGE_LOOP('',(#15353,#15354,#15355,#15356));
#2816=EDGE_LOOP('',(#15357,#15358,#15359,#15360));
#2817=EDGE_LOOP('',(#15361,#15362,#15363,#15364));
#2818=EDGE_LOOP('',(#15365,#15366,#15367,#15368));
#2819=EDGE_LOOP('',(#15369,#15370,#15371,#15372));
#2820=EDGE_LOOP('',(#15373,#15374,#15375,#15376));
#2821=EDGE_LOOP('',(#15377,#15378,#15379,#15380));
#2822=EDGE_LOOP('',(#15381,#15382,#15383,#15384));
#2823=EDGE_LOOP('',(#15385,#15386,#15387,#15388));
#2824=EDGE_LOOP('',(#15389,#15390,#15391,#15392));
#2825=EDGE_LOOP('',(#15393,#15394,#15395,#15396));
#2826=EDGE_LOOP('',(#15397,#15398,#15399,#15400));
#2827=EDGE_LOOP('',(#15401,#15402,#15403,#15404));
#2828=EDGE_LOOP('',(#15405,#15406,#15407,#15408));
#2829=EDGE_LOOP('',(#15409,#15410,#15411,#15412));
#2830=EDGE_LOOP('',(#15413,#15414,#15415,#15416));
#2831=EDGE_LOOP('',(#15417,#15418,#15419,#15420));
#2832=EDGE_LOOP('',(#15421,#15422,#15423,#15424));
#2833=EDGE_LOOP('',(#15425,#15426,#15427,#15428));
#2834=EDGE_LOOP('',(#15429,#15430,#15431,#15432));
#2835=EDGE_LOOP('',(#15433,#15434,#15435,#15436));
#2836=EDGE_LOOP('',(#15437,#15438,#15439,#15440));
#2837=EDGE_LOOP('',(#15441,#15442,#15443,#15444));
#2838=EDGE_LOOP('',(#15445,#15446,#15447,#15448));
#2839=EDGE_LOOP('',(#15449,#15450,#15451,#15452));
#2840=EDGE_LOOP('',(#15453,#15454,#15455,#15456));
#2841=EDGE_LOOP('',(#15457,#15458,#15459,#15460));
#2842=EDGE_LOOP('',(#15461,#15462,#15463,#15464));
#2843=EDGE_LOOP('',(#15465,#15466,#15467,#15468));
#2844=EDGE_LOOP('',(#15469,#15470,#15471,#15472));
#2845=EDGE_LOOP('',(#15473,#15474,#15475,#15476));
#2846=EDGE_LOOP('',(#15477,#15478,#15479,#15480));
#2847=EDGE_LOOP('',(#15481,#15482,#15483,#15484));
#2848=EDGE_LOOP('',(#15485,#15486,#15487,#15488));
#2849=EDGE_LOOP('',(#15489,#15490,#15491,#15492));
#2850=EDGE_LOOP('',(#15493,#15494,#15495,#15496));
#2851=EDGE_LOOP('',(#15497,#15498,#15499,#15500));
#2852=EDGE_LOOP('',(#15501,#15502,#15503,#15504));
#2853=EDGE_LOOP('',(#15505,#15506,#15507,#15508));
#2854=EDGE_LOOP('',(#15509,#15510,#15511,#15512));
#2855=EDGE_LOOP('',(#15513,#15514,#15515,#15516));
#2856=EDGE_LOOP('',(#15517,#15518,#15519,#15520));
#2857=EDGE_LOOP('',(#15521,#15522,#15523,#15524));
#2858=EDGE_LOOP('',(#15525,#15526,#15527,#15528));
#2859=EDGE_LOOP('',(#15529,#15530,#15531,#15532));
#2860=EDGE_LOOP('',(#15533,#15534,#15535,#15536));
#2861=EDGE_LOOP('',(#15537,#15538,#15539,#15540));
#2862=EDGE_LOOP('',(#15541,#15542,#15543,#15544));
#2863=EDGE_LOOP('',(#15545,#15546,#15547,#15548));
#2864=EDGE_LOOP('',(#15549,#15550,#15551,#15552));
#2865=EDGE_LOOP('',(#15553,#15554,#15555,#15556));
#2866=EDGE_LOOP('',(#15557,#15558,#15559,#15560));
#2867=EDGE_LOOP('',(#15561,#15562,#15563,#15564));
#2868=EDGE_LOOP('',(#15565,#15566,#15567,#15568));
#2869=EDGE_LOOP('',(#15569,#15570,#15571,#15572));
#2870=EDGE_LOOP('',(#15573,#15574,#15575,#15576));
#2871=EDGE_LOOP('',(#15577,#15578,#15579,#15580));
#2872=EDGE_LOOP('',(#15581,#15582,#15583,#15584));
#2873=EDGE_LOOP('',(#15585,#15586,#15587,#15588));
#2874=EDGE_LOOP('',(#15589,#15590,#15591,#15592));
#2875=EDGE_LOOP('',(#15593,#15594,#15595,#15596));
#2876=EDGE_LOOP('',(#15597,#15598,#15599,#15600));
#2877=EDGE_LOOP('',(#15601,#15602,#15603,#15604));
#2878=EDGE_LOOP('',(#15605,#15606,#15607,#15608));
#2879=EDGE_LOOP('',(#15609,#15610,#15611,#15612));
#2880=EDGE_LOOP('',(#15613,#15614,#15615,#15616));
#2881=EDGE_LOOP('',(#15617,#15618,#15619,#15620));
#2882=EDGE_LOOP('',(#15621,#15622,#15623,#15624));
#2883=EDGE_LOOP('',(#15625,#15626,#15627,#15628));
#2884=EDGE_LOOP('',(#15629,#15630,#15631,#15632));
#2885=EDGE_LOOP('',(#15633,#15634,#15635,#15636));
#2886=EDGE_LOOP('',(#15637,#15638,#15639,#15640));
#2887=EDGE_LOOP('',(#15641,#15642,#15643,#15644));
#2888=EDGE_LOOP('',(#15645,#15646,#15647,#15648));
#2889=EDGE_LOOP('',(#15649,#15650,#15651,#15652));
#2890=EDGE_LOOP('',(#15653,#15654,#15655,#15656));
#2891=EDGE_LOOP('',(#15657,#15658,#15659,#15660));
#2892=EDGE_LOOP('',(#15661,#15662,#15663,#15664));
#2893=EDGE_LOOP('',(#15665,#15666,#15667,#15668));
#2894=EDGE_LOOP('',(#15669,#15670,#15671,#15672));
#2895=EDGE_LOOP('',(#15673,#15674,#15675,#15676));
#2896=EDGE_LOOP('',(#15677,#15678,#15679,#15680));
#2897=EDGE_LOOP('',(#15681,#15682,#15683,#15684));
#2898=EDGE_LOOP('',(#15685,#15686,#15687,#15688));
#2899=EDGE_LOOP('',(#15689,#15690,#15691,#15692));
#2900=EDGE_LOOP('',(#15693,#15694,#15695,#15696));
#2901=EDGE_LOOP('',(#15697,#15698,#15699,#15700));
#2902=EDGE_LOOP('',(#15701,#15702,#15703,#15704));
#2903=EDGE_LOOP('',(#15705,#15706,#15707,#15708));
#2904=EDGE_LOOP('',(#15709,#15710,#15711,#15712));
#2905=EDGE_LOOP('',(#15713,#15714,#15715,#15716));
#2906=EDGE_LOOP('',(#15717,#15718,#15719,#15720));
#2907=EDGE_LOOP('',(#15721,#15722,#15723,#15724));
#2908=EDGE_LOOP('',(#15725,#15726,#15727,#15728));
#2909=EDGE_LOOP('',(#15729,#15730,#15731,#15732));
#2910=EDGE_LOOP('',(#15733,#15734,#15735,#15736));
#2911=EDGE_LOOP('',(#15737,#15738,#15739,#15740));
#2912=EDGE_LOOP('',(#15741,#15742,#15743,#15744));
#2913=EDGE_LOOP('',(#15745,#15746,#15747,#15748,#15749,#15750,#15751,#15752,
#15753,#15754,#15755,#15756,#15757,#15758,#15759,#15760,#15761,#15762,#15763,
#15764,#15765,#15766,#15767,#15768,#15769,#15770,#15771,#15772,#15773,#15774,
#15775,#15776,#15777,#15778,#15779,#15780,#15781,#15782,#15783,#15784,#15785,
#15786,#15787,#15788,#15789,#15790,#15791,#15792,#15793,#15794,#15795,#15796,
#15797,#15798,#15799,#15800,#15801,#15802,#15803,#15804,#15805,#15806,#15807,
#15808,#15809,#15810,#15811,#15812,#15813,#15814,#15815,#15816,#15817,#15818,
#15819,#15820,#15821,#15822,#15823,#15824,#15825,#15826,#15827,#15828,#15829,
#15830,#15831,#15832,#15833,#15834,#15835,#15836,#15837,#15838,#15839,#15840,
#15841,#15842,#15843,#15844,#15845,#15846,#15847,#15848,#15849,#15850,#15851,
#15852,#15853,#15854,#15855,#15856,#15857,#15858,#15859,#15860,#15861,#15862,
#15863,#15864,#15865,#15866,#15867,#15868,#15869,#15870,#15871,#15872,#15873,
#15874,#15875,#15876,#15877,#15878,#15879,#15880,#15881,#15882,#15883,#15884,
#15885,#15886,#15887,#15888,#15889,#15890,#15891,#15892,#15893,#15894,#15895,
#15896,#15897,#15898,#15899,#15900,#15901,#15902,#15903,#15904,#15905,#15906,
#15907,#15908,#15909,#15910,#15911,#15912,#15913,#15914,#15915,#15916,#15917,
#15918,#15919,#15920));
#2914=EDGE_LOOP('',(#15921,#15922,#15923,#15924,#15925,#15926,#15927,#15928,
#15929,#15930,#15931,#15932,#15933,#15934,#15935,#15936));
#2915=EDGE_LOOP('',(#15937));
#2916=EDGE_LOOP('',(#15938,#15939,#15940,#15941,#15942,#15943,#15944,#15945));
#2917=EDGE_LOOP('',(#15946,#15947,#15948,#15949,#15950,#15951,#15952,#15953));
#2918=EDGE_LOOP('',(#15954,#15955,#15956,#15957,#15958,#15959,#15960,#15961,
#15962,#15963,#15964,#15965,#15966,#15967,#15968,#15969));
#2919=EDGE_LOOP('',(#15970));
#2920=EDGE_LOOP('',(#15971,#15972,#15973,#15974,#15975,#15976,#15977,#15978,
#15979,#15980,#15981,#15982,#15983,#15984,#15985,#15986));
#2921=EDGE_LOOP('',(#15987));
#2922=EDGE_LOOP('',(#15988,#15989,#15990,#15991,#15992,#15993,#15994,#15995,
#15996,#15997,#15998,#15999,#16000,#16001,#16002,#16003));
#2923=EDGE_LOOP('',(#16004));
#2924=EDGE_LOOP('',(#16005,#16006,#16007,#16008,#16009,#16010,#16011,#16012));
#2925=EDGE_LOOP('',(#16013,#16014,#16015,#16016,#16017,#16018,#16019,#16020));
#2926=EDGE_LOOP('',(#16021));
#2927=EDGE_LOOP('',(#16022,#16023,#16024,#16025));
#2928=EDGE_LOOP('',(#16026,#16027,#16028,#16029));
#2929=EDGE_LOOP('',(#16030,#16031,#16032,#16033));
#2930=EDGE_LOOP('',(#16034,#16035,#16036,#16037));
#2931=EDGE_LOOP('',(#16038,#16039,#16040,#16041));
#2932=EDGE_LOOP('',(#16042,#16043,#16044,#16045));
#2933=EDGE_LOOP('',(#16046,#16047,#16048,#16049));
#2934=EDGE_LOOP('',(#16050,#16051,#16052,#16053));
#2935=EDGE_LOOP('',(#16054,#16055,#16056,#16057));
#2936=EDGE_LOOP('',(#16058,#16059,#16060,#16061));
#2937=EDGE_LOOP('',(#16062,#16063,#16064,#16065));
#2938=EDGE_LOOP('',(#16066,#16067,#16068,#16069));
#2939=EDGE_LOOP('',(#16070,#16071,#16072,#16073));
#2940=EDGE_LOOP('',(#16074,#16075,#16076,#16077));
#2941=EDGE_LOOP('',(#16078,#16079,#16080,#16081));
#2942=EDGE_LOOP('',(#16082,#16083,#16084,#16085));
#2943=EDGE_LOOP('',(#16086,#16087,#16088,#16089));
#2944=EDGE_LOOP('',(#16090,#16091,#16092,#16093));
#2945=EDGE_LOOP('',(#16094,#16095,#16096,#16097));
#2946=EDGE_LOOP('',(#16098,#16099,#16100,#16101));
#2947=EDGE_LOOP('',(#16102,#16103,#16104,#16105));
#2948=EDGE_LOOP('',(#16106,#16107,#16108,#16109));
#2949=EDGE_LOOP('',(#16110,#16111,#16112,#16113));
#2950=EDGE_LOOP('',(#16114,#16115,#16116,#16117));
#2951=EDGE_LOOP('',(#16118,#16119,#16120,#16121));
#2952=EDGE_LOOP('',(#16122,#16123,#16124,#16125));
#2953=EDGE_LOOP('',(#16126,#16127,#16128,#16129));
#2954=EDGE_LOOP('',(#16130,#16131,#16132,#16133));
#2955=EDGE_LOOP('',(#16134,#16135,#16136,#16137));
#2956=EDGE_LOOP('',(#16138,#16139,#16140,#16141));
#2957=EDGE_LOOP('',(#16142,#16143,#16144,#16145));
#2958=EDGE_LOOP('',(#16146,#16147,#16148,#16149));
#2959=EDGE_LOOP('',(#16150,#16151,#16152,#16153));
#2960=EDGE_LOOP('',(#16154,#16155,#16156,#16157));
#2961=EDGE_LOOP('',(#16158,#16159,#16160,#16161));
#2962=EDGE_LOOP('',(#16162,#16163,#16164,#16165));
#2963=EDGE_LOOP('',(#16166,#16167,#16168,#16169));
#2964=EDGE_LOOP('',(#16170,#16171,#16172,#16173));
#2965=EDGE_LOOP('',(#16174,#16175,#16176,#16177,#16178,#16179,#16180,#16181,
#16182,#16183,#16184,#16185,#16186,#16187,#16188,#16189,#16190,#16191,#16192,
#16193,#16194,#16195,#16196,#16197,#16198,#16199,#16200,#16201,#16202,#16203,
#16204,#16205,#16206,#16207,#16208,#16209,#16210,#16211,#16212,#16213,#16214,
#16215,#16216,#16217,#16218,#16219,#16220,#16221,#16222,#16223,#16224,#16225,
#16226,#16227,#16228,#16229,#16230,#16231,#16232,#16233,#16234,#16235,#16236,
#16237,#16238,#16239,#16240,#16241,#16242,#16243,#16244,#16245,#16246,#16247,
#16248,#16249,#16250,#16251,#16252,#16253,#16254,#16255,#16256,#16257,#16258,
#16259,#16260,#16261,#16262,#16263,#16264,#16265,#16266,#16267,#16268,#16269,
#16270,#16271,#16272,#16273,#16274,#16275,#16276,#16277,#16278,#16279,#16280,
#16281,#16282,#16283,#16284,#16285,#16286,#16287,#16288,#16289,#16290,#16291,
#16292,#16293,#16294,#16295,#16296,#16297,#16298,#16299,#16300,#16301,#16302,
#16303,#16304,#16305,#16306,#16307,#16308,#16309,#16310,#16311,#16312,#16313,
#16314,#16315,#16316,#16317,#16318,#16319,#16320,#16321,#16322,#16323,#16324,
#16325,#16326,#16327,#16328,#16329,#16330,#16331,#16332,#16333,#16334,#16335,
#16336,#16337,#16338,#16339,#16340,#16341,#16342,#16343,#16344,#16345,#16346,
#16347,#16348,#16349));
#2966=EDGE_LOOP('',(#16350,#16351,#16352,#16353,#16354,#16355,#16356,#16357));
#2967=EDGE_LOOP('',(#16358,#16359,#16360,#16361,#16362,#16363,#16364,#16365));
#2968=EDGE_LOOP('',(#16366));
#2969=EDGE_LOOP('',(#16367));
#2970=EDGE_LOOP('',(#16368,#16369,#16370,#16371,#16372,#16373,#16374,#16375,
#16376,#16377,#16378,#16379,#16380,#16381,#16382,#16383));
#2971=EDGE_LOOP('',(#16384,#16385,#16386,#16387,#16388,#16389,#16390,#16391,
#16392,#16393,#16394,#16395,#16396,#16397,#16398,#16399));
#2972=EDGE_LOOP('',(#16400));
#2973=EDGE_LOOP('',(#16401,#16402,#16403,#16404,#16405,#16406,#16407,#16408,
#16409,#16410,#16411,#16412,#16413,#16414,#16415,#16416));
#2974=EDGE_LOOP('',(#16417));
#2975=EDGE_LOOP('',(#16418));
#2976=EDGE_LOOP('',(#16419,#16420,#16421,#16422,#16423,#16424,#16425,#16426));
#2977=EDGE_LOOP('',(#16427,#16428,#16429,#16430,#16431,#16432,#16433,#16434));
#2978=EDGE_LOOP('',(#16435,#16436,#16437,#16438,#16439,#16440,#16441,#16442,
#16443,#16444,#16445,#16446,#16447,#16448,#16449,#16450));
#2979=EDGE_LOOP('',(#16451,#16452,#16453,#16454));
#2980=EDGE_LOOP('',(#16455,#16456,#16457,#16458));
#2981=EDGE_LOOP('',(#16459,#16460,#16461,#16462));
#2982=EDGE_LOOP('',(#16463,#16464,#16465,#16466));
#2983=EDGE_LOOP('',(#16467,#16468,#16469,#16470));
#2984=EDGE_LOOP('',(#16471,#16472,#16473,#16474));
#2985=EDGE_LOOP('',(#16475,#16476,#16477,#16478));
#2986=EDGE_LOOP('',(#16479,#16480,#16481,#16482));
#2987=EDGE_LOOP('',(#16483,#16484,#16485,#16486));
#2988=EDGE_LOOP('',(#16487,#16488,#16489,#16490));
#2989=EDGE_LOOP('',(#16491,#16492,#16493,#16494));
#2990=EDGE_LOOP('',(#16495,#16496,#16497,#16498));
#2991=EDGE_LOOP('',(#16499,#16500,#16501,#16502));
#2992=EDGE_LOOP('',(#16503,#16504,#16505,#16506));
#2993=EDGE_LOOP('',(#16507,#16508,#16509,#16510));
#2994=EDGE_LOOP('',(#16511,#16512,#16513,#16514));
#2995=EDGE_LOOP('',(#16515,#16516,#16517,#16518));
#2996=EDGE_LOOP('',(#16519,#16520,#16521,#16522));
#2997=EDGE_LOOP('',(#16523,#16524,#16525,#16526));
#2998=EDGE_LOOP('',(#16527,#16528,#16529,#16530));
#2999=EDGE_LOOP('',(#16531,#16532,#16533,#16534));
#3000=EDGE_LOOP('',(#16535,#16536,#16537,#16538));
#3001=EDGE_LOOP('',(#16539,#16540,#16541,#16542));
#3002=EDGE_LOOP('',(#16543,#16544,#16545,#16546));
#3003=EDGE_LOOP('',(#16547,#16548,#16549,#16550));
#3004=EDGE_LOOP('',(#16551,#16552,#16553,#16554));
#3005=EDGE_LOOP('',(#16555,#16556,#16557,#16558));
#3006=EDGE_LOOP('',(#16559,#16560,#16561,#16562));
#3007=EDGE_LOOP('',(#16563,#16564,#16565,#16566));
#3008=EDGE_LOOP('',(#16567,#16568,#16569,#16570));
#3009=EDGE_LOOP('',(#16571,#16572,#16573,#16574));
#3010=EDGE_LOOP('',(#16575,#16576,#16577,#16578));
#3011=EDGE_LOOP('',(#16579,#16580,#16581,#16582));
#3012=EDGE_LOOP('',(#16583,#16584,#16585,#16586));
#3013=EDGE_LOOP('',(#16587,#16588,#16589,#16590));
#3014=EDGE_LOOP('',(#16591,#16592,#16593,#16594));
#3015=EDGE_LOOP('',(#16595,#16596,#16597,#16598));
#3016=EDGE_LOOP('',(#16599,#16600,#16601,#16602));
#3017=EDGE_LOOP('',(#16603,#16604,#16605,#16606));
#3018=EDGE_LOOP('',(#16607,#16608,#16609,#16610));
#3019=EDGE_LOOP('',(#16611,#16612,#16613,#16614));
#3020=EDGE_LOOP('',(#16615,#16616,#16617,#16618));
#3021=EDGE_LOOP('',(#16619,#16620,#16621,#16622));
#3022=EDGE_LOOP('',(#16623,#16624,#16625,#16626));
#3023=EDGE_LOOP('',(#16627,#16628,#16629,#16630));
#3024=EDGE_LOOP('',(#16631,#16632,#16633,#16634));
#3025=EDGE_LOOP('',(#16635,#16636,#16637,#16638));
#3026=EDGE_LOOP('',(#16639,#16640,#16641,#16642));
#3027=EDGE_LOOP('',(#16643,#16644,#16645,#16646));
#3028=EDGE_LOOP('',(#16647,#16648,#16649,#16650));
#3029=EDGE_LOOP('',(#16651,#16652,#16653,#16654));
#3030=EDGE_LOOP('',(#16655,#16656,#16657,#16658));
#3031=EDGE_LOOP('',(#16659,#16660,#16661,#16662));
#3032=EDGE_LOOP('',(#16663,#16664,#16665,#16666));
#3033=EDGE_LOOP('',(#16667,#16668,#16669,#16670));
#3034=EDGE_LOOP('',(#16671,#16672,#16673,#16674));
#3035=EDGE_LOOP('',(#16675,#16676,#16677,#16678));
#3036=EDGE_LOOP('',(#16679,#16680,#16681,#16682));
#3037=EDGE_LOOP('',(#16683,#16684,#16685,#16686));
#3038=EDGE_LOOP('',(#16687,#16688,#16689,#16690));
#3039=EDGE_LOOP('',(#16691,#16692,#16693,#16694));
#3040=EDGE_LOOP('',(#16695,#16696,#16697,#16698));
#3041=EDGE_LOOP('',(#16699,#16700,#16701,#16702));
#3042=EDGE_LOOP('',(#16703,#16704,#16705,#16706));
#3043=EDGE_LOOP('',(#16707,#16708,#16709,#16710));
#3044=EDGE_LOOP('',(#16711,#16712,#16713,#16714));
#3045=EDGE_LOOP('',(#16715,#16716,#16717,#16718));
#3046=EDGE_LOOP('',(#16719,#16720,#16721,#16722));
#3047=EDGE_LOOP('',(#16723,#16724,#16725,#16726));
#3048=EDGE_LOOP('',(#16727,#16728,#16729,#16730));
#3049=EDGE_LOOP('',(#16731,#16732,#16733,#16734));
#3050=EDGE_LOOP('',(#16735,#16736,#16737,#16738));
#3051=EDGE_LOOP('',(#16739,#16740,#16741,#16742));
#3052=EDGE_LOOP('',(#16743,#16744,#16745,#16746));
#3053=EDGE_LOOP('',(#16747,#16748,#16749,#16750));
#3054=EDGE_LOOP('',(#16751,#16752,#16753,#16754));
#3055=EDGE_LOOP('',(#16755,#16756,#16757,#16758));
#3056=EDGE_LOOP('',(#16759,#16760,#16761,#16762));
#3057=EDGE_LOOP('',(#16763,#16764,#16765,#16766));
#3058=EDGE_LOOP('',(#16767,#16768,#16769,#16770));
#3059=EDGE_LOOP('',(#16771,#16772,#16773,#16774));
#3060=EDGE_LOOP('',(#16775,#16776,#16777,#16778));
#3061=EDGE_LOOP('',(#16779,#16780,#16781,#16782));
#3062=EDGE_LOOP('',(#16783,#16784,#16785,#16786));
#3063=EDGE_LOOP('',(#16787,#16788,#16789,#16790));
#3064=EDGE_LOOP('',(#16791,#16792,#16793,#16794));
#3065=EDGE_LOOP('',(#16795,#16796,#16797,#16798));
#3066=EDGE_LOOP('',(#16799,#16800,#16801,#16802));
#3067=EDGE_LOOP('',(#16803,#16804,#16805,#16806));
#3068=EDGE_LOOP('',(#16807,#16808,#16809,#16810));
#3069=EDGE_LOOP('',(#16811,#16812,#16813,#16814));
#3070=EDGE_LOOP('',(#16815,#16816,#16817,#16818));
#3071=EDGE_LOOP('',(#16819,#16820,#16821,#16822));
#3072=EDGE_LOOP('',(#16823,#16824,#16825,#16826));
#3073=EDGE_LOOP('',(#16827,#16828,#16829,#16830));
#3074=EDGE_LOOP('',(#16831,#16832,#16833,#16834));
#3075=EDGE_LOOP('',(#16835,#16836,#16837,#16838));
#3076=EDGE_LOOP('',(#16839,#16840,#16841,#16842));
#3077=EDGE_LOOP('',(#16843,#16844,#16845,#16846));
#3078=EDGE_LOOP('',(#16847,#16848,#16849,#16850));
#3079=EDGE_LOOP('',(#16851,#16852,#16853,#16854,#16855));
#3080=EDGE_LOOP('',(#16856,#16857,#16858,#16859,#16860,#16861,#16862,#16863));
#3081=EDGE_LOOP('',(#16864,#16865,#16866,#16867));
#3082=EDGE_LOOP('',(#16868,#16869,#16870,#16871));
#3083=EDGE_LOOP('',(#16872,#16873,#16874,#16875));
#3084=EDGE_LOOP('',(#16876,#16877,#16878,#16879));
#3085=EDGE_LOOP('',(#16880,#16881,#16882,#16883));
#3086=EDGE_LOOP('',(#16884,#16885,#16886,#16887));
#3087=EDGE_LOOP('',(#16888,#16889,#16890,#16891));
#3088=EDGE_LOOP('',(#16892,#16893,#16894,#16895));
#3089=EDGE_LOOP('',(#16896,#16897,#16898,#16899,#16900));
#3090=EDGE_LOOP('',(#16901,#16902,#16903,#16904));
#3091=EDGE_LOOP('',(#16905,#16906,#16907,#16908));
#3092=EDGE_LOOP('',(#16909,#16910,#16911,#16912));
#3093=EDGE_LOOP('',(#16913,#16914,#16915,#16916));
#3094=EDGE_LOOP('',(#16917,#16918,#16919,#16920));
#3095=EDGE_LOOP('',(#16921,#16922,#16923,#16924));
#3096=EDGE_LOOP('',(#16925,#16926,#16927,#16928));
#3097=EDGE_LOOP('',(#16929,#16930,#16931,#16932));
#3098=EDGE_LOOP('',(#16933,#16934,#16935,#16936));
#3099=EDGE_LOOP('',(#16937,#16938,#16939,#16940));
#3100=EDGE_LOOP('',(#16941,#16942,#16943,#16944));
#3101=EDGE_LOOP('',(#16945,#16946,#16947,#16948));
#3102=EDGE_LOOP('',(#16949,#16950,#16951,#16952));
#3103=EDGE_LOOP('',(#16953,#16954,#16955,#16956));
#3104=EDGE_LOOP('',(#16957,#16958,#16959,#16960));
#3105=EDGE_LOOP('',(#16961,#16962,#16963,#16964));
#3106=EDGE_LOOP('',(#16965,#16966,#16967,#16968));
#3107=EDGE_LOOP('',(#16969,#16970,#16971,#16972));
#3108=EDGE_LOOP('',(#16973,#16974,#16975,#16976));
#3109=EDGE_LOOP('',(#16977,#16978,#16979,#16980));
#3110=EDGE_LOOP('',(#16981,#16982,#16983,#16984));
#3111=EDGE_LOOP('',(#16985,#16986,#16987,#16988));
#3112=EDGE_LOOP('',(#16989,#16990,#16991,#16992));
#3113=EDGE_LOOP('',(#16993,#16994,#16995,#16996));
#3114=EDGE_LOOP('',(#16997,#16998,#16999,#17000));
#3115=EDGE_LOOP('',(#17001,#17002,#17003,#17004));
#3116=EDGE_LOOP('',(#17005,#17006,#17007,#17008));
#3117=EDGE_LOOP('',(#17009,#17010,#17011,#17012));
#3118=EDGE_LOOP('',(#17013,#17014,#17015,#17016));
#3119=EDGE_LOOP('',(#17017,#17018,#17019,#17020));
#3120=EDGE_LOOP('',(#17021,#17022,#17023,#17024));
#3121=EDGE_LOOP('',(#17025,#17026,#17027,#17028));
#3122=EDGE_LOOP('',(#17029,#17030,#17031,#17032));
#3123=EDGE_LOOP('',(#17033,#17034,#17035,#17036));
#3124=EDGE_LOOP('',(#17037,#17038,#17039,#17040));
#3125=EDGE_LOOP('',(#17041,#17042,#17043,#17044));
#3126=EDGE_LOOP('',(#17045,#17046,#17047,#17048));
#3127=EDGE_LOOP('',(#17049,#17050,#17051,#17052));
#3128=EDGE_LOOP('',(#17053,#17054,#17055,#17056));
#3129=EDGE_LOOP('',(#17057,#17058,#17059,#17060));
#3130=EDGE_LOOP('',(#17061,#17062,#17063,#17064));
#3131=EDGE_LOOP('',(#17065,#17066,#17067,#17068));
#3132=EDGE_LOOP('',(#17069,#17070,#17071,#17072));
#3133=EDGE_LOOP('',(#17073,#17074,#17075,#17076));
#3134=EDGE_LOOP('',(#17077,#17078,#17079,#17080));
#3135=EDGE_LOOP('',(#17081,#17082,#17083,#17084));
#3136=EDGE_LOOP('',(#17085,#17086,#17087,#17088));
#3137=EDGE_LOOP('',(#17089,#17090,#17091,#17092));
#3138=EDGE_LOOP('',(#17093,#17094,#17095,#17096));
#3139=EDGE_LOOP('',(#17097,#17098,#17099,#17100));
#3140=EDGE_LOOP('',(#17101,#17102,#17103,#17104));
#3141=EDGE_LOOP('',(#17105,#17106,#17107,#17108));
#3142=EDGE_LOOP('',(#17109,#17110,#17111,#17112));
#3143=EDGE_LOOP('',(#17113,#17114,#17115,#17116));
#3144=EDGE_LOOP('',(#17117,#17118,#17119,#17120));
#3145=EDGE_LOOP('',(#17121,#17122,#17123,#17124));
#3146=EDGE_LOOP('',(#17125,#17126,#17127,#17128));
#3147=EDGE_LOOP('',(#17129,#17130,#17131,#17132));
#3148=EDGE_LOOP('',(#17133,#17134,#17135,#17136));
#3149=EDGE_LOOP('',(#17137,#17138,#17139,#17140));
#3150=EDGE_LOOP('',(#17141,#17142,#17143,#17144));
#3151=EDGE_LOOP('',(#17145,#17146,#17147,#17148));
#3152=EDGE_LOOP('',(#17149,#17150,#17151,#17152));
#3153=EDGE_LOOP('',(#17153,#17154,#17155,#17156));
#3154=EDGE_LOOP('',(#17157,#17158,#17159,#17160));
#3155=EDGE_LOOP('',(#17161,#17162,#17163,#17164));
#3156=EDGE_LOOP('',(#17165,#17166,#17167,#17168));
#3157=EDGE_LOOP('',(#17169,#17170,#17171,#17172));
#3158=EDGE_LOOP('',(#17173,#17174,#17175,#17176));
#3159=EDGE_LOOP('',(#17177,#17178,#17179,#17180));
#3160=EDGE_LOOP('',(#17181,#17182,#17183,#17184));
#3161=EDGE_LOOP('',(#17185,#17186,#17187,#17188));
#3162=EDGE_LOOP('',(#17189,#17190,#17191,#17192));
#3163=EDGE_LOOP('',(#17193,#17194,#17195,#17196));
#3164=EDGE_LOOP('',(#17197,#17198,#17199,#17200));
#3165=EDGE_LOOP('',(#17201,#17202,#17203,#17204));
#3166=EDGE_LOOP('',(#17205,#17206,#17207,#17208));
#3167=EDGE_LOOP('',(#17209,#17210,#17211,#17212));
#3168=EDGE_LOOP('',(#17213,#17214,#17215,#17216));
#3169=EDGE_LOOP('',(#17217,#17218,#17219,#17220));
#3170=EDGE_LOOP('',(#17221,#17222,#17223,#17224));
#3171=EDGE_LOOP('',(#17225,#17226,#17227,#17228));
#3172=EDGE_LOOP('',(#17229,#17230,#17231,#17232));
#3173=EDGE_LOOP('',(#17233,#17234,#17235,#17236));
#3174=EDGE_LOOP('',(#17237,#17238,#17239,#17240));
#3175=EDGE_LOOP('',(#17241,#17242,#17243,#17244));
#3176=EDGE_LOOP('',(#17245,#17246,#17247,#17248));
#3177=EDGE_LOOP('',(#17249,#17250,#17251,#17252));
#3178=EDGE_LOOP('',(#17253,#17254,#17255,#17256));
#3179=EDGE_LOOP('',(#17257,#17258,#17259,#17260));
#3180=EDGE_LOOP('',(#17261,#17262,#17263,#17264));
#3181=EDGE_LOOP('',(#17265,#17266,#17267,#17268));
#3182=EDGE_LOOP('',(#17269,#17270,#17271,#17272));
#3183=EDGE_LOOP('',(#17273,#17274,#17275,#17276));
#3184=EDGE_LOOP('',(#17277,#17278,#17279,#17280));
#3185=EDGE_LOOP('',(#17281,#17282,#17283,#17284));
#3186=EDGE_LOOP('',(#17285,#17286,#17287,#17288));
#3187=EDGE_LOOP('',(#17289,#17290,#17291,#17292));
#3188=EDGE_LOOP('',(#17293,#17294,#17295,#17296));
#3189=EDGE_LOOP('',(#17297,#17298,#17299,#17300));
#3190=EDGE_LOOP('',(#17301,#17302,#17303,#17304));
#3191=EDGE_LOOP('',(#17305,#17306,#17307,#17308));
#3192=EDGE_LOOP('',(#17309,#17310,#17311,#17312));
#3193=EDGE_LOOP('',(#17313,#17314,#17315,#17316));
#3194=EDGE_LOOP('',(#17317,#17318,#17319,#17320));
#3195=EDGE_LOOP('',(#17321,#17322,#17323,#17324));
#3196=EDGE_LOOP('',(#17325,#17326,#17327,#17328));
#3197=EDGE_LOOP('',(#17329,#17330,#17331,#17332));
#3198=EDGE_LOOP('',(#17333,#17334,#17335,#17336));
#3199=EDGE_LOOP('',(#17337,#17338,#17339,#17340));
#3200=EDGE_LOOP('',(#17341,#17342,#17343,#17344));
#3201=EDGE_LOOP('',(#17345,#17346,#17347,#17348));
#3202=EDGE_LOOP('',(#17349));
#3203=EDGE_LOOP('',(#17350,#17351,#17352,#17353));
#3204=EDGE_LOOP('',(#17354,#17355,#17356,#17357));
#3205=EDGE_LOOP('',(#17358));
#3206=EDGE_LOOP('',(#17359,#17360,#17361,#17362,#17363));
#3207=EDGE_LOOP('',(#17364));
#3208=EDGE_LOOP('',(#17365,#17366,#17367,#17368,#17369,#17370,#17371,#17372,
#17373,#17374,#17375,#17376,#17377,#17378,#17379,#17380,#17381,#17382,#17383,
#17384,#17385,#17386,#17387,#17388,#17389,#17390,#17391,#17392,#17393,#17394,
#17395,#17396,#17397,#17398,#17399,#17400,#17401,#17402,#17403,#17404,#17405,
#17406,#17407,#17408,#17409,#17410,#17411,#17412,#17413,#17414,#17415,#17416,
#17417,#17418,#17419,#17420,#17421,#17422,#17423,#17424,#17425,#17426,#17427,
#17428,#17429,#17430,#17431,#17432,#17433,#17434,#17435,#17436,#17437,#17438,
#17439,#17440,#17441,#17442,#17443,#17444,#17445,#17446,#17447,#17448,#17449,
#17450,#17451,#17452,#17453,#17454,#17455,#17456,#17457,#17458,#17459,#17460,
#17461,#17462,#17463,#17464,#17465,#17466,#17467,#17468,#17469,#17470,#17471,
#17472,#17473,#17474,#17475,#17476,#17477,#17478,#17479,#17480,#17481,#17482,
#17483,#17484,#17485,#17486,#17487,#17488,#17489,#17490,#17491,#17492,#17493,
#17494,#17495,#17496,#17497,#17498,#17499,#17500,#17501,#17502,#17503,#17504,
#17505,#17506,#17507,#17508,#17509,#17510,#17511,#17512,#17513,#17514,#17515,
#17516,#17517,#17518,#17519,#17520,#17521,#17522,#17523,#17524,#17525,#17526,
#17527,#17528,#17529,#17530,#17531,#17532,#17533,#17534,#17535,#17536,#17537,
#17538,#17539,#17540,#17541,#17542,#17543,#17544,#17545,#17546,#17547,#17548,
#17549,#17550,#17551,#17552,#17553,#17554,#17555,#17556,#17557,#17558,#17559,
#17560,#17561,#17562,#17563,#17564,#17565,#17566,#17567,#17568));
#3209=EDGE_LOOP('',(#17569,#17570,#17571,#17572));
#3210=EDGE_LOOP('',(#17573));
#3211=EDGE_LOOP('',(#17574,#17575,#17576,#17577,#17578));
#3212=EDGE_LOOP('',(#17579,#17580,#17581,#17582,#17583,#17584,#17585,#17586,
#17587,#17588,#17589,#17590,#17591,#17592,#17593,#17594,#17595,#17596,#17597,
#17598,#17599,#17600,#17601,#17602));
#3213=EDGE_LOOP('',(#17603,#17604,#17605,#17606));
#3214=EDGE_LOOP('',(#17607,#17608,#17609,#17610));
#3215=EDGE_LOOP('',(#17611,#17612,#17613,#17614,#17615,#17616,#17617,#17618,
#17619,#17620,#17621,#17622,#17623,#17624,#17625,#17626,#17627,#17628,#17629,
#17630,#17631,#17632,#17633,#17634));
#3216=EDGE_LOOP('',(#17635,#17636,#17637));
#3217=EDGE_LOOP('',(#17638,#17639,#17640,#17641));
#3218=EDGE_LOOP('',(#17642));
#3219=EDGE_LOOP('',(#17643,#17644,#17645,#17646,#17647,#17648,#17649,#17650,
#17651,#17652,#17653,#17654,#17655,#17656,#17657,#17658,#17659,#17660,#17661,
#17662,#17663,#17664,#17665,#17666,#17667,#17668,#17669,#17670,#17671,#17672,
#17673,#17674,#17675,#17676,#17677,#17678,#17679,#17680,#17681,#17682,#17683,
#17684,#17685,#17686,#17687,#17688,#17689,#17690,#17691,#17692,#17693,#17694,
#17695,#17696,#17697,#17698,#17699,#17700,#17701,#17702,#17703,#17704,#17705,
#17706,#17707,#17708,#17709,#17710,#17711,#17712,#17713,#17714,#17715,#17716,
#17717,#17718,#17719,#17720,#17721,#17722,#17723,#17724,#17725,#17726,#17727,
#17728,#17729,#17730,#17731,#17732,#17733,#17734,#17735,#17736,#17737,#17738,
#17739,#17740,#17741,#17742,#17743,#17744,#17745,#17746,#17747,#17748,#17749,
#17750,#17751,#17752,#17753,#17754,#17755,#17756,#17757,#17758,#17759,#17760,
#17761,#17762,#17763,#17764,#17765,#17766,#17767,#17768,#17769,#17770,#17771,
#17772,#17773,#17774,#17775,#17776,#17777,#17778,#17779,#17780,#17781,#17782,
#17783,#17784,#17785,#17786,#17787,#17788,#17789,#17790,#17791,#17792,#17793,
#17794,#17795,#17796,#17797,#17798,#17799,#17800,#17801,#17802,#17803,#17804,
#17805,#17806,#17807,#17808,#17809,#17810,#17811,#17812,#17813,#17814,#17815,
#17816,#17817,#17818,#17819,#17820,#17821,#17822,#17823,#17824,#17825,#17826,
#17827,#17828,#17829,#17830,#17831,#17832,#17833,#17834,#17835,#17836,#17837,
#17838,#17839,#17840,#17841,#17842,#17843,#17844,#17845,#17846,#17847));
#3220=EDGE_LOOP('',(#17848,#17849,#17850));
#3221=EDGE_LOOP('',(#17851,#17852,#17853,#17854,#17855,#17856));
#3222=EDGE_LOOP('',(#17857));
#3223=EDGE_LOOP('',(#17858,#17859,#17860,#17861));
#3224=EDGE_LOOP('',(#17862,#17863,#17864,#17865));
#3225=EDGE_LOOP('',(#17866,#17867,#17868,#17869));
#3226=EDGE_LOOP('',(#17870,#17871,#17872,#17873));
#3227=EDGE_LOOP('',(#17874,#17875,#17876,#17877));
#3228=EDGE_LOOP('',(#17878,#17879,#17880,#17881));
#3229=EDGE_LOOP('',(#17882,#17883,#17884,#17885));
#3230=EDGE_LOOP('',(#17886,#17887,#17888,#17889));
#3231=EDGE_LOOP('',(#17890,#17891,#17892,#17893));
#3232=EDGE_LOOP('',(#17894,#17895,#17896,#17897));
#3233=EDGE_LOOP('',(#17898,#17899,#17900,#17901));
#3234=EDGE_LOOP('',(#17902,#17903,#17904,#17905));
#3235=EDGE_LOOP('',(#17906,#17907,#17908,#17909));
#3236=EDGE_LOOP('',(#17910,#17911,#17912,#17913));
#3237=EDGE_LOOP('',(#17914,#17915,#17916,#17917));
#3238=EDGE_LOOP('',(#17918,#17919,#17920,#17921));
#3239=EDGE_LOOP('',(#17922,#17923,#17924,#17925));
#3240=EDGE_LOOP('',(#17926,#17927,#17928,#17929));
#3241=EDGE_LOOP('',(#17930,#17931,#17932,#17933));
#3242=EDGE_LOOP('',(#17934,#17935,#17936,#17937));
#3243=EDGE_LOOP('',(#17938,#17939,#17940,#17941));
#3244=EDGE_LOOP('',(#17942,#17943,#17944,#17945,#17946,#17947));
#3245=EDGE_LOOP('',(#17948));
#3246=EDGE_LOOP('',(#17949,#17950,#17951,#17952));
#3247=EDGE_LOOP('',(#17953,#17954,#17955,#17956));
#3248=EDGE_LOOP('',(#17957,#17958,#17959,#17960));
#3249=EDGE_LOOP('',(#17961,#17962,#17963,#17964));
#3250=EDGE_LOOP('',(#17965,#17966,#17967,#17968));
#3251=EDGE_LOOP('',(#17969,#17970,#17971,#17972));
#3252=EDGE_LOOP('',(#17973));
#3253=EDGE_LOOP('',(#17974));
#3254=EDGE_LOOP('',(#17975));
#3255=EDGE_LOOP('',(#17976));
#3256=EDGE_LOOP('',(#17977));
#3257=EDGE_LOOP('',(#17978));
#3258=EDGE_LOOP('',(#17979));
#3259=EDGE_LOOP('',(#17980));
#3260=EDGE_LOOP('',(#17981,#17982,#17983,#17984));
#3261=EDGE_LOOP('',(#17985));
#3262=EDGE_LOOP('',(#17986));
#3263=EDGE_LOOP('',(#17987));
#3264=EDGE_LOOP('',(#17988));
#3265=EDGE_LOOP('',(#17989));
#3266=EDGE_LOOP('',(#17990));
#3267=EDGE_LOOP('',(#17991));
#3268=EDGE_LOOP('',(#17992));
#3269=EDGE_LOOP('',(#17993,#17994,#17995,#17996,#17997,#17998,#17999,#18000));
#3270=EDGE_LOOP('',(#18001,#18002,#18003,#18004,#18005,#18006,#18007,#18008));
#3271=EDGE_LOOP('',(#18009,#18010,#18011,#18012));
#3272=EDGE_LOOP('',(#18013,#18014,#18015,#18016));
#3273=EDGE_LOOP('',(#18017,#18018,#18019,#18020));
#3274=EDGE_LOOP('',(#18021));
#3275=EDGE_LOOP('',(#18022));
#3276=EDGE_LOOP('',(#18023));
#3277=EDGE_LOOP('',(#18024));
#3278=EDGE_LOOP('',(#18025));
#3279=EDGE_LOOP('',(#18026));
#3280=EDGE_LOOP('',(#18027));
#3281=EDGE_LOOP('',(#18028));
#3282=EDGE_LOOP('',(#18029));
#3283=EDGE_LOOP('',(#18030));
#3284=EDGE_LOOP('',(#18031));
#3285=EDGE_LOOP('',(#18032));
#3286=EDGE_LOOP('',(#18033));
#3287=EDGE_LOOP('',(#18034));
#3288=EDGE_LOOP('',(#18035));
#3289=EDGE_LOOP('',(#18036));
#3290=EDGE_LOOP('',(#18037,#18038,#18039,#18040));
#3291=EDGE_LOOP('',(#18041,#18042,#18043,#18044));
#3292=EDGE_LOOP('',(#18045,#18046,#18047,#18048));
#3293=EDGE_LOOP('',(#18049,#18050,#18051,#18052));
#3294=EDGE_LOOP('',(#18053,#18054,#18055,#18056));
#3295=EDGE_LOOP('',(#18057,#18058,#18059,#18060));
#3296=EDGE_LOOP('',(#18061,#18062,#18063,#18064));
#3297=EDGE_LOOP('',(#18065,#18066,#18067,#18068));
#3298=EDGE_LOOP('',(#18069,#18070,#18071,#18072));
#3299=EDGE_LOOP('',(#18073,#18074,#18075,#18076));
#3300=EDGE_LOOP('',(#18077,#18078,#18079,#18080));
#3301=EDGE_LOOP('',(#18081,#18082,#18083,#18084));
#3302=EDGE_LOOP('',(#18085,#18086,#18087,#18088));
#3303=EDGE_LOOP('',(#18089,#18090,#18091,#18092));
#3304=EDGE_LOOP('',(#18093,#18094,#18095,#18096));
#3305=EDGE_LOOP('',(#18097,#18098,#18099,#18100));
#3306=EDGE_LOOP('',(#18101,#18102,#18103,#18104,#18105,#18106,#18107,#18108,
#18109,#18110,#18111,#18112,#18113,#18114,#18115,#18116,#18117,#18118,#18119,
#18120,#18121,#18122,#18123,#18124,#18125,#18126,#18127,#18128,#18129,#18130,
#18131,#18132,#18133,#18134));
#3307=EDGE_LOOP('',(#18135,#18136,#18137,#18138));
#3308=EDGE_LOOP('',(#18139,#18140,#18141,#18142));
#3309=EDGE_LOOP('',(#18143,#18144,#18145,#18146));
#3310=EDGE_LOOP('',(#18147,#18148,#18149,#18150));
#3311=EDGE_LOOP('',(#18151,#18152,#18153,#18154));
#3312=EDGE_LOOP('',(#18155,#18156,#18157,#18158));
#3313=EDGE_LOOP('',(#18159,#18160,#18161,#18162));
#3314=EDGE_LOOP('',(#18163,#18164,#18165,#18166));
#3315=EDGE_LOOP('',(#18167,#18168,#18169,#18170));
#3316=EDGE_LOOP('',(#18171,#18172,#18173,#18174));
#3317=EDGE_LOOP('',(#18175,#18176,#18177,#18178));
#3318=EDGE_LOOP('',(#18179,#18180,#18181,#18182));
#3319=EDGE_LOOP('',(#18183,#18184,#18185,#18186));
#3320=EDGE_LOOP('',(#18187,#18188,#18189,#18190));
#3321=EDGE_LOOP('',(#18191,#18192,#18193,#18194));
#3322=EDGE_LOOP('',(#18195,#18196,#18197,#18198));
#3323=EDGE_LOOP('',(#18199,#18200,#18201,#18202));
#3324=EDGE_LOOP('',(#18203,#18204,#18205,#18206));
#3325=EDGE_LOOP('',(#18207,#18208,#18209,#18210,#18211,#18212,#18213,#18214,
#18215,#18216,#18217,#18218,#18219,#18220,#18221,#18222,#18223,#18224,#18225,
#18226,#18227,#18228,#18229,#18230,#18231,#18232,#18233,#18234,#18235,#18236,
#18237,#18238,#18239,#18240));
#3326=EDGE_LOOP('',(#18241,#18242,#18243,#18244));
#3327=EDGE_LOOP('',(#18245,#18246,#18247,#18248));
#3328=EDGE_LOOP('',(#18249,#18250,#18251,#18252));
#3329=EDGE_LOOP('',(#18253,#18254,#18255,#18256));
#3330=EDGE_LOOP('',(#18257,#18258,#18259,#18260));
#3331=EDGE_LOOP('',(#18261,#18262,#18263,#18264));
#3332=EDGE_LOOP('',(#18265));
#3333=EDGE_LOOP('',(#18266,#18267,#18268,#18269));
#3334=EDGE_LOOP('',(#18270));
#3335=EDGE_LOOP('',(#18271,#18272,#18273,#18274));
#3336=EDGE_LOOP('',(#18275,#18276,#18277,#18278));
#3337=EDGE_LOOP('',(#18279,#18280,#18281,#18282));
#3338=EDGE_LOOP('',(#18283,#18284,#18285,#18286));
#3339=EDGE_LOOP('',(#18287,#18288,#18289,#18290));
#3340=EDGE_LOOP('',(#18291,#18292,#18293,#18294));
#3341=EDGE_LOOP('',(#18295));
#3342=EDGE_LOOP('',(#18296,#18297,#18298,#18299));
#3343=EDGE_LOOP('',(#18300));
#3344=EDGE_LOOP('',(#18301,#18302,#18303,#18304));
#3345=EDGE_LOOP('',(#18305,#18306,#18307,#18308));
#3346=EDGE_LOOP('',(#18309,#18310,#18311,#18312));
#3347=EDGE_LOOP('',(#18313,#18314,#18315,#18316));
#3348=EDGE_LOOP('',(#18317,#18318,#18319,#18320));
#3349=EDGE_LOOP('',(#18321,#18322,#18323,#18324));
#3350=EDGE_LOOP('',(#18325));
#3351=EDGE_LOOP('',(#18326,#18327,#18328,#18329));
#3352=EDGE_LOOP('',(#18330));
#3353=EDGE_LOOP('',(#18331,#18332,#18333,#18334));
#3354=EDGE_LOOP('',(#18335,#18336,#18337,#18338));
#3355=EDGE_LOOP('',(#18339,#18340,#18341,#18342));
#3356=EDGE_LOOP('',(#18343,#18344,#18345,#18346));
#3357=EDGE_LOOP('',(#18347,#18348,#18349,#18350));
#3358=EDGE_LOOP('',(#18351,#18352,#18353,#18354));
#3359=EDGE_LOOP('',(#18355,#18356,#18357,#18358));
#3360=EDGE_LOOP('',(#18359,#18360,#18361,#18362));
#3361=EDGE_LOOP('',(#18363,#18364,#18365,#18366));
#3362=EDGE_LOOP('',(#18367,#18368,#18369,#18370));
#3363=EDGE_LOOP('',(#18371,#18372,#18373,#18374));
#3364=EDGE_LOOP('',(#18375,#18376,#18377,#18378));
#3365=EDGE_LOOP('',(#18379,#18380,#18381,#18382));
#3366=EDGE_LOOP('',(#18383,#18384,#18385,#18386));
#3367=EDGE_LOOP('',(#18387,#18388,#18389,#18390));
#3368=EDGE_LOOP('',(#18391,#18392,#18393,#18394));
#3369=EDGE_LOOP('',(#18395,#18396,#18397,#18398,#18399,#18400,#18401,#18402,
#18403,#18404,#18405,#18406,#18407,#18408,#18409,#18410,#18411,#18412,#18413,
#18414,#18415,#18416,#18417,#18418,#18419,#18420,#18421,#18422,#18423,#18424,
#18425,#18426,#18427,#18428));
#3370=EDGE_LOOP('',(#18429,#18430,#18431,#18432));
#3371=EDGE_LOOP('',(#18433,#18434,#18435,#18436));
#3372=EDGE_LOOP('',(#18437,#18438,#18439,#18440));
#3373=EDGE_LOOP('',(#18441,#18442,#18443,#18444));
#3374=EDGE_LOOP('',(#18445,#18446,#18447,#18448));
#3375=EDGE_LOOP('',(#18449,#18450,#18451,#18452));
#3376=EDGE_LOOP('',(#18453,#18454,#18455,#18456));
#3377=EDGE_LOOP('',(#18457,#18458,#18459,#18460));
#3378=EDGE_LOOP('',(#18461,#18462,#18463,#18464));
#3379=EDGE_LOOP('',(#18465,#18466,#18467,#18468));
#3380=EDGE_LOOP('',(#18469,#18470,#18471,#18472));
#3381=EDGE_LOOP('',(#18473,#18474,#18475,#18476));
#3382=EDGE_LOOP('',(#18477,#18478,#18479,#18480));
#3383=EDGE_LOOP('',(#18481,#18482,#18483,#18484));
#3384=EDGE_LOOP('',(#18485,#18486,#18487,#18488));
#3385=EDGE_LOOP('',(#18489,#18490,#18491,#18492));
#3386=EDGE_LOOP('',(#18493,#18494,#18495,#18496));
#3387=EDGE_LOOP('',(#18497,#18498,#18499,#18500));
#3388=EDGE_LOOP('',(#18501,#18502,#18503,#18504,#18505,#18506,#18507,#18508,
#18509,#18510,#18511,#18512,#18513,#18514,#18515,#18516,#18517,#18518,#18519,
#18520,#18521,#18522,#18523,#18524,#18525,#18526,#18527,#18528,#18529,#18530,
#18531,#18532,#18533,#18534));
#3389=CIRCLE('',#20259,1.04999999999996);
#3390=CIRCLE('',#20260,1.05);
#3391=CIRCLE('',#20261,1.39999999999978);
#3392=CIRCLE('',#20262,2.3640229247478);
#3393=CIRCLE('',#20263,0.599999999999987);
#3394=CIRCLE('',#20264,0.72500000000001);
#3395=CIRCLE('',#20265,2.46743797397101);
#3396=CIRCLE('',#20266,0.450000000000123);
#3397=CIRCLE('',#20267,0.45000000000016);
#3398=CIRCLE('',#20268,2.46743797397104);
#3399=CIRCLE('',#20269,0.724999999999998);
#3400=CIRCLE('',#20270,0.59999999999997);
#3401=CIRCLE('',#20271,2.36402292474775);
#3402=CIRCLE('',#20272,1.39999999999995);
#3403=CIRCLE('',#20273,1.04999999999995);
#3404=CIRCLE('',#20274,1.04999999999981);
#3405=CIRCLE('',#20277,0.45000000000016);
#3406=CIRCLE('',#20279,2.46743797397104);
#3407=CIRCLE('',#20281,0.724999999999998);
#3408=CIRCLE('',#20284,0.59999999999997);
#3409=CIRCLE('',#20286,2.36402292474775);
#3410=CIRCLE('',#20288,1.39999999999995);
#3411=CIRCLE('',#20291,1.04999999999995);
#3412=CIRCLE('',#20294,1.04999999999981);
#3413=CIRCLE('',#20304,1.04999999999996);
#3414=CIRCLE('',#20312,0.450000000000123);
#3415=CIRCLE('',#20314,2.46743797397101);
#3416=CIRCLE('',#20316,0.72500000000001);
#3417=CIRCLE('',#20319,0.599999999999987);
#3418=CIRCLE('',#20321,2.3640229247478);
#3419=CIRCLE('',#20323,1.39999999999978);
#3420=CIRCLE('',#20326,1.05);
#3421=CIRCLE('',#20330,0.45000000000016);
#3422=CIRCLE('',#20331,0.45000000000016);
#3423=CIRCLE('',#20333,2.46743797397104);
#3424=CIRCLE('',#20334,2.46743797397104);
#3425=CIRCLE('',#20336,0.724999999999998);
#3426=CIRCLE('',#20337,0.724999999999998);
#3427=CIRCLE('',#20340,0.59999999999997);
#3428=CIRCLE('',#20341,0.59999999999997);
#3429=CIRCLE('',#20343,2.36402292474775);
#3430=CIRCLE('',#20344,2.36402292474775);
#3431=CIRCLE('',#20346,1.04999999999981);
#3432=CIRCLE('',#20347,1.04999999999995);
#3433=CIRCLE('',#20348,1.39999999999995);
#3434=CIRCLE('',#20349,0.450000000000123);
#3435=CIRCLE('',#20350,2.46743797397101);
#3436=CIRCLE('',#20351,0.72500000000001);
#3437=CIRCLE('',#20352,0.599999999999987);
#3438=CIRCLE('',#20353,2.3640229247478);
#3439=CIRCLE('',#20354,1.39999999999978);
#3440=CIRCLE('',#20355,1.05);
#3441=CIRCLE('',#20356,1.04999999999996);
#3442=CIRCLE('',#20357,2.16656587073651);
#3443=CIRCLE('',#20358,2.16656587073651);
#3444=CIRCLE('',#20363,3.00000000000001);
#3445=CIRCLE('',#20364,3.00000000000001);
#3446=CIRCLE('',#20366,2.16656587073651);
#3447=CIRCLE('',#20369,2.16656587073651);
#3448=CIRCLE('',#20370,1.04999999999996);
#3449=CIRCLE('',#20371,1.05);
#3450=CIRCLE('',#20372,1.39999999999978);
#3451=CIRCLE('',#20373,2.3640229247478);
#3452=CIRCLE('',#20374,0.599999999999987);
#3453=CIRCLE('',#20375,0.72500000000001);
#3454=CIRCLE('',#20376,2.46743797397101);
#3455=CIRCLE('',#20377,0.450000000000123);
#3456=CIRCLE('',#20378,1.39999999999995);
#3457=CIRCLE('',#20379,1.04999999999995);
#3458=CIRCLE('',#20380,1.04999999999981);
#3459=CIRCLE('',#20385,3.00000000000001);
#3460=CIRCLE('',#20386,3.00000000000001);
#3461=CIRCLE('',#20389,3.00000000000001);
#3462=CIRCLE('',#20391,3.00000000000001);
#3463=CIRCLE('',#20393,3.00000000000001);
#3464=CIRCLE('',#20395,3.00000000000001);
#3465=CIRCLE('',#20423,1.39999999999995);
#3466=CIRCLE('',#20424,1.39999999999995);
#3467=CIRCLE('',#20427,1.04999999999995);
#3468=CIRCLE('',#20428,1.04999999999995);
#3469=CIRCLE('',#20431,1.04999999999981);
#3470=CIRCLE('',#20432,1.04999999999981);
#3471=CIRCLE('',#20444,1.04999999999996);
#3472=CIRCLE('',#20445,1.04999999999996);
#3473=CIRCLE('',#20447,1.05);
#3474=CIRCLE('',#20448,1.39999999999978);
#3475=CIRCLE('',#20449,2.3640229247478);
#3476=CIRCLE('',#20450,0.599999999999987);
#3477=CIRCLE('',#20451,0.72500000000001);
#3478=CIRCLE('',#20452,2.46743797397101);
#3479=CIRCLE('',#20453,0.450000000000123);
#3480=CIRCLE('',#20454,0.45000000000016);
#3481=CIRCLE('',#20455,2.46743797397104);
#3482=CIRCLE('',#20456,0.724999999999998);
#3483=CIRCLE('',#20457,0.59999999999997);
#3484=CIRCLE('',#20458,2.36402292474775);
#3485=CIRCLE('',#20462,1.05);
#3486=CIRCLE('',#20465,1.39999999999978);
#3487=CIRCLE('',#20467,2.3640229247478);
#3488=CIRCLE('',#20469,0.599999999999987);
#3489=CIRCLE('',#20472,0.72500000000001);
#3490=CIRCLE('',#20474,2.46743797397101);
#3491=CIRCLE('',#20476,0.450000000000123);
#3492=CIRCLE('',#20481,0.45000000000016);
#3493=CIRCLE('',#20483,2.46743797397104);
#3494=CIRCLE('',#20485,0.724999999999998);
#3495=CIRCLE('',#20488,0.59999999999997);
#3496=CIRCLE('',#20490,2.36402292474775);
#3497=CIRCLE('',#20494,1.04999999999981);
#3498=CIRCLE('',#20495,1.04999999999995);
#3499=CIRCLE('',#20496,1.39999999999995);
#3500=CIRCLE('',#20497,2.36402292474775);
#3501=CIRCLE('',#20498,0.59999999999997);
#3502=CIRCLE('',#20499,0.724999999999998);
#3503=CIRCLE('',#20500,2.46743797397104);
#3504=CIRCLE('',#20501,0.45000000000016);
#3505=CIRCLE('',#20502,0.450000000000123);
#3506=CIRCLE('',#20503,2.46743797397101);
#3507=CIRCLE('',#20504,0.72500000000001);
#3508=CIRCLE('',#20505,0.599999999999987);
#3509=CIRCLE('',#20506,2.3640229247478);
#3510=CIRCLE('',#20507,1.39999999999978);
#3511=CIRCLE('',#20508,1.05);
#3512=CIRCLE('',#20509,1.04999999999996);
#3513=CIRCLE('',#20512,0.45000000000016);
#3514=CIRCLE('',#20514,2.46743797397104);
#3515=CIRCLE('',#20516,0.724999999999998);
#3516=CIRCLE('',#20519,0.59999999999997);
#3517=CIRCLE('',#20521,2.36402292474775);
#3518=CIRCLE('',#20523,1.39999999999995);
#3519=CIRCLE('',#20526,1.04999999999995);
#3520=CIRCLE('',#20529,1.04999999999981);
#3521=CIRCLE('',#20539,1.04999999999996);
#3522=CIRCLE('',#20547,0.450000000000123);
#3523=CIRCLE('',#20549,2.46743797397101);
#3524=CIRCLE('',#20551,0.72500000000001);
#3525=CIRCLE('',#20554,0.599999999999987);
#3526=CIRCLE('',#20556,2.3640229247478);
#3527=CIRCLE('',#20558,1.39999999999978);
#3528=CIRCLE('',#20561,1.05);
#3529=CIRCLE('',#20565,0.45000000000016);
#3530=CIRCLE('',#20566,0.45000000000016);
#3531=CIRCLE('',#20568,2.46743797397104);
#3532=CIRCLE('',#20569,2.46743797397104);
#3533=CIRCLE('',#20571,0.724999999999998);
#3534=CIRCLE('',#20572,0.724999999999998);
#3535=CIRCLE('',#20575,0.59999999999997);
#3536=CIRCLE('',#20576,0.59999999999997);
#3537=CIRCLE('',#20578,2.36402292474775);
#3538=CIRCLE('',#20579,2.36402292474775);
#3539=CIRCLE('',#20581,2.16656587073651);
#3540=CIRCLE('',#20582,2.16656587073651);
#3541=CIRCLE('',#20583,1.04999999999996);
#3542=CIRCLE('',#20584,1.05);
#3543=CIRCLE('',#20585,1.39999999999978);
#3544=CIRCLE('',#20586,2.3640229247478);
#3545=CIRCLE('',#20587,0.599999999999987);
#3546=CIRCLE('',#20588,0.72500000000001);
#3547=CIRCLE('',#20589,2.46743797397101);
#3548=CIRCLE('',#20590,0.450000000000123);
#3549=CIRCLE('',#20591,1.39999999999995);
#3550=CIRCLE('',#20592,1.04999999999995);
#3551=CIRCLE('',#20593,1.04999999999981);
#3552=CIRCLE('',#20598,3.00000000000001);
#3553=CIRCLE('',#20599,3.00000000000001);
#3554=CIRCLE('',#20601,2.16656587073651);
#3555=CIRCLE('',#20604,1.04999999999981);
#3556=CIRCLE('',#20605,1.04999999999995);
#3557=CIRCLE('',#20606,1.39999999999995);
#3558=CIRCLE('',#20607,0.450000000000123);
#3559=CIRCLE('',#20608,2.46743797397101);
#3560=CIRCLE('',#20609,0.72500000000001);
#3561=CIRCLE('',#20610,0.599999999999987);
#3562=CIRCLE('',#20611,2.3640229247478);
#3563=CIRCLE('',#20612,1.39999999999978);
#3564=CIRCLE('',#20613,1.05);
#3565=CIRCLE('',#20614,1.04999999999996);
#3566=CIRCLE('',#20615,2.16656587073651);
#3567=CIRCLE('',#20620,3.00000000000001);
#3568=CIRCLE('',#20621,3.00000000000001);
#3569=CIRCLE('',#20624,3.00000000000001);
#3570=CIRCLE('',#20626,3.00000000000001);
#3571=CIRCLE('',#20628,3.00000000000001);
#3572=CIRCLE('',#20630,3.00000000000001);
#3573=CIRCLE('',#20658,1.39999999999995);
#3574=CIRCLE('',#20659,1.39999999999995);
#3575=CIRCLE('',#20662,1.04999999999995);
#3576=CIRCLE('',#20663,1.04999999999995);
#3577=CIRCLE('',#20666,1.04999999999981);
#3578=CIRCLE('',#20667,1.04999999999981);
#3579=CIRCLE('',#20679,1.04999999999996);
#3580=CIRCLE('',#20680,1.04999999999996);
#3581=CIRCLE('',#20682,1.05);
#3582=CIRCLE('',#20683,2.36402292474775);
#3583=CIRCLE('',#20684,0.59999999999997);
#3584=CIRCLE('',#20685,0.724999999999998);
#3585=CIRCLE('',#20686,2.46743797397104);
#3586=CIRCLE('',#20687,0.45000000000016);
#3587=CIRCLE('',#20688,0.450000000000123);
#3588=CIRCLE('',#20689,2.46743797397101);
#3589=CIRCLE('',#20690,0.72500000000001);
#3590=CIRCLE('',#20691,0.599999999999987);
#3591=CIRCLE('',#20692,2.3640229247478);
#3592=CIRCLE('',#20693,1.39999999999978);
#3593=CIRCLE('',#20697,1.05);
#3594=CIRCLE('',#20700,1.39999999999978);
#3595=CIRCLE('',#20702,2.3640229247478);
#3596=CIRCLE('',#20704,0.599999999999987);
#3597=CIRCLE('',#20707,0.72500000000001);
#3598=CIRCLE('',#20709,2.46743797397101);
#3599=CIRCLE('',#20711,0.450000000000123);
#3600=CIRCLE('',#20716,0.45000000000016);
#3601=CIRCLE('',#20718,2.46743797397104);
#3602=CIRCLE('',#20720,0.724999999999998);
#3603=CIRCLE('',#20723,0.59999999999997);
#3604=CIRCLE('',#20725,2.36402292474775);
#3605=CIRCLE('',#20729,8.671875);
#3606=CIRCLE('',#20730,8.671875);
#3607=CIRCLE('',#20732,8.781875);
#3608=CIRCLE('',#20733,0.110000000000001);
#3609=CIRCLE('',#20735,13.0772848379569);
#3610=CIRCLE('',#20736,5.39274861573998);
#3611=CIRCLE('',#20737,9.6875);
#3612=CIRCLE('',#20739,13.867180376262);
#3613=CIRCLE('',#20741,14.9186522951742);
#3614=CIRCLE('',#20742,14.9186522951742);
#3615=CIRCLE('',#20743,14.9186522951742);
#3616=CIRCLE('',#20744,14.9186522951742);
#3617=CIRCLE('',#20745,14.9186522951742);
#3618=CIRCLE('',#20746,14.9186522951742);
#3619=CIRCLE('',#20747,14.9186522951742);
#3620=CIRCLE('',#20748,14.9186522951742);
#3621=CIRCLE('',#20749,14.9186522951742);
#3622=CIRCLE('',#20750,0.726288026366507);
#3623=CIRCLE('',#20751,14.9186522951742);
#3624=CIRCLE('',#20752,14.9186522951742);
#3625=CIRCLE('',#20753,14.9186522951742);
#3626=CIRCLE('',#20754,14.9186522951742);
#3627=CIRCLE('',#20755,14.9186522951742);
#3628=CIRCLE('',#20756,14.9186522951742);
#3629=CIRCLE('',#20757,14.9186522951742);
#3630=CIRCLE('',#20758,14.9186522951742);
#3631=CIRCLE('',#20760,12.7315647249454);
#3632=CIRCLE('',#20761,13.5214602632505);
#3633=CIRCLE('',#20763,9.6875);
#3634=CIRCLE('',#20764,4.84274861573998);
#3635=CIRCLE('',#20766,1.27628802636651);
#3636=CIRCLE('',#20767,15.5300994798678);
#3637=CIRCLE('',#20768,1.27629997511691);
#3638=CIRCLE('',#20769,14.7602281873362);
#3639=CIRCLE('',#20770,1.27629996428189);
#3640=CIRCLE('',#20771,15.5300994798678);
#3641=CIRCLE('',#20772,1.27629997511692);
#3642=CIRCLE('',#20773,14.7602281873362);
#3643=CIRCLE('',#20774,1.27629996428189);
#3644=CIRCLE('',#20775,15.5300994798678);
#3645=CIRCLE('',#20776,1.27629997511692);
#3646=CIRCLE('',#20777,14.7602281873362);
#3647=CIRCLE('',#20778,1.27629996428189);
#3648=CIRCLE('',#20779,15.5300994798678);
#3649=CIRCLE('',#20780,1.27629997511691);
#3650=CIRCLE('',#20781,14.7602281873362);
#3651=CIRCLE('',#20782,1.27629996428186);
#3652=CIRCLE('',#20783,15.5300994798678);
#3653=CIRCLE('',#20784,1.27629997511693);
#3654=CIRCLE('',#20785,14.7602281873362);
#3655=CIRCLE('',#20786,1.27629996428187);
#3656=CIRCLE('',#20787,15.5300994798678);
#3657=CIRCLE('',#20788,1.27629997511691);
#3658=CIRCLE('',#20789,14.7602281873362);
#3659=CIRCLE('',#20790,1.27629996428189);
#3660=CIRCLE('',#20791,15.5300994798678);
#3661=CIRCLE('',#20792,1.27629997511692);
#3662=CIRCLE('',#20793,14.7602281873362);
#3663=CIRCLE('',#20794,1.27629996428189);
#3664=CIRCLE('',#20795,15.5300994798678);
#3665=CIRCLE('',#20796,1.27629997511693);
#3666=CIRCLE('',#20797,14.7602281873362);
#3667=CIRCLE('',#20798,1.27629996428189);
#3668=CIRCLE('',#20799,15.5300994798678);
#3669=CIRCLE('',#20801,14.5602281873362);
#3670=CIRCLE('',#20803,14.5602281873362);
#3671=CIRCLE('',#20805,14.5602281873362);
#3672=CIRCLE('',#20807,14.5602281873362);
#3673=CIRCLE('',#20809,14.5602281873362);
#3674=CIRCLE('',#20811,14.5602281873362);
#3675=CIRCLE('',#20813,14.5602281873362);
#3676=CIRCLE('',#20815,14.5602281873362);
#3677=CIRCLE('',#20817,14.4779295903485);
#3678=CIRCLE('',#20819,14.4779295903485);
#3679=CIRCLE('',#20821,14.4779295903485);
#3680=CIRCLE('',#20823,14.4779295903485);
#3681=CIRCLE('',#20825,14.4779295903485);
#3682=CIRCLE('',#20827,14.4779295903485);
#3683=CIRCLE('',#20829,14.4779295903485);
#3684=CIRCLE('',#20831,14.4779295903485);
#3685=CIRCLE('',#20867,3.828125);
#3686=CIRCLE('',#20869,8.4375);
#3687=CIRCLE('',#20870,3.828125);
#3688=CIRCLE('',#20871,8.4375);
#3689=CIRCLE('',#20873,5.44);
#3690=CIRCLE('',#20874,0.550000000000001);
#3691=CIRCLE('',#20875,5.10805041359455);
#3692=CIRCLE('',#20876,5.10805041359455);
#3693=CIRCLE('',#20878,5.);
#3694=CIRCLE('',#20879,5.);
#3695=CIRCLE('',#20881,5.);
#3696=CIRCLE('',#20883,5.10805041359455);
#3697=CIRCLE('',#20885,0.550000000000001);
#3698=CIRCLE('',#20886,5.44);
#3699=CIRCLE('',#20888,8.21796310590599);
#3700=CIRCLE('',#20889,0.55);
#3701=CIRCLE('',#20890,8.4375);
#3702=CIRCLE('',#20892,8.4375);
#3703=CIRCLE('',#20893,0.55);
#3704=CIRCLE('',#20894,8.21796310590599);
#3705=CIRCLE('',#20900,15.625);
#3706=CIRCLE('',#20901,3.828125);
#3707=CIRCLE('',#20902,15.625);
#3708=CIRCLE('',#20904,17.5);
#3709=CIRCLE('',#20905,17.5);
#3710=CIRCLE('',#20907,0.55);
#3711=CIRCLE('',#20908,17.0170281388728);
#3712=CIRCLE('',#20910,16.796875);
#3713=CIRCLE('',#20912,17.0170281388728);
#3714=CIRCLE('',#20913,16.796875);
#3715=CIRCLE('',#20914,17.0170281388728);
#3716=CIRCLE('',#20916,0.55);
#3717=CIRCLE('',#20918,15.625);
#3718=CIRCLE('',#20920,15.625);
#3719=CIRCLE('',#20924,3.828125);
#3720=CIRCLE('',#20926,3.828125);
#3721=CIRCLE('',#20928,3.828125);
#3722=CIRCLE('',#20930,3.828125);
#3723=CIRCLE('',#20932,3.828125);
#3724=CIRCLE('',#20934,3.828125);
#3725=CIRCLE('',#20936,3.828125);
#3726=CIRCLE('',#20938,14.46011695371);
#3727=CIRCLE('',#20939,14.46011695371);
#3728=CIRCLE('',#20940,3.828125);
#3729=CIRCLE('',#20941,12.9162151497931);
#3730=CIRCLE('',#20942,12.9162151497931);
#3731=CIRCLE('',#20944,8.671875);
#3732=CIRCLE('',#20945,8.671875);
#3733=CIRCLE('',#20947,8.781875);
#3734=CIRCLE('',#20948,0.110000000000001);
#3735=CIRCLE('',#20950,13.0772848379569);
#3736=CIRCLE('',#20951,5.39274861573998);
#3737=CIRCLE('',#20952,9.6875);
#3738=CIRCLE('',#20954,13.867180376262);
#3739=CIRCLE('',#20956,14.9186522951742);
#3740=CIRCLE('',#20957,14.9186522951742);
#3741=CIRCLE('',#20958,14.9186522951742);
#3742=CIRCLE('',#20959,14.9186522951742);
#3743=CIRCLE('',#20960,14.9186522951742);
#3744=CIRCLE('',#20961,14.9186522951742);
#3745=CIRCLE('',#20962,14.9186522951742);
#3746=CIRCLE('',#20963,14.9186522951742);
#3747=CIRCLE('',#20964,14.9186522951742);
#3748=CIRCLE('',#20965,0.726288026366507);
#3749=CIRCLE('',#20966,14.9186522951742);
#3750=CIRCLE('',#20967,14.9186522951742);
#3751=CIRCLE('',#20968,14.9186522951742);
#3752=CIRCLE('',#20969,14.9186522951742);
#3753=CIRCLE('',#20970,14.9186522951742);
#3754=CIRCLE('',#20971,14.9186522951742);
#3755=CIRCLE('',#20972,14.9186522951742);
#3756=CIRCLE('',#20973,14.9186522951742);
#3757=CIRCLE('',#20975,9.6875);
#3758=CIRCLE('',#20976,4.84274861573998);
#3759=CIRCLE('',#20977,12.7315647249454);
#3760=CIRCLE('',#20980,1.27628802636651);
#3761=CIRCLE('',#20981,15.5300994798678);
#3762=CIRCLE('',#20982,1.27629996428189);
#3763=CIRCLE('',#20983,14.7602281873362);
#3764=CIRCLE('',#20984,1.27629997511693);
#3765=CIRCLE('',#20985,15.5300994798678);
#3766=CIRCLE('',#20986,1.27629996428189);
#3767=CIRCLE('',#20987,14.7602281873362);
#3768=CIRCLE('',#20988,1.27629997511692);
#3769=CIRCLE('',#20989,15.5300994798678);
#3770=CIRCLE('',#20990,1.27629996428189);
#3771=CIRCLE('',#20991,14.7602281873362);
#3772=CIRCLE('',#20992,1.27629997511691);
#3773=CIRCLE('',#20993,15.5300994798678);
#3774=CIRCLE('',#20994,1.27629996428187);
#3775=CIRCLE('',#20995,14.7602281873362);
#3776=CIRCLE('',#20996,1.27629997511693);
#3777=CIRCLE('',#20997,15.5300994798678);
#3778=CIRCLE('',#20998,1.27629996428186);
#3779=CIRCLE('',#20999,14.7602281873362);
#3780=CIRCLE('',#21000,1.27629997511691);
#3781=CIRCLE('',#21001,15.5300994798678);
#3782=CIRCLE('',#21002,1.27629996428189);
#3783=CIRCLE('',#21003,14.7602281873362);
#3784=CIRCLE('',#21004,1.27629997511692);
#3785=CIRCLE('',#21005,15.5300994798678);
#3786=CIRCLE('',#21006,1.27629996428189);
#3787=CIRCLE('',#21007,14.7602281873362);
#3788=CIRCLE('',#21008,1.27629997511692);
#3789=CIRCLE('',#21009,15.5300994798678);
#3790=CIRCLE('',#21010,1.27629996428189);
#3791=CIRCLE('',#21011,14.7602281873362);
#3792=CIRCLE('',#21012,1.27629997511691);
#3793=CIRCLE('',#21013,15.5300994798678);
#3794=CIRCLE('',#21015,14.5602281873362);
#3795=CIRCLE('',#21017,14.5602281873362);
#3796=CIRCLE('',#21019,14.5602281873362);
#3797=CIRCLE('',#21021,14.5602281873362);
#3798=CIRCLE('',#21023,14.5602281873362);
#3799=CIRCLE('',#21025,14.5602281873362);
#3800=CIRCLE('',#21027,14.5602281873362);
#3801=CIRCLE('',#21029,14.5602281873362);
#3802=CIRCLE('',#21031,14.4779295903485);
#3803=CIRCLE('',#21033,14.4779295903485);
#3804=CIRCLE('',#21035,14.4779295903485);
#3805=CIRCLE('',#21037,14.4779295903485);
#3806=CIRCLE('',#21039,14.4779295903485);
#3807=CIRCLE('',#21041,14.4779295903485);
#3808=CIRCLE('',#21043,14.4779295903485);
#3809=CIRCLE('',#21045,14.4779295903485);
#3810=CIRCLE('',#21115,3.25);
#3811=CIRCLE('',#21116,3.25);
#3812=CIRCLE('',#21126,0.499999999999999);
#3813=CIRCLE('',#21127,0.499999999999999);
#3814=CIRCLE('',#21130,0.499999999999998);
#3815=CIRCLE('',#21131,0.499999999999998);
#3816=CIRCLE('',#21144,0.499999999999998);
#3817=CIRCLE('',#21145,0.499999999999998);
#3818=CIRCLE('',#21148,0.499999999999999);
#3819=CIRCLE('',#21149,0.499999999999999);
#3820=CIRCLE('',#21160,2.);
#3821=CIRCLE('',#21161,2.);
#3822=CIRCLE('',#21171,0.499999999999999);
#3823=CIRCLE('',#21172,0.499999999999999);
#3824=CIRCLE('',#21175,0.499999999999998);
#3825=CIRCLE('',#21176,0.499999999999998);
#3826=CIRCLE('',#21190,3.25);
#3827=CIRCLE('',#21191,3.25);
#3828=CIRCLE('',#21194,0.499999999999998);
#3829=CIRCLE('',#21195,0.499999999999998);
#3830=CIRCLE('',#21198,0.499999999999999);
#3831=CIRCLE('',#21199,0.499999999999999);
#3832=CIRCLE('',#21210,2.);
#3833=CIRCLE('',#21211,2.);
#3834=CIRCLE('',#21256,3.25);
#3835=CIRCLE('',#21257,3.25);
#3836=CIRCLE('',#21303,3.25);
#3837=CIRCLE('',#21304,3.25);
#3838=CIRCLE('',#21315,0.499999999999999);
#3839=CIRCLE('',#21316,0.499999999999999);
#3840=CIRCLE('',#21319,0.499999999999998);
#3841=CIRCLE('',#21320,0.499999999999998);
#3842=CIRCLE('',#21333,0.499999999999998);
#3843=CIRCLE('',#21334,0.499999999999998);
#3844=CIRCLE('',#21337,0.499999999999999);
#3845=CIRCLE('',#21338,0.499999999999999);
#3846=CIRCLE('',#21349,2.);
#3847=CIRCLE('',#21350,2.);
#3848=CIRCLE('',#21359,2.);
#3849=CIRCLE('',#21360,0.499999999999998);
#3850=CIRCLE('',#21361,0.499999999999999);
#3851=CIRCLE('',#21362,0.499999999999998);
#3852=CIRCLE('',#21363,0.499999999999999);
#3853=CIRCLE('',#21364,3.25);
#3854=CIRCLE('',#21367,0.499999999999999);
#3855=CIRCLE('',#21370,0.499999999999998);
#3856=CIRCLE('',#21384,3.25);
#3857=CIRCLE('',#21387,0.499999999999998);
#3858=CIRCLE('',#21390,0.499999999999999);
#3859=CIRCLE('',#21401,2.);
#3860=CIRCLE('',#21412,7.925);
#3861=CIRCLE('',#21513,7.925);
#3862=CIRCLE('',#21515,4.81675);
#3863=CIRCLE('',#21516,4.81675);
#3864=CIRCLE('',#21526,4.81675);
#3865=CIRCLE('',#21528,4.91825);
#3866=CIRCLE('',#21539,5.6435);
#3867=CIRCLE('',#21640,5.00000000000001);
#3868=CIRCLE('',#21641,4.00000000000001);
#3869=CIRCLE('',#21643,5.00000000000001);
#3870=CIRCLE('',#21646,4.);
#3871=CIRCLE('',#21647,5.);
#3872=CIRCLE('',#21649,5.);
#3873=CIRCLE('',#21652,7.925);
#3874=CIRCLE('',#21654,5.6435);
#3875=CIRCLE('',#21656,4.81675);
#3876=CIRCLE('',#21658,4.91825);
#3877=CIRCLE('',#21665,5.);
#3878=CIRCLE('',#21666,5.);
#3879=CIRCLE('',#21667,8.09375);
#3880=CIRCLE('',#21669,3.00000000000001);
#3881=CIRCLE('',#21670,3.00000000000001);
#3882=CIRCLE('',#21672,3.00000000000001);
#3883=CIRCLE('',#21673,3.00000000000001);
#3884=CIRCLE('',#21675,3.);
#3885=CIRCLE('',#21676,3.);
#3886=CIRCLE('',#21678,3.);
#3887=CIRCLE('',#21679,3.);
#3888=CIRCLE('',#21681,3.);
#3889=CIRCLE('',#21682,3.);
#3890=CIRCLE('',#21684,3.);
#3891=CIRCLE('',#21685,3.);
#3892=CIRCLE('',#21687,3.00000000000001);
#3893=CIRCLE('',#21688,3.00000000000001);
#3894=CIRCLE('',#21690,3.00000000000001);
#3895=CIRCLE('',#21691,3.00000000000001);
#3896=CIRCLE('',#21693,3.00000000000001);
#3897=CIRCLE('',#21694,3.00000000000001);
#3898=CIRCLE('',#21696,3.00000000000001);
#3899=CIRCLE('',#21697,3.00000000000001);
#3900=CIRCLE('',#21699,3.);
#3901=CIRCLE('',#21700,3.);
#3902=CIRCLE('',#21702,3.);
#3903=CIRCLE('',#21703,3.);
#3904=CIRCLE('',#21705,3.);
#3905=CIRCLE('',#21706,3.);
#3906=CIRCLE('',#21708,3.);
#3907=CIRCLE('',#21709,3.);
#3908=CIRCLE('',#21711,3.00000000000001);
#3909=CIRCLE('',#21712,3.00000000000001);
#3910=CIRCLE('',#21714,3.00000000000001);
#3911=CIRCLE('',#21715,3.00000000000001);
#3912=CIRCLE('',#21717,8.09375);
#3913=CIRCLE('',#21719,5.);
#3914=CIRCLE('',#21722,5.);
#3915=CIRCLE('',#21739,0.450000000000145);
#3916=CIRCLE('',#21740,0.450000000000145);
#3917=CIRCLE('',#21742,2.46743797397102);
#3918=CIRCLE('',#21743,2.46743797397102);
#3919=CIRCLE('',#21745,0.725000000000007);
#3920=CIRCLE('',#21746,0.725000000000007);
#3921=CIRCLE('',#21749,0.599999999999981);
#3922=CIRCLE('',#21750,0.599999999999981);
#3923=CIRCLE('',#21752,2.3640229247478);
#3924=CIRCLE('',#21753,2.3640229247478);
#3925=CIRCLE('',#21755,1.39999999999995);
#3926=CIRCLE('',#21756,1.39999999999995);
#3927=CIRCLE('',#21759,1.05000000000001);
#3928=CIRCLE('',#21760,1.05000000000001);
#3929=CIRCLE('',#21763,1.04999999999996);
#3930=CIRCLE('',#21764,1.04999999999996);
#3931=CIRCLE('',#21767,1.09999999999999);
#3932=CIRCLE('',#21768,1.09999999999999);
#3933=CIRCLE('',#21772,1.09999999999999);
#3934=CIRCLE('',#21773,1.04999999999996);
#3935=CIRCLE('',#21774,1.05000000000001);
#3936=CIRCLE('',#21775,1.39999999999995);
#3937=CIRCLE('',#21776,2.3640229247478);
#3938=CIRCLE('',#21777,0.599999999999981);
#3939=CIRCLE('',#21778,0.725000000000007);
#3940=CIRCLE('',#21779,2.46743797397102);
#3941=CIRCLE('',#21780,0.450000000000145);
#3942=CIRCLE('',#21783,0.450000000000145);
#3943=CIRCLE('',#21785,2.46743797397102);
#3944=CIRCLE('',#21787,0.725000000000007);
#3945=CIRCLE('',#21790,0.599999999999981);
#3946=CIRCLE('',#21792,2.3640229247478);
#3947=CIRCLE('',#21794,1.39999999999995);
#3948=CIRCLE('',#21797,1.05000000000001);
#3949=CIRCLE('',#21800,1.04999999999996);
#3950=CIRCLE('',#21803,1.09999999999999);
#3951=CIRCLE('',#21811,17.5);
#3952=CIRCLE('',#21812,17.5);
#3953=CIRCLE('',#21821,5.);
#3954=CIRCLE('',#21822,5.);
#3955=CIRCLE('',#21831,17.5);
#3956=CIRCLE('',#21832,17.5);
#3957=CIRCLE('',#21842,0.450000000000145);
#3958=CIRCLE('',#21843,0.450000000000145);
#3959=CIRCLE('',#21845,2.46743797397102);
#3960=CIRCLE('',#21846,2.46743797397102);
#3961=CIRCLE('',#21848,0.725000000000007);
#3962=CIRCLE('',#21849,0.725000000000007);
#3963=CIRCLE('',#21852,0.599999999999981);
#3964=CIRCLE('',#21853,0.599999999999981);
#3965=CIRCLE('',#21855,2.3640229247478);
#3966=CIRCLE('',#21856,2.3640229247478);
#3967=CIRCLE('',#21858,1.39999999999995);
#3968=CIRCLE('',#21859,1.39999999999995);
#3969=CIRCLE('',#21862,1.05000000000001);
#3970=CIRCLE('',#21863,1.05000000000001);
#3971=CIRCLE('',#21866,1.04999999999996);
#3972=CIRCLE('',#21867,1.04999999999996);
#3973=CIRCLE('',#21870,1.09999999999999);
#3974=CIRCLE('',#21871,1.09999999999999);
#3975=CIRCLE('',#21875,0.450000000000145);
#3976=CIRCLE('',#21876,2.46743797397102);
#3977=CIRCLE('',#21877,0.725000000000007);
#3978=CIRCLE('',#21878,0.599999999999981);
#3979=CIRCLE('',#21879,2.3640229247478);
#3980=CIRCLE('',#21880,1.39999999999995);
#3981=CIRCLE('',#21881,1.05000000000001);
#3982=CIRCLE('',#21882,1.04999999999996);
#3983=CIRCLE('',#21883,1.09999999999999);
#3984=CIRCLE('',#21886,0.450000000000145);
#3985=CIRCLE('',#21888,2.46743797397102);
#3986=CIRCLE('',#21890,0.725000000000007);
#3987=CIRCLE('',#21893,0.599999999999981);
#3988=CIRCLE('',#21895,2.3640229247478);
#3989=CIRCLE('',#21897,1.39999999999995);
#3990=CIRCLE('',#21900,1.05000000000001);
#3991=CIRCLE('',#21903,1.04999999999996);
#3992=CIRCLE('',#21906,1.09999999999999);
#3993=LINE('',#27152,#5874);
#3994=LINE('',#27154,#5875);
#3995=LINE('',#27156,#5876);
#3996=LINE('',#27158,#5877);
#3997=LINE('',#27162,#5878);
#3998=LINE('',#27166,#5879);
#3999=LINE('',#27174,#5880);
#4000=LINE('',#27182,#5881);
#4001=LINE('',#27184,#5882);
#4002=LINE('',#27186,#5883);
#4003=LINE('',#27194,#5884);
#4004=LINE('',#27202,#5885);
#4005=LINE('',#27206,#5886);
#4006=LINE('',#27210,#5887);
#4007=LINE('',#27212,#5888);
#4008=LINE('',#27214,#5889);
#4009=LINE('',#27216,#5890);
#4010=LINE('',#27218,#5891);
#4011=LINE('',#27220,#5892);
#4012=LINE('',#27221,#5893);
#4013=LINE('',#27224,#5894);
#4014=LINE('',#27226,#5895);
#4015=LINE('',#27227,#5896);
#4016=LINE('',#27231,#5897);
#4017=LINE('',#27235,#5898);
#4018=LINE('',#27239,#5899);
#4019=LINE('',#27242,#5900);
#4020=LINE('',#27243,#5901);
#4021=LINE('',#27247,#5902);
#4022=LINE('',#27251,#5903);
#4023=LINE('',#27255,#5904);
#4024=LINE('',#27258,#5905);
#4025=LINE('',#27259,#5906);
#4026=LINE('',#27263,#5907);
#4027=LINE('',#27266,#5908);
#4028=LINE('',#27267,#5909);
#4029=LINE('',#27271,#5910);
#4030=LINE('',#27274,#5911);
#4031=LINE('',#27275,#5912);
#4032=LINE('',#27278,#5913);
#4033=LINE('',#27279,#5914);
#4034=LINE('',#27282,#5915);
#4035=LINE('',#27283,#5916);
#4036=LINE('',#27286,#5917);
#4037=LINE('',#27287,#5918);
#4038=LINE('',#27290,#5919);
#4039=LINE('',#27292,#5920);
#4040=LINE('',#27293,#5921);
#4041=LINE('',#27296,#5922);
#4042=LINE('',#27297,#5923);
#4043=LINE('',#27300,#5924);
#4044=LINE('',#27301,#5925);
#4045=LINE('',#27304,#5926);
#4046=LINE('',#27305,#5927);
#4047=LINE('',#27309,#5928);
#4048=LINE('',#27312,#5929);
#4049=LINE('',#27313,#5930);
#4050=LINE('',#27316,#5931);
#4051=LINE('',#27317,#5932);
#4052=LINE('',#27319,#5933);
#4053=LINE('',#27322,#5934);
#4054=LINE('',#27323,#5935);
#4055=LINE('',#27326,#5936);
#4056=LINE('',#27327,#5937);
#4057=LINE('',#27330,#5938);
#4058=LINE('',#27331,#5939);
#4059=LINE('',#27334,#5940);
#4060=LINE('',#27338,#5941);
#4061=LINE('',#27342,#5942);
#4062=LINE('',#27346,#5943);
#4063=LINE('',#27347,#5944);
#4064=LINE('',#27350,#5945);
#4065=LINE('',#27354,#5946);
#4066=LINE('',#27358,#5947);
#4067=LINE('',#27362,#5948);
#4068=LINE('',#27363,#5949);
#4069=LINE('',#27370,#5950);
#4070=LINE('',#27372,#5951);
#4071=LINE('',#27374,#5952);
#4072=LINE('',#27375,#5953);
#4073=LINE('',#27380,#5954);
#4074=LINE('',#27386,#5955);
#4075=LINE('',#27392,#5956);
#4076=LINE('',#27396,#5957);
#4077=LINE('',#27398,#5958);
#4078=LINE('',#27399,#5959);
#4079=LINE('',#27404,#5960);
#4080=LINE('',#27410,#5961);
#4081=LINE('',#27415,#5962);
#4082=LINE('',#27417,#5963);
#4083=LINE('',#27419,#5964);
#4084=LINE('',#27421,#5965);
#4085=LINE('',#27423,#5966);
#4086=LINE('',#27427,#5967);
#4087=LINE('',#27431,#5968);
#4088=LINE('',#27434,#5969);
#4089=LINE('',#27436,#5970);
#4090=LINE('',#27444,#5971);
#4091=LINE('',#27452,#5972);
#4092=LINE('',#27456,#5973);
#4093=LINE('',#27460,#5974);
#4094=LINE('',#27462,#5975);
#4095=LINE('',#27464,#5976);
#4096=LINE('',#27466,#5977);
#4097=LINE('',#27468,#5978);
#4098=LINE('',#27470,#5979);
#4099=LINE('',#27472,#5980);
#4100=LINE('',#27474,#5981);
#4101=LINE('',#27478,#5982);
#4102=LINE('',#27482,#5983);
#4103=LINE('',#27484,#5984);
#4104=LINE('',#27485,#5985);
#4105=LINE('',#27488,#5986);
#4106=LINE('',#27490,#5987);
#4107=LINE('',#27491,#5988);
#4108=LINE('',#27494,#5989);
#4109=LINE('',#27495,#5990);
#4110=LINE('',#27498,#5991);
#4111=LINE('',#27499,#5992);
#4112=LINE('',#27502,#5993);
#4113=LINE('',#27503,#5994);
#4114=LINE('',#27510,#5995);
#4115=LINE('',#27514,#5996);
#4116=LINE('',#27515,#5997);
#4117=LINE('',#27520,#5998);
#4118=LINE('',#27522,#5999);
#4119=LINE('',#27524,#6000);
#4120=LINE('',#27526,#6001);
#4121=LINE('',#27528,#6002);
#4122=LINE('',#27530,#6003);
#4123=LINE('',#27532,#6004);
#4124=LINE('',#27534,#6005);
#4125=LINE('',#27538,#6006);
#4126=LINE('',#27542,#6007);
#4127=LINE('',#27550,#6008);
#4128=LINE('',#27558,#6009);
#4129=LINE('',#27559,#6010);
#4130=LINE('',#27563,#6011);
#4131=LINE('',#27567,#6012);
#4132=LINE('',#27571,#6013);
#4133=LINE('',#27573,#6014);
#4134=LINE('',#27575,#6015);
#4135=LINE('',#27576,#6016);
#4136=LINE('',#27578,#6017);
#4137=LINE('',#27579,#6018);
#4138=LINE('',#27581,#6019);
#4139=LINE('',#27583,#6020);
#4140=LINE('',#27585,#6021);
#4141=LINE('',#27593,#6022);
#4142=LINE('',#27597,#6023);
#4143=LINE('',#27601,#6024);
#4144=LINE('',#27605,#6025);
#4145=LINE('',#27608,#6026);
#4146=LINE('',#27610,#6027);
#4147=LINE('',#27612,#6028);
#4148=LINE('',#27614,#6029);
#4149=LINE('',#27616,#6030);
#4150=LINE('',#27618,#6031);
#4151=LINE('',#27620,#6032);
#4152=LINE('',#27622,#6033);
#4153=LINE('',#27625,#6034);
#4154=LINE('',#27627,#6035);
#4155=LINE('',#27629,#6036);
#4156=LINE('',#27631,#6037);
#4157=LINE('',#27633,#6038);
#4158=LINE('',#27635,#6039);
#4159=LINE('',#27637,#6040);
#4160=LINE('',#27639,#6041);
#4161=LINE('',#27641,#6042);
#4162=LINE('',#27643,#6043);
#4163=LINE('',#27645,#6044);
#4164=LINE('',#27647,#6045);
#4165=LINE('',#27649,#6046);
#4166=LINE('',#27651,#6047);
#4167=LINE('',#27653,#6048);
#4168=LINE('',#27655,#6049);
#4169=LINE('',#27662,#6050);
#4170=LINE('',#27665,#6051);
#4171=LINE('',#27668,#6052);
#4172=LINE('',#27670,#6053);
#4173=LINE('',#27671,#6054);
#4174=LINE('',#27676,#6055);
#4175=LINE('',#27680,#6056);
#4176=LINE('',#27682,#6057);
#4177=LINE('',#27683,#6058);
#4178=LINE('',#27688,#6059);
#4179=LINE('',#27692,#6060);
#4180=LINE('',#27694,#6061);
#4181=LINE('',#27695,#6062);
#4182=LINE('',#27698,#6063);
#4183=LINE('',#27700,#6064);
#4184=LINE('',#27701,#6065);
#4185=LINE('',#27704,#6066);
#4186=LINE('',#27706,#6067);
#4187=LINE('',#27707,#6068);
#4188=LINE('',#27711,#6069);
#4189=LINE('',#27713,#6070);
#4190=LINE('',#27715,#6071);
#4191=LINE('',#27716,#6072);
#4192=LINE('',#27719,#6073);
#4193=LINE('',#27721,#6074);
#4194=LINE('',#27722,#6075);
#4195=LINE('',#27725,#6076);
#4196=LINE('',#27727,#6077);
#4197=LINE('',#27728,#6078);
#4198=LINE('',#27731,#6079);
#4199=LINE('',#27733,#6080);
#4200=LINE('',#27734,#6081);
#4201=LINE('',#27737,#6082);
#4202=LINE('',#27739,#6083);
#4203=LINE('',#27740,#6084);
#4204=LINE('',#27743,#6085);
#4205=LINE('',#27745,#6086);
#4206=LINE('',#27746,#6087);
#4207=LINE('',#27749,#6088);
#4208=LINE('',#27751,#6089);
#4209=LINE('',#27752,#6090);
#4210=LINE('',#27757,#6091);
#4211=LINE('',#27764,#6092);
#4212=LINE('',#27772,#6093);
#4213=LINE('',#27780,#6094);
#4214=LINE('',#27782,#6095);
#4215=LINE('',#27784,#6096);
#4216=LINE('',#27792,#6097);
#4217=LINE('',#27796,#6098);
#4218=LINE('',#27797,#6099);
#4219=LINE('',#27799,#6100);
#4220=LINE('',#27802,#6101);
#4221=LINE('',#27803,#6102);
#4222=LINE('',#27807,#6103);
#4223=LINE('',#27810,#6104);
#4224=LINE('',#27811,#6105);
#4225=LINE('',#27815,#6106);
#4226=LINE('',#27819,#6107);
#4227=LINE('',#27823,#6108);
#4228=LINE('',#27826,#6109);
#4229=LINE('',#27827,#6110);
#4230=LINE('',#27831,#6111);
#4231=LINE('',#27835,#6112);
#4232=LINE('',#27839,#6113);
#4233=LINE('',#27842,#6114);
#4234=LINE('',#27843,#6115);
#4235=LINE('',#27846,#6116);
#4236=LINE('',#27847,#6117);
#4237=LINE('',#27850,#6118);
#4238=LINE('',#27851,#6119);
#4239=LINE('',#27855,#6120);
#4240=LINE('',#27859,#6121);
#4241=LINE('',#27863,#6122);
#4242=LINE('',#27866,#6123);
#4243=LINE('',#27867,#6124);
#4244=LINE('',#27871,#6125);
#4245=LINE('',#27879,#6126);
#4246=LINE('',#27881,#6127);
#4247=LINE('',#27883,#6128);
#4248=LINE('',#27885,#6129);
#4249=LINE('',#27887,#6130);
#4250=LINE('',#27889,#6131);
#4251=LINE('',#27891,#6132);
#4252=LINE('',#27893,#6133);
#4253=LINE('',#27897,#6134);
#4254=LINE('',#27901,#6135);
#4255=LINE('',#27909,#6136);
#4256=LINE('',#27917,#6137);
#4257=LINE('',#27919,#6138);
#4258=LINE('',#27921,#6139);
#4259=LINE('',#27929,#6140);
#4260=LINE('',#27937,#6141);
#4261=LINE('',#27941,#6142);
#4262=LINE('',#27945,#6143);
#4263=LINE('',#27947,#6144);
#4264=LINE('',#27948,#6145);
#4265=LINE('',#27951,#6146);
#4266=LINE('',#27953,#6147);
#4267=LINE('',#27954,#6148);
#4268=LINE('',#27957,#6149);
#4269=LINE('',#27961,#6150);
#4270=LINE('',#27965,#6151);
#4271=LINE('',#27969,#6152);
#4272=LINE('',#27970,#6153);
#4273=LINE('',#27973,#6154);
#4274=LINE('',#27977,#6155);
#4275=LINE('',#27981,#6156);
#4276=LINE('',#27985,#6157);
#4277=LINE('',#27986,#6158);
#4278=LINE('',#27989,#6159);
#4279=LINE('',#27993,#6160);
#4280=LINE('',#27994,#6161);
#4281=LINE('',#27997,#6162);
#4282=LINE('',#28001,#6163);
#4283=LINE('',#28002,#6164);
#4284=LINE('',#28005,#6165);
#4285=LINE('',#28006,#6166);
#4286=LINE('',#28009,#6167);
#4287=LINE('',#28010,#6168);
#4288=LINE('',#28013,#6169);
#4289=LINE('',#28014,#6170);
#4290=LINE('',#28017,#6171);
#4291=LINE('',#28019,#6172);
#4292=LINE('',#28020,#6173);
#4293=LINE('',#28023,#6174);
#4294=LINE('',#28024,#6175);
#4295=LINE('',#28027,#6176);
#4296=LINE('',#28028,#6177);
#4297=LINE('',#28031,#6178);
#4298=LINE('',#28032,#6179);
#4299=LINE('',#28035,#6180);
#4300=LINE('',#28039,#6181);
#4301=LINE('',#28040,#6182);
#4302=LINE('',#28043,#6183);
#4303=LINE('',#28044,#6184);
#4304=LINE('',#28046,#6185);
#4305=LINE('',#28049,#6186);
#4306=LINE('',#28050,#6187);
#4307=LINE('',#28053,#6188);
#4308=LINE('',#28054,#6189);
#4309=LINE('',#28057,#6190);
#4310=LINE('',#28058,#6191);
#4311=LINE('',#28062,#6192);
#4312=LINE('',#28066,#6193);
#4313=LINE('',#28070,#6194);
#4314=LINE('',#28073,#6195);
#4315=LINE('',#28074,#6196);
#4316=LINE('',#28078,#6197);
#4317=LINE('',#28082,#6198);
#4318=LINE('',#28086,#6199);
#4319=LINE('',#28089,#6200);
#4320=LINE('',#28090,#6201);
#4321=LINE('',#28097,#6202);
#4322=LINE('',#28099,#6203);
#4323=LINE('',#28101,#6204);
#4324=LINE('',#28102,#6205);
#4325=LINE('',#28108,#6206);
#4326=LINE('',#28114,#6207);
#4327=LINE('',#28120,#6208);
#4328=LINE('',#28123,#6209);
#4329=LINE('',#28125,#6210);
#4330=LINE('',#28126,#6211);
#4331=LINE('',#28132,#6212);
#4332=LINE('',#28138,#6213);
#4333=LINE('',#28142,#6214);
#4334=LINE('',#28144,#6215);
#4335=LINE('',#28146,#6216);
#4336=LINE('',#28148,#6217);
#4337=LINE('',#28152,#6218);
#4338=LINE('',#28156,#6219);
#4339=LINE('',#28158,#6220);
#4340=LINE('',#28160,#6221);
#4341=LINE('',#28162,#6222);
#4342=LINE('',#28164,#6223);
#4343=LINE('',#28166,#6224);
#4344=LINE('',#28168,#6225);
#4345=LINE('',#28170,#6226);
#4346=LINE('',#28174,#6227);
#4347=LINE('',#28178,#6228);
#4348=LINE('',#28186,#6229);
#4349=LINE('',#28194,#6230);
#4350=LINE('',#28195,#6231);
#4351=LINE('',#28199,#6232);
#4352=LINE('',#28203,#6233);
#4353=LINE('',#28207,#6234);
#4354=LINE('',#28209,#6235);
#4355=LINE('',#28211,#6236);
#4356=LINE('',#28212,#6237);
#4357=LINE('',#28215,#6238);
#4358=LINE('',#28217,#6239);
#4359=LINE('',#28218,#6240);
#4360=LINE('',#28221,#6241);
#4361=LINE('',#28222,#6242);
#4362=LINE('',#28225,#6243);
#4363=LINE('',#28226,#6244);
#4364=LINE('',#28229,#6245);
#4365=LINE('',#28230,#6246);
#4366=LINE('',#28237,#6247);
#4367=LINE('',#28241,#6248);
#4368=LINE('',#28242,#6249);
#4369=LINE('',#28245,#6250);
#4370=LINE('',#28247,#6251);
#4371=LINE('',#28249,#6252);
#4372=LINE('',#28251,#6253);
#4373=LINE('',#28255,#6254);
#4374=LINE('',#28259,#6255);
#4375=LINE('',#28262,#6256);
#4376=LINE('',#28264,#6257);
#4377=LINE('',#28272,#6258);
#4378=LINE('',#28280,#6259);
#4379=LINE('',#28284,#6260);
#4380=LINE('',#28288,#6261);
#4381=LINE('',#28290,#6262);
#4382=LINE('',#28292,#6263);
#4383=LINE('',#28294,#6264);
#4384=LINE('',#28296,#6265);
#4385=LINE('',#28298,#6266);
#4386=LINE('',#28300,#6267);
#4387=LINE('',#28302,#6268);
#4388=LINE('',#28305,#6269);
#4389=LINE('',#28306,#6270);
#4390=LINE('',#28308,#6271);
#4391=LINE('',#28310,#6272);
#4392=LINE('',#28312,#6273);
#4393=LINE('',#28320,#6274);
#4394=LINE('',#28324,#6275);
#4395=LINE('',#28328,#6276);
#4396=LINE('',#28332,#6277);
#4397=LINE('',#28335,#6278);
#4398=LINE('',#28337,#6279);
#4399=LINE('',#28339,#6280);
#4400=LINE('',#28341,#6281);
#4401=LINE('',#28343,#6282);
#4402=LINE('',#28345,#6283);
#4403=LINE('',#28347,#6284);
#4404=LINE('',#28349,#6285);
#4405=LINE('',#28352,#6286);
#4406=LINE('',#28354,#6287);
#4407=LINE('',#28356,#6288);
#4408=LINE('',#28358,#6289);
#4409=LINE('',#28360,#6290);
#4410=LINE('',#28362,#6291);
#4411=LINE('',#28364,#6292);
#4412=LINE('',#28366,#6293);
#4413=LINE('',#28368,#6294);
#4414=LINE('',#28370,#6295);
#4415=LINE('',#28372,#6296);
#4416=LINE('',#28374,#6297);
#4417=LINE('',#28376,#6298);
#4418=LINE('',#28378,#6299);
#4419=LINE('',#28380,#6300);
#4420=LINE('',#28382,#6301);
#4421=LINE('',#28389,#6302);
#4422=LINE('',#28392,#6303);
#4423=LINE('',#28395,#6304);
#4424=LINE('',#28397,#6305);
#4425=LINE('',#28398,#6306);
#4426=LINE('',#28404,#6307);
#4427=LINE('',#28407,#6308);
#4428=LINE('',#28409,#6309);
#4429=LINE('',#28410,#6310);
#4430=LINE('',#28416,#6311);
#4431=LINE('',#28419,#6312);
#4432=LINE('',#28421,#6313);
#4433=LINE('',#28422,#6314);
#4434=LINE('',#28425,#6315);
#4435=LINE('',#28427,#6316);
#4436=LINE('',#28428,#6317);
#4437=LINE('',#28431,#6318);
#4438=LINE('',#28433,#6319);
#4439=LINE('',#28434,#6320);
#4440=LINE('',#28438,#6321);
#4441=LINE('',#28440,#6322);
#4442=LINE('',#28442,#6323);
#4443=LINE('',#28443,#6324);
#4444=LINE('',#28446,#6325);
#4445=LINE('',#28448,#6326);
#4446=LINE('',#28449,#6327);
#4447=LINE('',#28452,#6328);
#4448=LINE('',#28454,#6329);
#4449=LINE('',#28455,#6330);
#4450=LINE('',#28458,#6331);
#4451=LINE('',#28460,#6332);
#4452=LINE('',#28461,#6333);
#4453=LINE('',#28464,#6334);
#4454=LINE('',#28466,#6335);
#4455=LINE('',#28467,#6336);
#4456=LINE('',#28470,#6337);
#4457=LINE('',#28472,#6338);
#4458=LINE('',#28473,#6339);
#4459=LINE('',#28476,#6340);
#4460=LINE('',#28478,#6341);
#4461=LINE('',#28479,#6342);
#4462=LINE('',#28485,#6343);
#4463=LINE('',#28490,#6344);
#4464=LINE('',#28491,#6345);
#4465=LINE('',#28497,#6346);
#4466=LINE('',#28505,#6347);
#4467=LINE('',#28507,#6348);
#4468=LINE('',#28509,#6349);
#4469=LINE('',#28517,#6350);
#4470=LINE('',#28524,#6351);
#4471=LINE('',#28526,#6352);
#4472=LINE('',#28529,#6353);
#4473=LINE('',#28530,#6354);
#4474=LINE('',#28534,#6355);
#4475=LINE('',#28537,#6356);
#4476=LINE('',#28538,#6357);
#4477=LINE('',#28542,#6358);
#4478=LINE('',#28546,#6359);
#4479=LINE('',#28550,#6360);
#4480=LINE('',#28553,#6361);
#4481=LINE('',#28554,#6362);
#4482=LINE('',#28558,#6363);
#4483=LINE('',#28562,#6364);
#4484=LINE('',#28566,#6365);
#4485=LINE('',#28569,#6366);
#4486=LINE('',#28570,#6367);
#4487=LINE('',#28573,#6368);
#4488=LINE('',#28574,#6369);
#4489=LINE('',#28577,#6370);
#4490=LINE('',#28578,#6371);
#4491=LINE('',#28582,#6372);
#4492=LINE('',#28586,#6373);
#4493=LINE('',#28590,#6374);
#4494=LINE('',#28593,#6375);
#4495=LINE('',#28594,#6376);
#4496=LINE('',#28598,#6377);
#4497=LINE('',#28607,#6378);
#4498=LINE('',#28622,#6379);
#4499=LINE('',#28663,#6380);
#4500=LINE('',#28739,#6381);
#4501=LINE('',#28742,#6382);
#4502=LINE('',#28747,#6383);
#4503=LINE('',#28748,#6384);
#4504=LINE('',#28751,#6385);
#4505=LINE('',#28754,#6386);
#4506=LINE('',#28757,#6387);
#4507=LINE('',#28760,#6388);
#4508=LINE('',#28763,#6389);
#4509=LINE('',#28766,#6390);
#4510=LINE('',#28769,#6391);
#4511=LINE('',#28772,#6392);
#4512=LINE('',#28775,#6393);
#4513=LINE('',#28778,#6394);
#4514=LINE('',#28783,#6395);
#4515=LINE('',#28784,#6396);
#4516=LINE('',#28787,#6397);
#4517=LINE('',#28790,#6398);
#4518=LINE('',#28795,#6399);
#4519=LINE('',#28796,#6400);
#4520=LINE('',#28799,#6401);
#4521=LINE('',#28802,#6402);
#4522=LINE('',#28805,#6403);
#4523=LINE('',#28808,#6404);
#4524=LINE('',#28811,#6405);
#4525=LINE('',#28814,#6406);
#4526=LINE('',#28817,#6407);
#4527=LINE('',#28820,#6408);
#4528=LINE('',#28823,#6409);
#4529=LINE('',#28826,#6410);
#4530=LINE('',#28831,#6411);
#4531=LINE('',#28832,#6412);
#4532=LINE('',#28834,#6413);
#4533=LINE('',#28835,#6414);
#4534=LINE('',#28837,#6415);
#4535=LINE('',#28838,#6416);
#4536=LINE('',#28840,#6417);
#4537=LINE('',#28841,#6418);
#4538=LINE('',#28843,#6419);
#4539=LINE('',#28844,#6420);
#4540=LINE('',#28846,#6421);
#4541=LINE('',#28847,#6422);
#4542=LINE('',#28849,#6423);
#4543=LINE('',#28850,#6424);
#4544=LINE('',#28852,#6425);
#4545=LINE('',#28853,#6426);
#4546=LINE('',#28855,#6427);
#4547=LINE('',#28856,#6428);
#4548=LINE('',#28860,#6429);
#4549=LINE('',#28862,#6430);
#4550=LINE('',#28865,#6431);
#4551=LINE('',#28867,#6432);
#4552=LINE('',#28870,#6433);
#4553=LINE('',#28872,#6434);
#4554=LINE('',#28875,#6435);
#4555=LINE('',#28877,#6436);
#4556=LINE('',#28880,#6437);
#4557=LINE('',#28882,#6438);
#4558=LINE('',#28885,#6439);
#4559=LINE('',#28887,#6440);
#4560=LINE('',#28890,#6441);
#4561=LINE('',#28892,#6442);
#4562=LINE('',#28895,#6443);
#4563=LINE('',#28897,#6444);
#4564=LINE('',#28921,#6445);
#4565=LINE('',#28925,#6446);
#4566=LINE('',#28929,#6447);
#4567=LINE('',#28948,#6448);
#4568=LINE('',#28950,#6449);
#4569=LINE('',#28963,#6450);
#4570=LINE('',#28971,#6451);
#4571=LINE('',#28978,#6452);
#4572=LINE('',#28986,#6453);
#4573=LINE('',#28989,#6454);
#4574=LINE('',#29035,#6455);
#4575=LINE('',#29050,#6456);
#4576=LINE('',#29094,#6457);
#4577=LINE('',#29165,#6458);
#4578=LINE('',#29168,#6459);
#4579=LINE('',#29173,#6460);
#4580=LINE('',#29174,#6461);
#4581=LINE('',#29177,#6462);
#4582=LINE('',#29180,#6463);
#4583=LINE('',#29183,#6464);
#4584=LINE('',#29186,#6465);
#4585=LINE('',#29189,#6466);
#4586=LINE('',#29192,#6467);
#4587=LINE('',#29195,#6468);
#4588=LINE('',#29198,#6469);
#4589=LINE('',#29201,#6470);
#4590=LINE('',#29204,#6471);
#4591=LINE('',#29209,#6472);
#4592=LINE('',#29210,#6473);
#4593=LINE('',#29213,#6474);
#4594=LINE('',#29216,#6475);
#4595=LINE('',#29221,#6476);
#4596=LINE('',#29222,#6477);
#4597=LINE('',#29225,#6478);
#4598=LINE('',#29228,#6479);
#4599=LINE('',#29231,#6480);
#4600=LINE('',#29234,#6481);
#4601=LINE('',#29237,#6482);
#4602=LINE('',#29240,#6483);
#4603=LINE('',#29243,#6484);
#4604=LINE('',#29246,#6485);
#4605=LINE('',#29249,#6486);
#4606=LINE('',#29252,#6487);
#4607=LINE('',#29257,#6488);
#4608=LINE('',#29258,#6489);
#4609=LINE('',#29260,#6490);
#4610=LINE('',#29261,#6491);
#4611=LINE('',#29263,#6492);
#4612=LINE('',#29264,#6493);
#4613=LINE('',#29266,#6494);
#4614=LINE('',#29267,#6495);
#4615=LINE('',#29269,#6496);
#4616=LINE('',#29270,#6497);
#4617=LINE('',#29272,#6498);
#4618=LINE('',#29273,#6499);
#4619=LINE('',#29275,#6500);
#4620=LINE('',#29276,#6501);
#4621=LINE('',#29278,#6502);
#4622=LINE('',#29279,#6503);
#4623=LINE('',#29281,#6504);
#4624=LINE('',#29282,#6505);
#4625=LINE('',#29286,#6506);
#4626=LINE('',#29288,#6507);
#4627=LINE('',#29291,#6508);
#4628=LINE('',#29293,#6509);
#4629=LINE('',#29296,#6510);
#4630=LINE('',#29298,#6511);
#4631=LINE('',#29301,#6512);
#4632=LINE('',#29303,#6513);
#4633=LINE('',#29306,#6514);
#4634=LINE('',#29308,#6515);
#4635=LINE('',#29311,#6516);
#4636=LINE('',#29313,#6517);
#4637=LINE('',#29316,#6518);
#4638=LINE('',#29318,#6519);
#4639=LINE('',#29321,#6520);
#4640=LINE('',#29323,#6521);
#4641=LINE('',#29329,#6522);
#4642=LINE('',#29331,#6523);
#4643=LINE('',#29333,#6524);
#4644=LINE('',#29334,#6525);
#4645=LINE('',#29337,#6526);
#4646=LINE('',#29339,#6527);
#4647=LINE('',#29340,#6528);
#4648=LINE('',#29343,#6529);
#4649=LINE('',#29345,#6530);
#4650=LINE('',#29346,#6531);
#4651=LINE('',#29350,#6532);
#4652=LINE('',#29352,#6533);
#4653=LINE('',#29354,#6534);
#4654=LINE('',#29355,#6535);
#4655=LINE('',#29358,#6536);
#4656=LINE('',#29360,#6537);
#4657=LINE('',#29361,#6538);
#4658=LINE('',#29364,#6539);
#4659=LINE('',#29366,#6540);
#4660=LINE('',#29367,#6541);
#4661=LINE('',#29370,#6542);
#4662=LINE('',#29372,#6543);
#4663=LINE('',#29373,#6544);
#4664=LINE('',#29376,#6545);
#4665=LINE('',#29378,#6546);
#4666=LINE('',#29379,#6547);
#4667=LINE('',#29382,#6548);
#4668=LINE('',#29384,#6549);
#4669=LINE('',#29385,#6550);
#4670=LINE('',#29389,#6551);
#4671=LINE('',#29391,#6552);
#4672=LINE('',#29393,#6553);
#4673=LINE('',#29394,#6554);
#4674=LINE('',#29397,#6555);
#4675=LINE('',#29399,#6556);
#4676=LINE('',#29400,#6557);
#4677=LINE('',#29403,#6558);
#4678=LINE('',#29405,#6559);
#4679=LINE('',#29406,#6560);
#4680=LINE('',#29409,#6561);
#4681=LINE('',#29411,#6562);
#4682=LINE('',#29412,#6563);
#4683=LINE('',#29416,#6564);
#4684=LINE('',#29418,#6565);
#4685=LINE('',#29420,#6566);
#4686=LINE('',#29421,#6567);
#4687=LINE('',#29424,#6568);
#4688=LINE('',#29426,#6569);
#4689=LINE('',#29427,#6570);
#4690=LINE('',#29430,#6571);
#4691=LINE('',#29432,#6572);
#4692=LINE('',#29433,#6573);
#4693=LINE('',#29436,#6574);
#4694=LINE('',#29438,#6575);
#4695=LINE('',#29439,#6576);
#4696=LINE('',#29442,#6577);
#4697=LINE('',#29444,#6578);
#4698=LINE('',#29445,#6579);
#4699=LINE('',#29447,#6580);
#4700=LINE('',#29448,#6581);
#4701=LINE('',#29452,#6582);
#4702=LINE('',#29454,#6583);
#4703=LINE('',#29456,#6584);
#4704=LINE('',#29457,#6585);
#4705=LINE('',#29460,#6586);
#4706=LINE('',#29462,#6587);
#4707=LINE('',#29463,#6588);
#4708=LINE('',#29466,#6589);
#4709=LINE('',#29468,#6590);
#4710=LINE('',#29469,#6591);
#4711=LINE('',#29471,#6592);
#4712=LINE('',#29472,#6593);
#4713=LINE('',#29476,#6594);
#4714=LINE('',#29478,#6595);
#4715=LINE('',#29480,#6596);
#4716=LINE('',#29481,#6597);
#4717=LINE('',#29484,#6598);
#4718=LINE('',#29486,#6599);
#4719=LINE('',#29487,#6600);
#4720=LINE('',#29490,#6601);
#4721=LINE('',#29492,#6602);
#4722=LINE('',#29493,#6603);
#4723=LINE('',#29496,#6604);
#4724=LINE('',#29498,#6605);
#4725=LINE('',#29499,#6606);
#4726=LINE('',#29502,#6607);
#4727=LINE('',#29504,#6608);
#4728=LINE('',#29505,#6609);
#4729=LINE('',#29508,#6610);
#4730=LINE('',#29510,#6611);
#4731=LINE('',#29511,#6612);
#4732=LINE('',#29515,#6613);
#4733=LINE('',#29517,#6614);
#4734=LINE('',#29519,#6615);
#4735=LINE('',#29520,#6616);
#4736=LINE('',#29523,#6617);
#4737=LINE('',#29525,#6618);
#4738=LINE('',#29526,#6619);
#4739=LINE('',#29529,#6620);
#4740=LINE('',#29531,#6621);
#4741=LINE('',#29532,#6622);
#4742=LINE('',#29534,#6623);
#4743=LINE('',#29535,#6624);
#4744=LINE('',#29540,#6625);
#4745=LINE('',#29544,#6626);
#4746=LINE('',#29546,#6627);
#4747=LINE('',#29547,#6628);
#4748=LINE('',#29551,#6629);
#4749=LINE('',#29553,#6630);
#4750=LINE('',#29555,#6631);
#4751=LINE('',#29556,#6632);
#4752=LINE('',#29559,#6633);
#4753=LINE('',#29561,#6634);
#4754=LINE('',#29562,#6635);
#4755=LINE('',#29565,#6636);
#4756=LINE('',#29567,#6637);
#4757=LINE('',#29568,#6638);
#4758=LINE('',#29571,#6639);
#4759=LINE('',#29573,#6640);
#4760=LINE('',#29574,#6641);
#4761=LINE('',#29577,#6642);
#4762=LINE('',#29579,#6643);
#4763=LINE('',#29580,#6644);
#4764=LINE('',#29582,#6645);
#4765=LINE('',#29583,#6646);
#4766=LINE('',#29587,#6647);
#4767=LINE('',#29589,#6648);
#4768=LINE('',#29591,#6649);
#4769=LINE('',#29592,#6650);
#4770=LINE('',#29598,#6651);
#4771=LINE('',#29601,#6652);
#4772=LINE('',#29603,#6653);
#4773=LINE('',#29604,#6654);
#4774=LINE('',#29610,#6655);
#4775=LINE('',#29614,#6656);
#4776=LINE('',#29616,#6657);
#4777=LINE('',#29618,#6658);
#4778=LINE('',#29619,#6659);
#4779=LINE('',#29622,#6660);
#4780=LINE('',#29624,#6661);
#4781=LINE('',#29625,#6662);
#4782=LINE('',#29628,#6663);
#4783=LINE('',#29630,#6664);
#4784=LINE('',#29631,#6665);
#4785=LINE('',#29634,#6666);
#4786=LINE('',#29636,#6667);
#4787=LINE('',#29637,#6668);
#4788=LINE('',#29640,#6669);
#4789=LINE('',#29642,#6670);
#4790=LINE('',#29643,#6671);
#4791=LINE('',#29646,#6672);
#4792=LINE('',#29648,#6673);
#4793=LINE('',#29649,#6674);
#4794=LINE('',#29651,#6675);
#4795=LINE('',#29652,#6676);
#4796=LINE('',#29655,#6677);
#4797=LINE('',#29657,#6678);
#4798=LINE('',#29658,#6679);
#4799=LINE('',#29661,#6680);
#4800=LINE('',#29663,#6681);
#4801=LINE('',#29664,#6682);
#4802=LINE('',#29667,#6683);
#4803=LINE('',#29669,#6684);
#4804=LINE('',#29670,#6685);
#4805=LINE('',#29673,#6686);
#4806=LINE('',#29675,#6687);
#4807=LINE('',#29676,#6688);
#4808=LINE('',#29681,#6689);
#4809=LINE('',#29685,#6690);
#4810=LINE('',#29687,#6691);
#4811=LINE('',#29688,#6692);
#4812=LINE('',#29693,#6693);
#4813=LINE('',#29696,#6694);
#4814=LINE('',#29697,#6695);
#4815=LINE('',#29700,#6696);
#4816=LINE('',#29702,#6697);
#4817=LINE('',#29703,#6698);
#4818=LINE('',#29706,#6699);
#4819=LINE('',#29708,#6700);
#4820=LINE('',#29709,#6701);
#4821=LINE('',#29712,#6702);
#4822=LINE('',#29714,#6703);
#4823=LINE('',#29715,#6704);
#4824=LINE('',#29718,#6705);
#4825=LINE('',#29720,#6706);
#4826=LINE('',#29721,#6707);
#4827=LINE('',#29724,#6708);
#4828=LINE('',#29726,#6709);
#4829=LINE('',#29727,#6710);
#4830=LINE('',#29730,#6711);
#4831=LINE('',#29732,#6712);
#4832=LINE('',#29733,#6713);
#4833=LINE('',#29736,#6714);
#4834=LINE('',#29738,#6715);
#4835=LINE('',#29739,#6716);
#4836=LINE('',#29742,#6717);
#4837=LINE('',#29744,#6718);
#4838=LINE('',#29745,#6719);
#4839=LINE('',#29750,#6720);
#4840=LINE('',#29754,#6721);
#4841=LINE('',#29756,#6722);
#4842=LINE('',#29757,#6723);
#4843=LINE('',#29760,#6724);
#4844=LINE('',#29762,#6725);
#4845=LINE('',#29763,#6726);
#4846=LINE('',#29766,#6727);
#4847=LINE('',#29768,#6728);
#4848=LINE('',#29769,#6729);
#4849=LINE('',#29772,#6730);
#4850=LINE('',#29774,#6731);
#4851=LINE('',#29775,#6732);
#4852=LINE('',#29778,#6733);
#4853=LINE('',#29780,#6734);
#4854=LINE('',#29781,#6735);
#4855=LINE('',#29784,#6736);
#4856=LINE('',#29786,#6737);
#4857=LINE('',#29787,#6738);
#4858=LINE('',#29790,#6739);
#4859=LINE('',#29792,#6740);
#4860=LINE('',#29793,#6741);
#4861=LINE('',#29797,#6742);
#4862=LINE('',#29799,#6743);
#4863=LINE('',#29801,#6744);
#4864=LINE('',#29802,#6745);
#4865=LINE('',#29807,#6746);
#4866=LINE('',#29811,#6747);
#4867=LINE('',#29813,#6748);
#4868=LINE('',#29814,#6749);
#4869=LINE('',#29819,#6750);
#4870=LINE('',#29824,#6751);
#4871=LINE('',#29826,#6752);
#4872=LINE('',#29828,#6753);
#4873=LINE('',#29829,#6754);
#4874=LINE('',#29832,#6755);
#4875=LINE('',#29834,#6756);
#4876=LINE('',#29835,#6757);
#4877=LINE('',#29838,#6758);
#4878=LINE('',#29840,#6759);
#4879=LINE('',#29841,#6760);
#4880=LINE('',#29844,#6761);
#4881=LINE('',#29846,#6762);
#4882=LINE('',#29847,#6763);
#4883=LINE('',#29850,#6764);
#4884=LINE('',#29852,#6765);
#4885=LINE('',#29853,#6766);
#4886=LINE('',#29856,#6767);
#4887=LINE('',#29858,#6768);
#4888=LINE('',#29859,#6769);
#4889=LINE('',#29861,#6770);
#4890=LINE('',#29862,#6771);
#4891=LINE('',#29865,#6772);
#4892=LINE('',#29867,#6773);
#4893=LINE('',#29868,#6774);
#4894=LINE('',#29871,#6775);
#4895=LINE('',#29873,#6776);
#4896=LINE('',#29874,#6777);
#4897=LINE('',#29877,#6778);
#4898=LINE('',#29879,#6779);
#4899=LINE('',#29880,#6780);
#4900=LINE('',#29883,#6781);
#4901=LINE('',#29885,#6782);
#4902=LINE('',#29886,#6783);
#4903=LINE('',#29888,#6784);
#4904=LINE('',#29889,#6785);
#4905=LINE('',#29894,#6786);
#4906=LINE('',#29898,#6787);
#4907=LINE('',#29900,#6788);
#4908=LINE('',#29901,#6789);
#4909=LINE('',#29907,#6790);
#4910=LINE('',#29910,#6791);
#4911=LINE('',#29912,#6792);
#4912=LINE('',#29913,#6793);
#4913=LINE('',#29919,#6794);
#4914=LINE('',#29921,#6795);
#4915=LINE('',#29922,#6796);
#4916=LINE('',#29925,#6797);
#4917=LINE('',#29927,#6798);
#4918=LINE('',#29928,#6799);
#4919=LINE('',#29931,#6800);
#4920=LINE('',#29933,#6801);
#4921=LINE('',#29934,#6802);
#4922=LINE('',#29937,#6803);
#4923=LINE('',#29939,#6804);
#4924=LINE('',#29940,#6805);
#4925=LINE('',#29943,#6806);
#4926=LINE('',#29945,#6807);
#4927=LINE('',#29946,#6808);
#4928=LINE('',#29949,#6809);
#4929=LINE('',#29951,#6810);
#4930=LINE('',#29952,#6811);
#4931=LINE('',#29955,#6812);
#4932=LINE('',#29957,#6813);
#4933=LINE('',#29958,#6814);
#4934=LINE('',#29961,#6815);
#4935=LINE('',#29963,#6816);
#4936=LINE('',#29964,#6817);
#4937=LINE('',#29967,#6818);
#4938=LINE('',#29969,#6819);
#4939=LINE('',#29970,#6820);
#4940=LINE('',#29976,#6821);
#4941=LINE('',#29979,#6822);
#4942=LINE('',#29981,#6823);
#4943=LINE('',#29982,#6824);
#4944=LINE('',#29985,#6825);
#4945=LINE('',#29987,#6826);
#4946=LINE('',#29988,#6827);
#4947=LINE('',#29991,#6828);
#4948=LINE('',#29993,#6829);
#4949=LINE('',#29994,#6830);
#4950=LINE('',#29997,#6831);
#4951=LINE('',#29999,#6832);
#4952=LINE('',#30000,#6833);
#4953=LINE('',#30003,#6834);
#4954=LINE('',#30005,#6835);
#4955=LINE('',#30006,#6836);
#4956=LINE('',#30009,#6837);
#4957=LINE('',#30011,#6838);
#4958=LINE('',#30012,#6839);
#4959=LINE('',#30014,#6840);
#4960=LINE('',#30015,#6841);
#4961=LINE('',#30019,#6842);
#4962=LINE('',#30021,#6843);
#4963=LINE('',#30023,#6844);
#4964=LINE('',#30024,#6845);
#4965=LINE('',#30027,#6846);
#4966=LINE('',#30029,#6847);
#4967=LINE('',#30030,#6848);
#4968=LINE('',#30033,#6849);
#4969=LINE('',#30035,#6850);
#4970=LINE('',#30036,#6851);
#4971=LINE('',#30040,#6852);
#4972=LINE('',#30042,#6853);
#4973=LINE('',#30044,#6854);
#4974=LINE('',#30045,#6855);
#4975=LINE('',#30048,#6856);
#4976=LINE('',#30050,#6857);
#4977=LINE('',#30051,#6858);
#4978=LINE('',#30054,#6859);
#4979=LINE('',#30056,#6860);
#4980=LINE('',#30057,#6861);
#4981=LINE('',#30060,#6862);
#4982=LINE('',#30062,#6863);
#4983=LINE('',#30063,#6864);
#4984=LINE('',#30066,#6865);
#4985=LINE('',#30068,#6866);
#4986=LINE('',#30069,#6867);
#4987=LINE('',#30072,#6868);
#4988=LINE('',#30074,#6869);
#4989=LINE('',#30075,#6870);
#4990=LINE('',#30078,#6871);
#4991=LINE('',#30080,#6872);
#4992=LINE('',#30081,#6873);
#4993=LINE('',#30084,#6874);
#4994=LINE('',#30086,#6875);
#4995=LINE('',#30087,#6876);
#4996=LINE('',#30090,#6877);
#4997=LINE('',#30092,#6878);
#4998=LINE('',#30093,#6879);
#4999=LINE('',#30096,#6880);
#5000=LINE('',#30098,#6881);
#5001=LINE('',#30099,#6882);
#5002=LINE('',#30102,#6883);
#5003=LINE('',#30104,#6884);
#5004=LINE('',#30105,#6885);
#5005=LINE('',#30108,#6886);
#5006=LINE('',#30110,#6887);
#5007=LINE('',#30111,#6888);
#5008=LINE('',#30114,#6889);
#5009=LINE('',#30116,#6890);
#5010=LINE('',#30117,#6891);
#5011=LINE('',#30120,#6892);
#5012=LINE('',#30122,#6893);
#5013=LINE('',#30123,#6894);
#5014=LINE('',#30126,#6895);
#5015=LINE('',#30128,#6896);
#5016=LINE('',#30129,#6897);
#5017=LINE('',#30132,#6898);
#5018=LINE('',#30134,#6899);
#5019=LINE('',#30135,#6900);
#5020=LINE('',#30138,#6901);
#5021=LINE('',#30140,#6902);
#5022=LINE('',#30141,#6903);
#5023=LINE('',#30143,#6904);
#5024=LINE('',#30144,#6905);
#5025=LINE('',#30148,#6906);
#5026=LINE('',#30150,#6907);
#5027=LINE('',#30152,#6908);
#5028=LINE('',#30153,#6909);
#5029=LINE('',#30156,#6910);
#5030=LINE('',#30158,#6911);
#5031=LINE('',#30159,#6912);
#5032=LINE('',#30162,#6913);
#5033=LINE('',#30164,#6914);
#5034=LINE('',#30165,#6915);
#5035=LINE('',#30167,#6916);
#5036=LINE('',#30168,#6917);
#5037=LINE('',#30172,#6918);
#5038=LINE('',#30174,#6919);
#5039=LINE('',#30176,#6920);
#5040=LINE('',#30177,#6921);
#5041=LINE('',#30180,#6922);
#5042=LINE('',#30182,#6923);
#5043=LINE('',#30183,#6924);
#5044=LINE('',#30186,#6925);
#5045=LINE('',#30188,#6926);
#5046=LINE('',#30189,#6927);
#5047=LINE('',#30192,#6928);
#5048=LINE('',#30194,#6929);
#5049=LINE('',#30195,#6930);
#5050=LINE('',#30198,#6931);
#5051=LINE('',#30200,#6932);
#5052=LINE('',#30201,#6933);
#5053=LINE('',#30204,#6934);
#5054=LINE('',#30206,#6935);
#5055=LINE('',#30207,#6936);
#5056=LINE('',#30210,#6937);
#5057=LINE('',#30212,#6938);
#5058=LINE('',#30213,#6939);
#5059=LINE('',#30216,#6940);
#5060=LINE('',#30218,#6941);
#5061=LINE('',#30219,#6942);
#5062=LINE('',#30222,#6943);
#5063=LINE('',#30224,#6944);
#5064=LINE('',#30225,#6945);
#5065=LINE('',#30228,#6946);
#5066=LINE('',#30230,#6947);
#5067=LINE('',#30231,#6948);
#5068=LINE('',#30233,#6949);
#5069=LINE('',#30234,#6950);
#5070=LINE('',#30239,#6951);
#5071=LINE('',#30243,#6952);
#5072=LINE('',#30245,#6953);
#5073=LINE('',#30246,#6954);
#5074=LINE('',#30249,#6955);
#5075=LINE('',#30251,#6956);
#5076=LINE('',#30252,#6957);
#5077=LINE('',#30255,#6958);
#5078=LINE('',#30257,#6959);
#5079=LINE('',#30258,#6960);
#5080=LINE('',#30261,#6961);
#5081=LINE('',#30263,#6962);
#5082=LINE('',#30264,#6963);
#5083=LINE('',#30267,#6964);
#5084=LINE('',#30269,#6965);
#5085=LINE('',#30270,#6966);
#5086=LINE('',#30273,#6967);
#5087=LINE('',#30275,#6968);
#5088=LINE('',#30276,#6969);
#5089=LINE('',#30279,#6970);
#5090=LINE('',#30281,#6971);
#5091=LINE('',#30282,#6972);
#5092=LINE('',#30284,#6973);
#5093=LINE('',#30285,#6974);
#5094=LINE('',#30289,#6975);
#5095=LINE('',#30291,#6976);
#5096=LINE('',#30293,#6977);
#5097=LINE('',#30294,#6978);
#5098=LINE('',#30297,#6979);
#5099=LINE('',#30299,#6980);
#5100=LINE('',#30300,#6981);
#5101=LINE('',#30303,#6982);
#5102=LINE('',#30305,#6983);
#5103=LINE('',#30306,#6984);
#5104=LINE('',#30310,#6985);
#5105=LINE('',#30312,#6986);
#5106=LINE('',#30314,#6987);
#5107=LINE('',#30315,#6988);
#5108=LINE('',#30318,#6989);
#5109=LINE('',#30320,#6990);
#5110=LINE('',#30321,#6991);
#5111=LINE('',#30324,#6992);
#5112=LINE('',#30326,#6993);
#5113=LINE('',#30327,#6994);
#5114=LINE('',#30330,#6995);
#5115=LINE('',#30332,#6996);
#5116=LINE('',#30333,#6997);
#5117=LINE('',#30336,#6998);
#5118=LINE('',#30338,#6999);
#5119=LINE('',#30339,#7000);
#5120=LINE('',#30342,#7001);
#5121=LINE('',#30344,#7002);
#5122=LINE('',#30345,#7003);
#5123=LINE('',#30348,#7004);
#5124=LINE('',#30350,#7005);
#5125=LINE('',#30351,#7006);
#5126=LINE('',#30354,#7007);
#5127=LINE('',#30356,#7008);
#5128=LINE('',#30357,#7009);
#5129=LINE('',#30360,#7010);
#5130=LINE('',#30362,#7011);
#5131=LINE('',#30363,#7012);
#5132=LINE('',#30366,#7013);
#5133=LINE('',#30368,#7014);
#5134=LINE('',#30369,#7015);
#5135=LINE('',#30372,#7016);
#5136=LINE('',#30374,#7017);
#5137=LINE('',#30375,#7018);
#5138=LINE('',#30378,#7019);
#5139=LINE('',#30380,#7020);
#5140=LINE('',#30381,#7021);
#5141=LINE('',#30384,#7022);
#5142=LINE('',#30386,#7023);
#5143=LINE('',#30387,#7024);
#5144=LINE('',#30390,#7025);
#5145=LINE('',#30392,#7026);
#5146=LINE('',#30393,#7027);
#5147=LINE('',#30396,#7028);
#5148=LINE('',#30398,#7029);
#5149=LINE('',#30399,#7030);
#5150=LINE('',#30402,#7031);
#5151=LINE('',#30404,#7032);
#5152=LINE('',#30405,#7033);
#5153=LINE('',#30408,#7034);
#5154=LINE('',#30410,#7035);
#5155=LINE('',#30411,#7036);
#5156=LINE('',#30413,#7037);
#5157=LINE('',#30414,#7038);
#5158=LINE('',#30418,#7039);
#5159=LINE('',#30420,#7040);
#5160=LINE('',#30422,#7041);
#5161=LINE('',#30423,#7042);
#5162=LINE('',#30426,#7043);
#5163=LINE('',#30428,#7044);
#5164=LINE('',#30429,#7045);
#5165=LINE('',#30432,#7046);
#5166=LINE('',#30434,#7047);
#5167=LINE('',#30435,#7048);
#5168=LINE('',#30437,#7049);
#5169=LINE('',#30438,#7050);
#5170=LINE('',#30442,#7051);
#5171=LINE('',#30444,#7052);
#5172=LINE('',#30446,#7053);
#5173=LINE('',#30447,#7054);
#5174=LINE('',#30450,#7055);
#5175=LINE('',#30452,#7056);
#5176=LINE('',#30453,#7057);
#5177=LINE('',#30456,#7058);
#5178=LINE('',#30458,#7059);
#5179=LINE('',#30459,#7060);
#5180=LINE('',#30462,#7061);
#5181=LINE('',#30464,#7062);
#5182=LINE('',#30465,#7063);
#5183=LINE('',#30468,#7064);
#5184=LINE('',#30470,#7065);
#5185=LINE('',#30471,#7066);
#5186=LINE('',#30474,#7067);
#5187=LINE('',#30476,#7068);
#5188=LINE('',#30477,#7069);
#5189=LINE('',#30480,#7070);
#5190=LINE('',#30482,#7071);
#5191=LINE('',#30483,#7072);
#5192=LINE('',#30486,#7073);
#5193=LINE('',#30488,#7074);
#5194=LINE('',#30489,#7075);
#5195=LINE('',#30492,#7076);
#5196=LINE('',#30494,#7077);
#5197=LINE('',#30495,#7078);
#5198=LINE('',#30498,#7079);
#5199=LINE('',#30500,#7080);
#5200=LINE('',#30501,#7081);
#5201=LINE('',#30503,#7082);
#5202=LINE('',#30504,#7083);
#5203=LINE('',#30509,#7084);
#5204=LINE('',#30513,#7085);
#5205=LINE('',#30515,#7086);
#5206=LINE('',#30516,#7087);
#5207=LINE('',#30519,#7088);
#5208=LINE('',#30521,#7089);
#5209=LINE('',#30522,#7090);
#5210=LINE('',#30525,#7091);
#5211=LINE('',#30527,#7092);
#5212=LINE('',#30528,#7093);
#5213=LINE('',#30531,#7094);
#5214=LINE('',#30533,#7095);
#5215=LINE('',#30534,#7096);
#5216=LINE('',#30537,#7097);
#5217=LINE('',#30539,#7098);
#5218=LINE('',#30540,#7099);
#5219=LINE('',#30543,#7100);
#5220=LINE('',#30545,#7101);
#5221=LINE('',#30546,#7102);
#5222=LINE('',#30549,#7103);
#5223=LINE('',#30551,#7104);
#5224=LINE('',#30552,#7105);
#5225=LINE('',#30554,#7106);
#5226=LINE('',#30555,#7107);
#5227=LINE('',#30559,#7108);
#5228=LINE('',#30561,#7109);
#5229=LINE('',#30563,#7110);
#5230=LINE('',#30564,#7111);
#5231=LINE('',#30570,#7112);
#5232=LINE('',#30573,#7113);
#5233=LINE('',#30575,#7114);
#5234=LINE('',#30576,#7115);
#5235=LINE('',#30582,#7116);
#5236=LINE('',#30586,#7117);
#5237=LINE('',#30588,#7118);
#5238=LINE('',#30590,#7119);
#5239=LINE('',#30591,#7120);
#5240=LINE('',#30594,#7121);
#5241=LINE('',#30596,#7122);
#5242=LINE('',#30597,#7123);
#5243=LINE('',#30600,#7124);
#5244=LINE('',#30602,#7125);
#5245=LINE('',#30603,#7126);
#5246=LINE('',#30606,#7127);
#5247=LINE('',#30608,#7128);
#5248=LINE('',#30609,#7129);
#5249=LINE('',#30612,#7130);
#5250=LINE('',#30614,#7131);
#5251=LINE('',#30615,#7132);
#5252=LINE('',#30618,#7133);
#5253=LINE('',#30620,#7134);
#5254=LINE('',#30621,#7135);
#5255=LINE('',#30623,#7136);
#5256=LINE('',#30624,#7137);
#5257=LINE('',#30627,#7138);
#5258=LINE('',#30629,#7139);
#5259=LINE('',#30630,#7140);
#5260=LINE('',#30633,#7141);
#5261=LINE('',#30635,#7142);
#5262=LINE('',#30636,#7143);
#5263=LINE('',#30639,#7144);
#5264=LINE('',#30641,#7145);
#5265=LINE('',#30642,#7146);
#5266=LINE('',#30645,#7147);
#5267=LINE('',#30647,#7148);
#5268=LINE('',#30648,#7149);
#5269=LINE('',#30653,#7150);
#5270=LINE('',#30657,#7151);
#5271=LINE('',#30659,#7152);
#5272=LINE('',#30660,#7153);
#5273=LINE('',#30665,#7154);
#5274=LINE('',#30668,#7155);
#5275=LINE('',#30669,#7156);
#5276=LINE('',#30672,#7157);
#5277=LINE('',#30674,#7158);
#5278=LINE('',#30675,#7159);
#5279=LINE('',#30678,#7160);
#5280=LINE('',#30680,#7161);
#5281=LINE('',#30681,#7162);
#5282=LINE('',#30684,#7163);
#5283=LINE('',#30686,#7164);
#5284=LINE('',#30687,#7165);
#5285=LINE('',#30690,#7166);
#5286=LINE('',#30692,#7167);
#5287=LINE('',#30693,#7168);
#5288=LINE('',#30696,#7169);
#5289=LINE('',#30698,#7170);
#5290=LINE('',#30699,#7171);
#5291=LINE('',#30702,#7172);
#5292=LINE('',#30704,#7173);
#5293=LINE('',#30705,#7174);
#5294=LINE('',#30708,#7175);
#5295=LINE('',#30710,#7176);
#5296=LINE('',#30711,#7177);
#5297=LINE('',#30714,#7178);
#5298=LINE('',#30716,#7179);
#5299=LINE('',#30717,#7180);
#5300=LINE('',#30722,#7181);
#5301=LINE('',#30726,#7182);
#5302=LINE('',#30728,#7183);
#5303=LINE('',#30729,#7184);
#5304=LINE('',#30732,#7185);
#5305=LINE('',#30734,#7186);
#5306=LINE('',#30735,#7187);
#5307=LINE('',#30738,#7188);
#5308=LINE('',#30740,#7189);
#5309=LINE('',#30741,#7190);
#5310=LINE('',#30744,#7191);
#5311=LINE('',#30746,#7192);
#5312=LINE('',#30747,#7193);
#5313=LINE('',#30750,#7194);
#5314=LINE('',#30752,#7195);
#5315=LINE('',#30753,#7196);
#5316=LINE('',#30756,#7197);
#5317=LINE('',#30758,#7198);
#5318=LINE('',#30759,#7199);
#5319=LINE('',#30762,#7200);
#5320=LINE('',#30764,#7201);
#5321=LINE('',#30765,#7202);
#5322=LINE('',#30768,#7203);
#5323=LINE('',#30770,#7204);
#5324=LINE('',#30772,#7205);
#5325=LINE('',#30774,#7206);
#5326=LINE('',#30776,#7207);
#5327=LINE('',#30778,#7208);
#5328=LINE('',#30780,#7209);
#5329=LINE('',#30782,#7210);
#5330=LINE('',#30784,#7211);
#5331=LINE('',#30786,#7212);
#5332=LINE('',#30788,#7213);
#5333=LINE('',#30790,#7214);
#5334=LINE('',#30792,#7215);
#5335=LINE('',#30794,#7216);
#5336=LINE('',#30796,#7217);
#5337=LINE('',#30800,#7218);
#5338=LINE('',#30802,#7219);
#5339=LINE('',#30804,#7220);
#5340=LINE('',#30806,#7221);
#5341=LINE('',#30808,#7222);
#5342=LINE('',#30810,#7223);
#5343=LINE('',#30812,#7224);
#5344=LINE('',#30813,#7225);
#5345=LINE('',#30815,#7226);
#5346=LINE('',#30817,#7227);
#5347=LINE('',#30819,#7228);
#5348=LINE('',#30821,#7229);
#5349=LINE('',#30822,#7230);
#5350=LINE('',#30827,#7231);
#5351=LINE('',#30831,#7232);
#5352=LINE('',#30835,#7233);
#5353=LINE('',#30838,#7234);
#5354=LINE('',#30843,#7235);
#5355=LINE('',#30845,#7236);
#5356=LINE('',#30846,#7237);
#5357=LINE('',#30849,#7238);
#5358=LINE('',#30853,#7239);
#5359=LINE('',#30854,#7240);
#5360=LINE('',#30857,#7241);
#5361=LINE('',#30861,#7242);
#5362=LINE('',#30863,#7243);
#5363=LINE('',#30864,#7244);
#5364=LINE('',#30867,#7245);
#5365=LINE('',#30868,#7246);
#5366=LINE('',#30871,#7247);
#5367=LINE('',#30872,#7248);
#5368=LINE('',#30875,#7249);
#5369=LINE('',#30876,#7250);
#5370=LINE('',#30879,#7251);
#5371=LINE('',#30880,#7252);
#5372=LINE('',#30883,#7253);
#5373=LINE('',#30884,#7254);
#5374=LINE('',#30886,#7255);
#5375=LINE('',#30889,#7256);
#5376=LINE('',#30890,#7257);
#5377=LINE('',#30893,#7258);
#5378=LINE('',#30894,#7259);
#5379=LINE('',#30897,#7260);
#5380=LINE('',#30898,#7261);
#5381=LINE('',#30901,#7262);
#5382=LINE('',#30902,#7263);
#5383=LINE('',#30904,#7264);
#5384=LINE('',#30908,#7265);
#5385=LINE('',#30911,#7266);
#5386=LINE('',#30912,#7267);
#5387=LINE('',#30916,#7268);
#5388=LINE('',#30919,#7269);
#5389=LINE('',#30920,#7270);
#5390=LINE('',#30924,#7271);
#5391=LINE('',#30926,#7272);
#5392=LINE('',#30929,#7273);
#5393=LINE('',#30930,#7274);
#5394=LINE('',#30933,#7275);
#5395=LINE('',#30934,#7276);
#5396=LINE('',#30937,#7277);
#5397=LINE('',#30938,#7278);
#5398=LINE('',#30941,#7279);
#5399=LINE('',#30942,#7280);
#5400=LINE('',#30945,#7281);
#5401=LINE('',#30946,#7282);
#5402=LINE('',#30949,#7283);
#5403=LINE('',#30950,#7284);
#5404=LINE('',#30953,#7285);
#5405=LINE('',#30954,#7286);
#5406=LINE('',#30957,#7287);
#5407=LINE('',#30958,#7288);
#5408=LINE('',#30962,#7289);
#5409=LINE('',#30965,#7290);
#5410=LINE('',#30966,#7291);
#5411=LINE('',#30969,#7292);
#5412=LINE('',#30970,#7293);
#5413=LINE('',#30973,#7294);
#5414=LINE('',#30974,#7295);
#5415=LINE('',#30977,#7296);
#5416=LINE('',#30978,#7297);
#5417=LINE('',#30981,#7298);
#5418=LINE('',#30982,#7299);
#5419=LINE('',#30985,#7300);
#5420=LINE('',#30986,#7301);
#5421=LINE('',#30988,#7302);
#5422=LINE('',#30994,#7303);
#5423=LINE('',#31018,#7304);
#5424=LINE('',#31072,#7305);
#5425=LINE('',#31129,#7306);
#5426=LINE('',#31183,#7307);
#5427=LINE('',#31237,#7308);
#5428=LINE('',#31291,#7309);
#5429=LINE('',#31342,#7310);
#5430=LINE('',#31396,#7311);
#5431=LINE('',#31450,#7312);
#5432=LINE('',#31504,#7313);
#5433=LINE('',#31558,#7314);
#5434=LINE('',#31612,#7315);
#5435=LINE('',#31666,#7316);
#5436=LINE('',#31720,#7317);
#5437=LINE('',#31774,#7318);
#5438=LINE('',#31828,#7319);
#5439=LINE('',#31882,#7320);
#5440=LINE('',#31939,#7321);
#5441=LINE('',#31993,#7322);
#5442=LINE('',#32047,#7323);
#5443=LINE('',#32101,#7324);
#5444=LINE('',#32152,#7325);
#5445=LINE('',#32206,#7326);
#5446=LINE('',#32260,#7327);
#5447=LINE('',#32314,#7328);
#5448=LINE('',#32368,#7329);
#5449=LINE('',#32422,#7330);
#5450=LINE('',#32479,#7331);
#5451=LINE('',#32533,#7332);
#5452=LINE('',#32587,#7333);
#5453=LINE('',#32644,#7334);
#5454=LINE('',#32698,#7335);
#5455=LINE('',#32752,#7336);
#5456=LINE('',#32806,#7337);
#5457=LINE('',#32860,#7338);
#5458=LINE('',#32914,#7339);
#5459=LINE('',#32965,#7340);
#5460=LINE('',#33019,#7341);
#5461=LINE('',#33073,#7342);
#5462=LINE('',#33127,#7343);
#5463=LINE('',#33184,#7344);
#5464=LINE('',#33238,#7345);
#5465=LINE('',#33292,#7346);
#5466=LINE('',#33346,#7347);
#5467=LINE('',#33400,#7348);
#5468=LINE('',#33454,#7349);
#5469=LINE('',#33508,#7350);
#5470=LINE('',#33562,#7351);
#5471=LINE('',#33616,#7352);
#5472=LINE('',#33670,#7353);
#5473=LINE('',#33724,#7354);
#5474=LINE('',#33775,#7355);
#5475=LINE('',#33829,#7356);
#5476=LINE('',#33883,#7357);
#5477=LINE('',#33937,#7358);
#5478=LINE('',#33991,#7359);
#5479=LINE('',#34045,#7360);
#5480=LINE('',#34099,#7361);
#5481=LINE('',#34150,#7362);
#5482=LINE('',#34204,#7363);
#5483=LINE('',#34258,#7364);
#5484=LINE('',#34312,#7365);
#5485=LINE('',#34363,#7366);
#5486=LINE('',#34417,#7367);
#5487=LINE('',#34471,#7368);
#5488=LINE('',#34525,#7369);
#5489=LINE('',#34579,#7370);
#5490=LINE('',#34633,#7371);
#5491=LINE('',#34690,#7372);
#5492=LINE('',#34744,#7373);
#5493=LINE('',#34798,#7374);
#5494=LINE('',#34852,#7375);
#5495=LINE('',#34906,#7376);
#5496=LINE('',#34963,#7377);
#5497=LINE('',#35017,#7378);
#5498=LINE('',#35074,#7379);
#5499=LINE('',#35128,#7380);
#5500=LINE('',#35179,#7381);
#5501=LINE('',#35233,#7382);
#5502=LINE('',#35287,#7383);
#5503=LINE('',#35341,#7384);
#5504=LINE('',#35395,#7385);
#5505=LINE('',#35449,#7386);
#5506=LINE('',#35506,#7387);
#5507=LINE('',#35560,#7388);
#5508=LINE('',#35614,#7389);
#5509=LINE('',#35668,#7390);
#5510=LINE('',#35722,#7391);
#5511=LINE('',#35776,#7392);
#5512=LINE('',#35830,#7393);
#5513=LINE('',#35884,#7394);
#5514=LINE('',#35938,#7395);
#5515=LINE('',#35989,#7396);
#5516=LINE('',#36043,#7397);
#5517=LINE('',#36097,#7398);
#5518=LINE('',#36151,#7399);
#5519=LINE('',#36205,#7400);
#5520=LINE('',#36262,#7401);
#5521=LINE('',#36316,#7402);
#5522=LINE('',#36370,#7403);
#5523=LINE('',#36423,#7404);
#5524=LINE('',#36443,#7405);
#5525=LINE('',#36469,#7406);
#5526=LINE('',#36532,#7407);
#5527=LINE('',#36593,#7408);
#5528=LINE('',#36657,#7409);
#5529=LINE('',#36721,#7410);
#5530=LINE('',#36784,#7411);
#5531=LINE('',#36845,#7412);
#5532=LINE('',#36909,#7413);
#5533=LINE('',#36972,#7414);
#5534=LINE('',#37033,#7415);
#5535=LINE('',#37061,#7416);
#5536=LINE('',#37098,#7417);
#5537=LINE('',#37136,#7418);
#5538=LINE('',#37174,#7419);
#5539=LINE('',#37210,#7420);
#5540=LINE('',#37248,#7421);
#5541=LINE('',#37286,#7422);
#5542=LINE('',#37324,#7423);
#5543=LINE('',#37360,#7424);
#5544=LINE('',#37398,#7425);
#5545=LINE('',#37421,#7426);
#5546=LINE('',#37447,#7427);
#5547=LINE('',#37484,#7428);
#5548=LINE('',#37527,#7429);
#5549=LINE('',#37581,#7430);
#5550=LINE('',#37632,#7431);
#5551=LINE('',#37658,#7432);
#5552=LINE('',#37686,#7433);
#5553=LINE('',#37723,#7434);
#5554=LINE('',#37777,#7435);
#5555=LINE('',#37817,#7436);
#5556=LINE('',#37845,#7437);
#5557=LINE('',#37882,#7438);
#5558=LINE('',#37922,#7439);
#5559=LINE('',#37979,#7440);
#5560=LINE('',#38033,#7441);
#5561=LINE('',#38073,#7442);
#5562=LINE('',#38099,#7443);
#5563=LINE('',#38126,#7444);
#5564=LINE('',#38166,#7445);
#5565=LINE('',#38220,#7446);
#5566=LINE('',#38264,#7447);
#5567=LINE('',#38290,#7448);
#5568=LINE('',#38316,#7449);
#5569=LINE('',#38341,#7450);
#5570=LINE('',#38369,#7451);
#5571=LINE('',#38395,#7452);
#5572=LINE('',#38421,#7453);
#5573=LINE('',#38448,#7454);
#5574=LINE('',#38474,#7455);
#5575=LINE('',#38511,#7456);
#5576=LINE('',#38551,#7457);
#5577=LINE('',#38595,#7458);
#5578=LINE('',#38620,#7459);
#5579=LINE('',#38646,#7460);
#5580=LINE('',#38674,#7461);
#5581=LINE('',#38700,#7462);
#5582=LINE('',#38737,#7463);
#5583=LINE('',#38762,#7464);
#5584=LINE('',#38790,#7465);
#5585=LINE('',#38816,#7466);
#5586=LINE('',#38842,#7467);
#5587=LINE('',#38870,#7468);
#5588=LINE('',#38895,#7469);
#5589=LINE('',#38932,#7470);
#5590=LINE('',#38958,#7471);
#5591=LINE('',#38986,#7472);
#5592=LINE('',#39012,#7473);
#5593=LINE('',#39037,#7474);
#5594=LINE('',#39065,#7475);
#5595=LINE('',#39090,#7476);
#5596=LINE('',#39127,#7477);
#5597=LINE('',#39153,#7478);
#5598=LINE('',#39181,#7479);
#5599=LINE('',#39207,#7480);
#5600=LINE('',#39232,#7481);
#5601=LINE('',#39260,#7482);
#5602=LINE('',#39286,#7483);
#5603=LINE('',#39323,#7484);
#5604=LINE('',#39349,#7485);
#5605=LINE('',#39376,#7486);
#5606=LINE('',#39402,#7487);
#5607=LINE('',#39428,#7488);
#5608=LINE('',#39456,#7489);
#5609=LINE('',#39481,#7490);
#5610=LINE('',#39507,#7491);
#5611=LINE('',#39533,#7492);
#5612=LINE('',#39561,#7493);
#5613=LINE('',#39587,#7494);
#5614=LINE('',#39613,#7495);
#5615=LINE('',#39640,#7496);
#5616=LINE('',#39666,#7497);
#5617=LINE('',#39692,#7498);
#5618=LINE('',#39718,#7499);
#5619=LINE('',#39745,#7500);
#5620=LINE('',#39771,#7501);
#5621=LINE('',#39808,#7502);
#5622=LINE('',#39836,#7503);
#5623=LINE('',#39862,#7504);
#5624=LINE('',#39888,#7505);
#5625=LINE('',#39913,#7506);
#5626=LINE('',#39941,#7507);
#5627=LINE('',#39967,#7508);
#5628=LINE('',#40004,#7509);
#5629=LINE('',#40031,#7510);
#5630=LINE('',#40057,#7511);
#5631=LINE('',#40094,#7512);
#5632=LINE('',#40120,#7513);
#5633=LINE('',#40148,#7514);
#5634=LINE('',#40173,#7515);
#5635=LINE('',#40199,#7516);
#5636=LINE('',#40227,#7517);
#5637=LINE('',#40253,#7518);
#5638=LINE('',#40290,#7519);
#5639=LINE('',#40315,#7520);
#5640=LINE('',#40343,#7521);
#5641=LINE('',#40369,#7522);
#5642=LINE('',#40395,#7523);
#5643=LINE('',#40422,#7524);
#5644=LINE('',#40449,#7525);
#5645=LINE('',#40453,#7526);
#5646=LINE('',#40460,#7527);
#5647=LINE('',#40464,#7528);
#5648=LINE('',#47633,#7529);
#5649=LINE('',#47637,#7530);
#5650=LINE('',#47639,#7531);
#5651=LINE('',#47640,#7532);
#5652=LINE('',#47647,#7533);
#5653=LINE('',#47653,#7534);
#5654=LINE('',#47659,#7535);
#5655=LINE('',#47665,#7536);
#5656=LINE('',#47671,#7537);
#5657=LINE('',#47677,#7538);
#5658=LINE('',#47683,#7539);
#5659=LINE('',#47689,#7540);
#5660=LINE('',#47695,#7541);
#5661=LINE('',#47701,#7542);
#5662=LINE('',#47707,#7543);
#5663=LINE('',#47713,#7544);
#5664=LINE('',#47719,#7545);
#5665=LINE('',#47725,#7546);
#5666=LINE('',#47731,#7547);
#5667=LINE('',#47737,#7548);
#5668=LINE('',#47742,#7549);
#5669=LINE('',#47747,#7550);
#5670=LINE('',#47748,#7551);
#5671=LINE('',#47751,#7552);
#5672=LINE('',#47752,#7553);
#5673=LINE('',#47756,#7554);
#5674=LINE('',#47759,#7555);
#5675=LINE('',#47760,#7556);
#5676=LINE('',#47763,#7557);
#5677=LINE('',#47764,#7558);
#5678=LINE('',#47766,#7559);
#5679=LINE('',#47770,#7560);
#5680=LINE('',#47772,#7561);
#5681=LINE('',#47774,#7562);
#5682=LINE('',#47775,#7563);
#5683=LINE('',#47778,#7564);
#5684=LINE('',#47780,#7565);
#5685=LINE('',#47781,#7566);
#5686=LINE('',#47784,#7567);
#5687=LINE('',#47786,#7568);
#5688=LINE('',#47787,#7569);
#5689=LINE('',#47790,#7570);
#5690=LINE('',#47792,#7571);
#5691=LINE('',#47793,#7572);
#5692=LINE('',#47796,#7573);
#5693=LINE('',#47798,#7574);
#5694=LINE('',#47799,#7575);
#5695=LINE('',#47802,#7576);
#5696=LINE('',#47804,#7577);
#5697=LINE('',#47805,#7578);
#5698=LINE('',#47808,#7579);
#5699=LINE('',#47810,#7580);
#5700=LINE('',#47811,#7581);
#5701=LINE('',#47813,#7582);
#5702=LINE('',#47815,#7583);
#5703=LINE('',#47821,#7584);
#5704=LINE('',#47823,#7585);
#5705=LINE('',#47825,#7586);
#5706=LINE('',#47826,#7587);
#5707=LINE('',#47831,#7588);
#5708=LINE('',#47837,#7589);
#5709=LINE('',#47843,#7590);
#5710=LINE('',#47847,#7591);
#5711=LINE('',#47849,#7592);
#5712=LINE('',#47850,#7593);
#5713=LINE('',#47855,#7594);
#5714=LINE('',#47861,#7595);
#5715=LINE('',#47867,#7596);
#5716=LINE('',#47871,#7597);
#5717=LINE('',#47873,#7598);
#5718=LINE('',#47874,#7599);
#5719=LINE('',#47879,#7600);
#5720=LINE('',#47883,#7601);
#5721=LINE('',#47885,#7602);
#5722=LINE('',#47886,#7603);
#5723=LINE('',#47891,#7604);
#5724=LINE('',#47895,#7605);
#5725=LINE('',#47897,#7606);
#5726=LINE('',#47898,#7607);
#5727=LINE('',#47903,#7608);
#5728=LINE('',#47907,#7609);
#5729=LINE('',#47909,#7610);
#5730=LINE('',#47910,#7611);
#5731=LINE('',#47913,#7612);
#5732=LINE('',#47915,#7613);
#5733=LINE('',#47916,#7614);
#5734=LINE('',#47919,#7615);
#5735=LINE('',#47921,#7616);
#5736=LINE('',#47923,#7617);
#5737=LINE('',#47925,#7618);
#5738=LINE('',#47929,#7619);
#5739=LINE('',#47933,#7620);
#5740=LINE('',#47937,#7621);
#5741=LINE('',#47945,#7622);
#5742=LINE('',#47952,#7623);
#5743=LINE('',#47955,#7624);
#5744=LINE('',#47957,#7625);
#5745=LINE('',#47958,#7626);
#5746=LINE('',#47961,#7627);
#5747=LINE('',#47965,#7628);
#5748=LINE('',#47969,#7629);
#5749=LINE('',#47973,#7630);
#5750=LINE('',#47974,#7631);
#5751=LINE('',#47977,#7632);
#5752=LINE('',#47981,#7633);
#5753=LINE('',#47985,#7634);
#5754=LINE('',#47989,#7635);
#5755=LINE('',#47990,#7636);
#5756=LINE('',#47993,#7637);
#5757=LINE('',#47997,#7638);
#5758=LINE('',#47998,#7639);
#5759=LINE('',#48001,#7640);
#5760=LINE('',#48005,#7641);
#5761=LINE('',#48006,#7642);
#5762=LINE('',#48009,#7643);
#5763=LINE('',#48013,#7644);
#5764=LINE('',#48014,#7645);
#5765=LINE('',#48017,#7646);
#5766=LINE('',#48018,#7647);
#5767=LINE('',#48020,#7648);
#5768=LINE('',#48022,#7649);
#5769=LINE('',#48029,#7650);
#5770=LINE('',#48034,#7651);
#5771=LINE('',#48036,#7652);
#5772=LINE('',#48038,#7653);
#5773=LINE('',#48039,#7654);
#5774=LINE('',#48042,#7655);
#5775=LINE('',#48044,#7656);
#5776=LINE('',#48045,#7657);
#5777=LINE('',#48048,#7658);
#5778=LINE('',#48050,#7659);
#5779=LINE('',#48051,#7660);
#5780=LINE('',#48053,#7661);
#5781=LINE('',#48054,#7662);
#5782=LINE('',#48062,#7663);
#5783=LINE('',#48067,#7664);
#5784=LINE('',#48069,#7665);
#5785=LINE('',#48071,#7666);
#5786=LINE('',#48072,#7667);
#5787=LINE('',#48075,#7668);
#5788=LINE('',#48077,#7669);
#5789=LINE('',#48078,#7670);
#5790=LINE('',#48081,#7671);
#5791=LINE('',#48083,#7672);
#5792=LINE('',#48084,#7673);
#5793=LINE('',#48086,#7674);
#5794=LINE('',#48087,#7675);
#5795=LINE('',#48095,#7676);
#5796=LINE('',#48100,#7677);
#5797=LINE('',#48102,#7678);
#5798=LINE('',#48104,#7679);
#5799=LINE('',#48105,#7680);
#5800=LINE('',#48108,#7681);
#5801=LINE('',#48110,#7682);
#5802=LINE('',#48111,#7683);
#5803=LINE('',#48114,#7684);
#5804=LINE('',#48116,#7685);
#5805=LINE('',#48117,#7686);
#5806=LINE('',#48119,#7687);
#5807=LINE('',#48120,#7688);
#5808=LINE('',#48127,#7689);
#5809=LINE('',#48129,#7690);
#5810=LINE('',#48131,#7691);
#5811=LINE('',#48132,#7692);
#5812=LINE('',#48137,#7693);
#5813=LINE('',#48143,#7694);
#5814=LINE('',#48149,#7695);
#5815=LINE('',#48153,#7696);
#5816=LINE('',#48155,#7697);
#5817=LINE('',#48156,#7698);
#5818=LINE('',#48161,#7699);
#5819=LINE('',#48167,#7700);
#5820=LINE('',#48173,#7701);
#5821=LINE('',#48177,#7702);
#5822=LINE('',#48179,#7703);
#5823=LINE('',#48180,#7704);
#5824=LINE('',#48185,#7705);
#5825=LINE('',#48189,#7706);
#5826=LINE('',#48191,#7707);
#5827=LINE('',#48192,#7708);
#5828=LINE('',#48197,#7709);
#5829=LINE('',#48201,#7710);
#5830=LINE('',#48203,#7711);
#5831=LINE('',#48204,#7712);
#5832=LINE('',#48209,#7713);
#5833=LINE('',#48213,#7714);
#5834=LINE('',#48215,#7715);
#5835=LINE('',#48216,#7716);
#5836=LINE('',#48219,#7717);
#5837=LINE('',#48221,#7718);
#5838=LINE('',#48222,#7719);
#5839=LINE('',#48225,#7720);
#5840=LINE('',#48227,#7721);
#5841=LINE('',#48235,#7722);
#5842=LINE('',#48243,#7723);
#5843=LINE('',#48247,#7724);
#5844=LINE('',#48251,#7725);
#5845=LINE('',#48255,#7726);
#5846=LINE('',#48257,#7727);
#5847=LINE('',#48258,#7728);
#5848=LINE('',#48261,#7729);
#5849=LINE('',#48263,#7730);
#5850=LINE('',#48264,#7731);
#5851=LINE('',#48268,#7732);
#5852=LINE('',#48272,#7733);
#5853=LINE('',#48276,#7734);
#5854=LINE('',#48279,#7735);
#5855=LINE('',#48280,#7736);
#5856=LINE('',#48284,#7737);
#5857=LINE('',#48288,#7738);
#5858=LINE('',#48292,#7739);
#5859=LINE('',#48295,#7740);
#5860=LINE('',#48296,#7741);
#5861=LINE('',#48300,#7742);
#5862=LINE('',#48303,#7743);
#5863=LINE('',#48304,#7744);
#5864=LINE('',#48308,#7745);
#5865=LINE('',#48311,#7746);
#5866=LINE('',#48312,#7747);
#5867=LINE('',#48316,#7748);
#5868=LINE('',#48319,#7749);
#5869=LINE('',#48320,#7750);
#5870=LINE('',#48323,#7751);
#5871=LINE('',#48324,#7752);
#5872=LINE('',#48326,#7753);
#5873=LINE('',#48328,#7754);
#5874=VECTOR('',#21932,10.);
#5875=VECTOR('',#21933,10.);
#5876=VECTOR('',#21934,10.);
#5877=VECTOR('',#21935,10.);
#5878=VECTOR('',#21938,10.);
#5879=VECTOR('',#21941,10.);
#5880=VECTOR('',#21948,10.);
#5881=VECTOR('',#21955,10.);
#5882=VECTOR('',#21956,10.);
#5883=VECTOR('',#21957,10.);
#5884=VECTOR('',#21964,10.);
#5885=VECTOR('',#21971,10.);
#5886=VECTOR('',#21974,10.);
#5887=VECTOR('',#21977,10.);
#5888=VECTOR('',#21978,10.);
#5889=VECTOR('',#21979,10.);
#5890=VECTOR('',#21980,10.);
#5891=VECTOR('',#21981,10.);
#5892=VECTOR('',#21982,10.);
#5893=VECTOR('',#21983,10.);
#5894=VECTOR('',#21986,10.);
#5895=VECTOR('',#21987,10.);
#5896=VECTOR('',#21988,10.);
#5897=VECTOR('',#21993,10.);
#5898=VECTOR('',#21998,10.);
#5899=VECTOR('',#22003,10.);
#5900=VECTOR('',#22006,10.);
#5901=VECTOR('',#22007,10.);
#5902=VECTOR('',#22012,10.);
#5903=VECTOR('',#22017,10.);
#5904=VECTOR('',#22022,10.);
#5905=VECTOR('',#22025,10.);
#5906=VECTOR('',#22026,10.);
#5907=VECTOR('',#22031,10.);
#5908=VECTOR('',#22034,10.);
#5909=VECTOR('',#22035,10.);
#5910=VECTOR('',#22040,10.);
#5911=VECTOR('',#22043,10.);
#5912=VECTOR('',#22044,10.);
#5913=VECTOR('',#22047,10.);
#5914=VECTOR('',#22048,10.);
#5915=VECTOR('',#22051,10.);
#5916=VECTOR('',#22052,10.);
#5917=VECTOR('',#22055,10.);
#5918=VECTOR('',#22056,10.);
#5919=VECTOR('',#22059,10.);
#5920=VECTOR('',#22060,10.);
#5921=VECTOR('',#22061,10.);
#5922=VECTOR('',#22064,10.);
#5923=VECTOR('',#22065,10.);
#5924=VECTOR('',#22068,10.);
#5925=VECTOR('',#22069,10.);
#5926=VECTOR('',#22072,10.);
#5927=VECTOR('',#22073,10.);
#5928=VECTOR('',#22078,10.);
#5929=VECTOR('',#22081,10.);
#5930=VECTOR('',#22082,10.);
#5931=VECTOR('',#22085,10.);
#5932=VECTOR('',#22086,10.);
#5933=VECTOR('',#22089,10.);
#5934=VECTOR('',#22092,10.);
#5935=VECTOR('',#22093,10.);
#5936=VECTOR('',#22096,10.);
#5937=VECTOR('',#22097,10.);
#5938=VECTOR('',#22100,10.);
#5939=VECTOR('',#22101,10.);
#5940=VECTOR('',#22104,10.);
#5941=VECTOR('',#22109,10.);
#5942=VECTOR('',#22114,10.);
#5943=VECTOR('',#22119,10.);
#5944=VECTOR('',#22120,10.);
#5945=VECTOR('',#22123,10.);
#5946=VECTOR('',#22128,10.);
#5947=VECTOR('',#22133,10.);
#5948=VECTOR('',#22138,10.);
#5949=VECTOR('',#22139,10.);
#5950=VECTOR('',#22148,10.);
#5951=VECTOR('',#22149,10.);
#5952=VECTOR('',#22150,10.);
#5953=VECTOR('',#22151,10.);
#5954=VECTOR('',#22156,10.);
#5955=VECTOR('',#22163,10.);
#5956=VECTOR('',#22170,10.);
#5957=VECTOR('',#22175,10.);
#5958=VECTOR('',#22176,10.);
#5959=VECTOR('',#22177,10.);
#5960=VECTOR('',#22182,10.);
#5961=VECTOR('',#22189,10.);
#5962=VECTOR('',#22194,10.);
#5963=VECTOR('',#22195,10.);
#5964=VECTOR('',#22196,10.);
#5965=VECTOR('',#22197,10.);
#5966=VECTOR('',#22198,10.);
#5967=VECTOR('',#22201,10.);
#5968=VECTOR('',#22204,10.);
#5969=VECTOR('',#22207,10.);
#5970=VECTOR('',#22208,10.);
#5971=VECTOR('',#22215,10.);
#5972=VECTOR('',#22222,10.);
#5973=VECTOR('',#22225,10.);
#5974=VECTOR('',#22228,10.);
#5975=VECTOR('',#22229,10.);
#5976=VECTOR('',#22230,10.);
#5977=VECTOR('',#22231,10.);
#5978=VECTOR('',#22232,10.);
#5979=VECTOR('',#22233,10.);
#5980=VECTOR('',#22234,10.);
#5981=VECTOR('',#22235,10.);
#5982=VECTOR('',#22238,10.);
#5983=VECTOR('',#22241,10.);
#5984=VECTOR('',#22242,10.);
#5985=VECTOR('',#22243,10.);
#5986=VECTOR('',#22246,10.);
#5987=VECTOR('',#22247,10.);
#5988=VECTOR('',#22248,10.);
#5989=VECTOR('',#22251,10.);
#5990=VECTOR('',#22252,10.);
#5991=VECTOR('',#22255,10.);
#5992=VECTOR('',#22256,10.);
#5993=VECTOR('',#22259,10.);
#5994=VECTOR('',#22260,10.);
#5995=VECTOR('',#22267,10.);
#5996=VECTOR('',#22272,10.);
#5997=VECTOR('',#22273,10.);
#5998=VECTOR('',#22278,10.);
#5999=VECTOR('',#22279,10.);
#6000=VECTOR('',#22280,10.);
#6001=VECTOR('',#22281,10.);
#6002=VECTOR('',#22282,10.);
#6003=VECTOR('',#22283,10.);
#6004=VECTOR('',#22284,10.);
#6005=VECTOR('',#22285,10.);
#6006=VECTOR('',#22288,10.);
#6007=VECTOR('',#22291,10.);
#6008=VECTOR('',#22298,10.);
#6009=VECTOR('',#22305,10.);
#6010=VECTOR('',#22306,10.);
#6011=VECTOR('',#22309,10.);
#6012=VECTOR('',#22312,10.);
#6013=VECTOR('',#22315,10.);
#6014=VECTOR('',#22316,10.);
#6015=VECTOR('',#22317,10.);
#6016=VECTOR('',#22318,10.);
#6017=VECTOR('',#22321,10.);
#6018=VECTOR('',#22322,10.);
#6019=VECTOR('',#22325,10.);
#6020=VECTOR('',#22328,10.);
#6021=VECTOR('',#22331,10.);
#6022=VECTOR('',#22340,3.00000000000001);
#6023=VECTOR('',#22345,3.00000000000001);
#6024=VECTOR('',#22350,3.00000000000001);
#6025=VECTOR('',#22355,3.00000000000001);
#6026=VECTOR('',#22360,10.);
#6027=VECTOR('',#22363,10.);
#6028=VECTOR('',#22366,10.);
#6029=VECTOR('',#22369,10.);
#6030=VECTOR('',#22372,10.);
#6031=VECTOR('',#22375,10.);
#6032=VECTOR('',#22378,10.);
#6033=VECTOR('',#22381,10.);
#6034=VECTOR('',#22386,10.);
#6035=VECTOR('',#22389,10.);
#6036=VECTOR('',#22392,10.);
#6037=VECTOR('',#22395,10.);
#6038=VECTOR('',#22398,10.);
#6039=VECTOR('',#22401,10.);
#6040=VECTOR('',#22404,10.);
#6041=VECTOR('',#22407,10.);
#6042=VECTOR('',#22410,10.);
#6043=VECTOR('',#22413,10.);
#6044=VECTOR('',#22416,10.);
#6045=VECTOR('',#22419,10.);
#6046=VECTOR('',#22422,10.);
#6047=VECTOR('',#22425,10.);
#6048=VECTOR('',#22428,10.);
#6049=VECTOR('',#22431,10.);
#6050=VECTOR('',#22438,10.);
#6051=VECTOR('',#22441,10.);
#6052=VECTOR('',#22444,10.);
#6053=VECTOR('',#22445,10.);
#6054=VECTOR('',#22446,10.);
#6055=VECTOR('',#22451,10.);
#6056=VECTOR('',#22456,10.);
#6057=VECTOR('',#22457,10.);
#6058=VECTOR('',#22458,10.);
#6059=VECTOR('',#22463,10.);
#6060=VECTOR('',#22468,10.);
#6061=VECTOR('',#22469,10.);
#6062=VECTOR('',#22470,10.);
#6063=VECTOR('',#22473,10.);
#6064=VECTOR('',#22474,10.);
#6065=VECTOR('',#22475,10.);
#6066=VECTOR('',#22478,10.);
#6067=VECTOR('',#22479,10.);
#6068=VECTOR('',#22480,10.);
#6069=VECTOR('',#22483,10.);
#6070=VECTOR('',#22484,10.);
#6071=VECTOR('',#22485,10.);
#6072=VECTOR('',#22486,10.);
#6073=VECTOR('',#22489,10.);
#6074=VECTOR('',#22490,10.);
#6075=VECTOR('',#22491,10.);
#6076=VECTOR('',#22494,10.);
#6077=VECTOR('',#22495,10.);
#6078=VECTOR('',#22496,10.);
#6079=VECTOR('',#22499,10.);
#6080=VECTOR('',#22500,10.);
#6081=VECTOR('',#22501,10.);
#6082=VECTOR('',#22504,10.);
#6083=VECTOR('',#22505,10.);
#6084=VECTOR('',#22506,10.);
#6085=VECTOR('',#22509,10.);
#6086=VECTOR('',#22510,10.);
#6087=VECTOR('',#22511,10.);
#6088=VECTOR('',#22514,10.);
#6089=VECTOR('',#22515,10.);
#6090=VECTOR('',#22516,10.);
#6091=VECTOR('',#22521,10.);
#6092=VECTOR('',#22528,10.);
#6093=VECTOR('',#22535,10.);
#6094=VECTOR('',#22542,10.);
#6095=VECTOR('',#22543,10.);
#6096=VECTOR('',#22544,10.);
#6097=VECTOR('',#22551,10.);
#6098=VECTOR('',#22556,10.);
#6099=VECTOR('',#22557,10.);
#6100=VECTOR('',#22560,10.);
#6101=VECTOR('',#22563,10.);
#6102=VECTOR('',#22564,10.);
#6103=VECTOR('',#22569,10.);
#6104=VECTOR('',#22572,10.);
#6105=VECTOR('',#22573,10.);
#6106=VECTOR('',#22578,10.);
#6107=VECTOR('',#22583,10.);
#6108=VECTOR('',#22588,10.);
#6109=VECTOR('',#22591,10.);
#6110=VECTOR('',#22592,10.);
#6111=VECTOR('',#22597,10.);
#6112=VECTOR('',#22602,10.);
#6113=VECTOR('',#22607,10.);
#6114=VECTOR('',#22610,10.);
#6115=VECTOR('',#22611,10.);
#6116=VECTOR('',#22614,10.);
#6117=VECTOR('',#22615,10.);
#6118=VECTOR('',#22618,10.);
#6119=VECTOR('',#22619,10.);
#6120=VECTOR('',#22624,10.);
#6121=VECTOR('',#22629,10.);
#6122=VECTOR('',#22634,10.);
#6123=VECTOR('',#22637,10.);
#6124=VECTOR('',#22638,10.);
#6125=VECTOR('',#22643,10.);
#6126=VECTOR('',#22654,10.);
#6127=VECTOR('',#22655,10.);
#6128=VECTOR('',#22656,10.);
#6129=VECTOR('',#22657,10.);
#6130=VECTOR('',#22658,10.);
#6131=VECTOR('',#22659,10.);
#6132=VECTOR('',#22660,10.);
#6133=VECTOR('',#22661,10.);
#6134=VECTOR('',#22664,10.);
#6135=VECTOR('',#22667,10.);
#6136=VECTOR('',#22674,10.);
#6137=VECTOR('',#22681,10.);
#6138=VECTOR('',#22682,10.);
#6139=VECTOR('',#22683,10.);
#6140=VECTOR('',#22690,10.);
#6141=VECTOR('',#22697,10.);
#6142=VECTOR('',#22700,10.);
#6143=VECTOR('',#22703,10.);
#6144=VECTOR('',#22704,10.);
#6145=VECTOR('',#22705,10.);
#6146=VECTOR('',#22708,10.);
#6147=VECTOR('',#22709,10.);
#6148=VECTOR('',#22710,10.);
#6149=VECTOR('',#22713,10.);
#6150=VECTOR('',#22718,10.);
#6151=VECTOR('',#22723,10.);
#6152=VECTOR('',#22728,10.);
#6153=VECTOR('',#22729,10.);
#6154=VECTOR('',#22732,10.);
#6155=VECTOR('',#22737,10.);
#6156=VECTOR('',#22742,10.);
#6157=VECTOR('',#22747,10.);
#6158=VECTOR('',#22748,10.);
#6159=VECTOR('',#22751,10.);
#6160=VECTOR('',#22756,10.);
#6161=VECTOR('',#22757,10.);
#6162=VECTOR('',#22760,10.);
#6163=VECTOR('',#22765,10.);
#6164=VECTOR('',#22766,10.);
#6165=VECTOR('',#22769,10.);
#6166=VECTOR('',#22770,10.);
#6167=VECTOR('',#22773,10.);
#6168=VECTOR('',#22774,10.);
#6169=VECTOR('',#22777,10.);
#6170=VECTOR('',#22778,10.);
#6171=VECTOR('',#22781,10.);
#6172=VECTOR('',#22782,10.);
#6173=VECTOR('',#22783,10.);
#6174=VECTOR('',#22786,10.);
#6175=VECTOR('',#22787,10.);
#6176=VECTOR('',#22790,10.);
#6177=VECTOR('',#22791,10.);
#6178=VECTOR('',#22794,10.);
#6179=VECTOR('',#22795,10.);
#6180=VECTOR('',#22798,10.);
#6181=VECTOR('',#22803,10.);
#6182=VECTOR('',#22804,10.);
#6183=VECTOR('',#22807,10.);
#6184=VECTOR('',#22808,10.);
#6185=VECTOR('',#22811,10.);
#6186=VECTOR('',#22814,10.);
#6187=VECTOR('',#22815,10.);
#6188=VECTOR('',#22818,10.);
#6189=VECTOR('',#22819,10.);
#6190=VECTOR('',#22822,10.);
#6191=VECTOR('',#22823,10.);
#6192=VECTOR('',#22828,10.);
#6193=VECTOR('',#22833,10.);
#6194=VECTOR('',#22838,10.);
#6195=VECTOR('',#22841,10.);
#6196=VECTOR('',#22842,10.);
#6197=VECTOR('',#22847,10.);
#6198=VECTOR('',#22852,10.);
#6199=VECTOR('',#22857,10.);
#6200=VECTOR('',#22860,10.);
#6201=VECTOR('',#22861,10.);
#6202=VECTOR('',#22870,10.);
#6203=VECTOR('',#22871,10.);
#6204=VECTOR('',#22872,10.);
#6205=VECTOR('',#22873,10.);
#6206=VECTOR('',#22880,10.);
#6207=VECTOR('',#22887,10.);
#6208=VECTOR('',#22894,10.);
#6209=VECTOR('',#22897,10.);
#6210=VECTOR('',#22898,10.);
#6211=VECTOR('',#22899,10.);
#6212=VECTOR('',#22906,10.);
#6213=VECTOR('',#22913,10.);
#6214=VECTOR('',#22916,10.);
#6215=VECTOR('',#22917,10.);
#6216=VECTOR('',#22918,10.);
#6217=VECTOR('',#22919,10.);
#6218=VECTOR('',#22922,10.);
#6219=VECTOR('',#22925,10.);
#6220=VECTOR('',#22926,10.);
#6221=VECTOR('',#22927,10.);
#6222=VECTOR('',#22928,10.);
#6223=VECTOR('',#22929,10.);
#6224=VECTOR('',#22930,10.);
#6225=VECTOR('',#22931,10.);
#6226=VECTOR('',#22932,10.);
#6227=VECTOR('',#22935,10.);
#6228=VECTOR('',#22938,10.);
#6229=VECTOR('',#22945,10.);
#6230=VECTOR('',#22952,10.);
#6231=VECTOR('',#22953,10.);
#6232=VECTOR('',#22956,10.);
#6233=VECTOR('',#22959,10.);
#6234=VECTOR('',#22962,10.);
#6235=VECTOR('',#22963,10.);
#6236=VECTOR('',#22964,10.);
#6237=VECTOR('',#22965,10.);
#6238=VECTOR('',#22968,10.);
#6239=VECTOR('',#22969,10.);
#6240=VECTOR('',#22970,10.);
#6241=VECTOR('',#22973,10.);
#6242=VECTOR('',#22974,10.);
#6243=VECTOR('',#22977,10.);
#6244=VECTOR('',#22978,10.);
#6245=VECTOR('',#22981,10.);
#6246=VECTOR('',#22982,10.);
#6247=VECTOR('',#22989,10.);
#6248=VECTOR('',#22994,10.);
#6249=VECTOR('',#22995,10.);
#6250=VECTOR('',#22998,10.);
#6251=VECTOR('',#22999,10.);
#6252=VECTOR('',#23000,10.);
#6253=VECTOR('',#23001,10.);
#6254=VECTOR('',#23004,10.);
#6255=VECTOR('',#23007,10.);
#6256=VECTOR('',#23010,10.);
#6257=VECTOR('',#23011,10.);
#6258=VECTOR('',#23018,10.);
#6259=VECTOR('',#23025,10.);
#6260=VECTOR('',#23028,10.);
#6261=VECTOR('',#23031,10.);
#6262=VECTOR('',#23032,10.);
#6263=VECTOR('',#23033,10.);
#6264=VECTOR('',#23034,10.);
#6265=VECTOR('',#23035,10.);
#6266=VECTOR('',#23036,10.);
#6267=VECTOR('',#23037,10.);
#6268=VECTOR('',#23038,10.);
#6269=VECTOR('',#23043,10.);
#6270=VECTOR('',#23044,10.);
#6271=VECTOR('',#23047,10.);
#6272=VECTOR('',#23050,10.);
#6273=VECTOR('',#23053,10.);
#6274=VECTOR('',#23062,3.00000000000001);
#6275=VECTOR('',#23067,3.00000000000001);
#6276=VECTOR('',#23072,3.00000000000001);
#6277=VECTOR('',#23077,3.00000000000001);
#6278=VECTOR('',#23082,10.);
#6279=VECTOR('',#23085,10.);
#6280=VECTOR('',#23088,10.);
#6281=VECTOR('',#23091,10.);
#6282=VECTOR('',#23094,10.);
#6283=VECTOR('',#23097,10.);
#6284=VECTOR('',#23100,10.);
#6285=VECTOR('',#23103,10.);
#6286=VECTOR('',#23108,10.);
#6287=VECTOR('',#23111,10.);
#6288=VECTOR('',#23114,10.);
#6289=VECTOR('',#23117,10.);
#6290=VECTOR('',#23120,10.);
#6291=VECTOR('',#23123,10.);
#6292=VECTOR('',#23126,10.);
#6293=VECTOR('',#23129,10.);
#6294=VECTOR('',#23132,10.);
#6295=VECTOR('',#23135,10.);
#6296=VECTOR('',#23138,10.);
#6297=VECTOR('',#23141,10.);
#6298=VECTOR('',#23144,10.);
#6299=VECTOR('',#23147,10.);
#6300=VECTOR('',#23150,10.);
#6301=VECTOR('',#23153,10.);
#6302=VECTOR('',#23160,10.);
#6303=VECTOR('',#23163,10.);
#6304=VECTOR('',#23166,10.);
#6305=VECTOR('',#23167,10.);
#6306=VECTOR('',#23168,10.);
#6307=VECTOR('',#23175,10.);
#6308=VECTOR('',#23178,10.);
#6309=VECTOR('',#23179,10.);
#6310=VECTOR('',#23180,10.);
#6311=VECTOR('',#23187,10.);
#6312=VECTOR('',#23190,10.);
#6313=VECTOR('',#23191,10.);
#6314=VECTOR('',#23192,10.);
#6315=VECTOR('',#23195,10.);
#6316=VECTOR('',#23196,10.);
#6317=VECTOR('',#23197,10.);
#6318=VECTOR('',#23200,10.);
#6319=VECTOR('',#23201,10.);
#6320=VECTOR('',#23202,10.);
#6321=VECTOR('',#23205,10.);
#6322=VECTOR('',#23206,10.);
#6323=VECTOR('',#23207,10.);
#6324=VECTOR('',#23208,10.);
#6325=VECTOR('',#23211,10.);
#6326=VECTOR('',#23212,10.);
#6327=VECTOR('',#23213,10.);
#6328=VECTOR('',#23216,10.);
#6329=VECTOR('',#23217,10.);
#6330=VECTOR('',#23218,10.);
#6331=VECTOR('',#23221,10.);
#6332=VECTOR('',#23222,10.);
#6333=VECTOR('',#23223,10.);
#6334=VECTOR('',#23226,10.);
#6335=VECTOR('',#23227,10.);
#6336=VECTOR('',#23228,10.);
#6337=VECTOR('',#23231,10.);
#6338=VECTOR('',#23232,10.);
#6339=VECTOR('',#23233,10.);
#6340=VECTOR('',#23236,10.);
#6341=VECTOR('',#23237,10.);
#6342=VECTOR('',#23238,10.);
#6343=VECTOR('',#23245,10.);
#6344=VECTOR('',#23250,10.);
#6345=VECTOR('',#23251,10.);
#6346=VECTOR('',#23256,10.);
#6347=VECTOR('',#23263,10.);
#6348=VECTOR('',#23264,10.);
#6349=VECTOR('',#23265,10.);
#6350=VECTOR('',#23272,10.);
#6351=VECTOR('',#23279,10.);
#6352=VECTOR('',#23282,10.);
#6353=VECTOR('',#23285,10.);
#6354=VECTOR('',#23286,10.);
#6355=VECTOR('',#23291,10.);
#6356=VECTOR('',#23294,10.);
#6357=VECTOR('',#23295,10.);
#6358=VECTOR('',#23300,10.);
#6359=VECTOR('',#23305,10.);
#6360=VECTOR('',#23310,10.);
#6361=VECTOR('',#23313,10.);
#6362=VECTOR('',#23314,10.);
#6363=VECTOR('',#23319,10.);
#6364=VECTOR('',#23324,10.);
#6365=VECTOR('',#23329,10.);
#6366=VECTOR('',#23332,10.);
#6367=VECTOR('',#23333,10.);
#6368=VECTOR('',#23336,10.);
#6369=VECTOR('',#23337,10.);
#6370=VECTOR('',#23340,10.);
#6371=VECTOR('',#23341,10.);
#6372=VECTOR('',#23346,10.);
#6373=VECTOR('',#23351,10.);
#6374=VECTOR('',#23356,10.);
#6375=VECTOR('',#23359,10.);
#6376=VECTOR('',#23360,10.);
#6377=VECTOR('',#23365,10.);
#6378=VECTOR('',#23378,8.671875);
#6379=VECTOR('',#23399,13.867180376262);
#6380=VECTOR('',#23442,12.7315647249454);
#6381=VECTOR('',#23523,10.);
#6382=VECTOR('',#23526,10.);
#6383=VECTOR('',#23531,10.);
#6384=VECTOR('',#23532,10.);
#6385=VECTOR('',#23535,10.);
#6386=VECTOR('',#23538,10.);
#6387=VECTOR('',#23541,10.);
#6388=VECTOR('',#23544,10.);
#6389=VECTOR('',#23547,10.);
#6390=VECTOR('',#23550,10.);
#6391=VECTOR('',#23553,10.);
#6392=VECTOR('',#23556,10.);
#6393=VECTOR('',#23559,10.);
#6394=VECTOR('',#23562,10.);
#6395=VECTOR('',#23567,10.);
#6396=VECTOR('',#23568,10.);
#6397=VECTOR('',#23571,10.);
#6398=VECTOR('',#23574,10.);
#6399=VECTOR('',#23579,10.);
#6400=VECTOR('',#23580,10.);
#6401=VECTOR('',#23583,10.);
#6402=VECTOR('',#23586,10.);
#6403=VECTOR('',#23589,10.);
#6404=VECTOR('',#23592,10.);
#6405=VECTOR('',#23595,10.);
#6406=VECTOR('',#23598,10.);
#6407=VECTOR('',#23601,10.);
#6408=VECTOR('',#23604,10.);
#6409=VECTOR('',#23607,10.);
#6410=VECTOR('',#23610,10.);
#6411=VECTOR('',#23615,10.);
#6412=VECTOR('',#23616,10.);
#6413=VECTOR('',#23619,10.);
#6414=VECTOR('',#23620,10.);
#6415=VECTOR('',#23623,10.);
#6416=VECTOR('',#23624,10.);
#6417=VECTOR('',#23627,10.);
#6418=VECTOR('',#23628,10.);
#6419=VECTOR('',#23631,10.);
#6420=VECTOR('',#23632,10.);
#6421=VECTOR('',#23635,10.);
#6422=VECTOR('',#23636,10.);
#6423=VECTOR('',#23639,10.);
#6424=VECTOR('',#23640,10.);
#6425=VECTOR('',#23643,10.);
#6426=VECTOR('',#23644,10.);
#6427=VECTOR('',#23647,10.);
#6428=VECTOR('',#23648,10.);
#6429=VECTOR('',#23655,1000.);
#6430=VECTOR('',#23658,1000.);
#6431=VECTOR('',#23663,1000.);
#6432=VECTOR('',#23666,1000.);
#6433=VECTOR('',#23671,1000.);
#6434=VECTOR('',#23674,1000.);
#6435=VECTOR('',#23679,1000.);
#6436=VECTOR('',#23682,1000.);
#6437=VECTOR('',#23687,1000.);
#6438=VECTOR('',#23690,1000.);
#6439=VECTOR('',#23695,1000.);
#6440=VECTOR('',#23698,1000.);
#6441=VECTOR('',#23703,1000.);
#6442=VECTOR('',#23706,1000.);
#6443=VECTOR('',#23711,1000.);
#6444=VECTOR('',#23714,1000.);
#6445=VECTOR('',#23743,5.);
#6446=VECTOR('',#23748,5.);
#6447=VECTOR('',#23753,5.10805041359455);
#6448=VECTOR('',#23780,8.4375);
#6449=VECTOR('',#23783,8.4375);
#6450=VECTOR('',#23800,17.5);
#6451=VECTOR('',#23811,16.796875);
#6452=VECTOR('',#23818,17.0170281388728);
#6453=VECTOR('',#23831,15.625);
#6454=VECTOR('',#23834,15.625);
#6455=VECTOR('',#23885,8.671875);
#6456=VECTOR('',#23906,13.867180376262);
#6457=VECTOR('',#23955,12.7315647249454);
#6458=VECTOR('',#24028,10.);
#6459=VECTOR('',#24031,10.);
#6460=VECTOR('',#24036,10.);
#6461=VECTOR('',#24037,10.);
#6462=VECTOR('',#24040,10.);
#6463=VECTOR('',#24043,10.);
#6464=VECTOR('',#24046,10.);
#6465=VECTOR('',#24049,10.);
#6466=VECTOR('',#24052,10.);
#6467=VECTOR('',#24055,10.);
#6468=VECTOR('',#24058,10.);
#6469=VECTOR('',#24061,10.);
#6470=VECTOR('',#24064,10.);
#6471=VECTOR('',#24067,10.);
#6472=VECTOR('',#24072,10.);
#6473=VECTOR('',#24073,10.);
#6474=VECTOR('',#24076,10.);
#6475=VECTOR('',#24079,10.);
#6476=VECTOR('',#24084,10.);
#6477=VECTOR('',#24085,10.);
#6478=VECTOR('',#24088,10.);
#6479=VECTOR('',#24091,10.);
#6480=VECTOR('',#24094,10.);
#6481=VECTOR('',#24097,10.);
#6482=VECTOR('',#24100,10.);
#6483=VECTOR('',#24103,10.);
#6484=VECTOR('',#24106,10.);
#6485=VECTOR('',#24109,10.);
#6486=VECTOR('',#24112,10.);
#6487=VECTOR('',#24115,10.);
#6488=VECTOR('',#24120,10.);
#6489=VECTOR('',#24121,10.);
#6490=VECTOR('',#24124,10.);
#6491=VECTOR('',#24125,10.);
#6492=VECTOR('',#24128,10.);
#6493=VECTOR('',#24129,10.);
#6494=VECTOR('',#24132,10.);
#6495=VECTOR('',#24133,10.);
#6496=VECTOR('',#24136,10.);
#6497=VECTOR('',#24137,10.);
#6498=VECTOR('',#24140,10.);
#6499=VECTOR('',#24141,10.);
#6500=VECTOR('',#24144,10.);
#6501=VECTOR('',#24145,10.);
#6502=VECTOR('',#24148,10.);
#6503=VECTOR('',#24149,10.);
#6504=VECTOR('',#24152,10.);
#6505=VECTOR('',#24153,10.);
#6506=VECTOR('',#24160,1000.);
#6507=VECTOR('',#24163,1000.);
#6508=VECTOR('',#24168,1000.);
#6509=VECTOR('',#24171,1000.);
#6510=VECTOR('',#24176,1000.);
#6511=VECTOR('',#24179,1000.);
#6512=VECTOR('',#24184,1000.);
#6513=VECTOR('',#24187,1000.);
#6514=VECTOR('',#24192,1000.);
#6515=VECTOR('',#24195,1000.);
#6516=VECTOR('',#24200,1000.);
#6517=VECTOR('',#24203,1000.);
#6518=VECTOR('',#24208,1000.);
#6519=VECTOR('',#24211,1000.);
#6520=VECTOR('',#24216,1000.);
#6521=VECTOR('',#24219,1000.);
#6522=VECTOR('',#24226,10.);
#6523=VECTOR('',#24227,10.);
#6524=VECTOR('',#24228,10.);
#6525=VECTOR('',#24229,10.);
#6526=VECTOR('',#24232,10.);
#6527=VECTOR('',#24233,10.);
#6528=VECTOR('',#24234,10.);
#6529=VECTOR('',#24237,10.);
#6530=VECTOR('',#24238,10.);
#6531=VECTOR('',#24239,10.);
#6532=VECTOR('',#24242,10.);
#6533=VECTOR('',#24243,10.);
#6534=VECTOR('',#24244,10.);
#6535=VECTOR('',#24245,10.);
#6536=VECTOR('',#24248,10.);
#6537=VECTOR('',#24249,10.);
#6538=VECTOR('',#24250,10.);
#6539=VECTOR('',#24253,10.);
#6540=VECTOR('',#24254,10.);
#6541=VECTOR('',#24255,10.);
#6542=VECTOR('',#24258,10.);
#6543=VECTOR('',#24259,10.);
#6544=VECTOR('',#24260,10.);
#6545=VECTOR('',#24263,10.);
#6546=VECTOR('',#24264,10.);
#6547=VECTOR('',#24265,10.);
#6548=VECTOR('',#24268,10.);
#6549=VECTOR('',#24269,10.);
#6550=VECTOR('',#24270,10.);
#6551=VECTOR('',#24273,10.);
#6552=VECTOR('',#24274,10.);
#6553=VECTOR('',#24275,10.);
#6554=VECTOR('',#24276,10.);
#6555=VECTOR('',#24279,10.);
#6556=VECTOR('',#24280,10.);
#6557=VECTOR('',#24281,10.);
#6558=VECTOR('',#24284,10.);
#6559=VECTOR('',#24285,10.);
#6560=VECTOR('',#24286,10.);
#6561=VECTOR('',#24289,10.);
#6562=VECTOR('',#24290,10.);
#6563=VECTOR('',#24291,10.);
#6564=VECTOR('',#24294,10.);
#6565=VECTOR('',#24295,10.);
#6566=VECTOR('',#24296,10.);
#6567=VECTOR('',#24297,10.);
#6568=VECTOR('',#24300,10.);
#6569=VECTOR('',#24301,10.);
#6570=VECTOR('',#24302,10.);
#6571=VECTOR('',#24305,10.);
#6572=VECTOR('',#24306,10.);
#6573=VECTOR('',#24307,10.);
#6574=VECTOR('',#24310,10.);
#6575=VECTOR('',#24311,10.);
#6576=VECTOR('',#24312,10.);
#6577=VECTOR('',#24315,10.);
#6578=VECTOR('',#24316,10.);
#6579=VECTOR('',#24317,10.);
#6580=VECTOR('',#24320,10.);
#6581=VECTOR('',#24321,10.);
#6582=VECTOR('',#24324,10.);
#6583=VECTOR('',#24325,10.);
#6584=VECTOR('',#24326,10.);
#6585=VECTOR('',#24327,10.);
#6586=VECTOR('',#24330,10.);
#6587=VECTOR('',#24331,10.);
#6588=VECTOR('',#24332,10.);
#6589=VECTOR('',#24335,10.);
#6590=VECTOR('',#24336,10.);
#6591=VECTOR('',#24337,10.);
#6592=VECTOR('',#24340,10.);
#6593=VECTOR('',#24341,10.);
#6594=VECTOR('',#24344,10.);
#6595=VECTOR('',#24345,10.);
#6596=VECTOR('',#24346,10.);
#6597=VECTOR('',#24347,10.);
#6598=VECTOR('',#24350,10.);
#6599=VECTOR('',#24351,10.);
#6600=VECTOR('',#24352,10.);
#6601=VECTOR('',#24355,10.);
#6602=VECTOR('',#24356,10.);
#6603=VECTOR('',#24357,10.);
#6604=VECTOR('',#24360,10.);
#6605=VECTOR('',#24361,10.);
#6606=VECTOR('',#24362,10.);
#6607=VECTOR('',#24365,10.);
#6608=VECTOR('',#24366,10.);
#6609=VECTOR('',#24367,10.);
#6610=VECTOR('',#24370,10.);
#6611=VECTOR('',#24371,10.);
#6612=VECTOR('',#24372,10.);
#6613=VECTOR('',#24375,10.);
#6614=VECTOR('',#24376,10.);
#6615=VECTOR('',#24377,10.);
#6616=VECTOR('',#24378,10.);
#6617=VECTOR('',#24381,10.);
#6618=VECTOR('',#24382,10.);
#6619=VECTOR('',#24383,10.);
#6620=VECTOR('',#24386,10.);
#6621=VECTOR('',#24387,10.);
#6622=VECTOR('',#24388,10.);
#6623=VECTOR('',#24391,10.);
#6624=VECTOR('',#24392,10.);
#6625=VECTOR('',#24397,3.25);
#6626=VECTOR('',#24402,10.);
#6627=VECTOR('',#24403,10.);
#6628=VECTOR('',#24404,10.);
#6629=VECTOR('',#24407,10.);
#6630=VECTOR('',#24408,10.);
#6631=VECTOR('',#24409,10.);
#6632=VECTOR('',#24410,10.);
#6633=VECTOR('',#24413,10.);
#6634=VECTOR('',#24414,10.);
#6635=VECTOR('',#24415,10.);
#6636=VECTOR('',#24418,10.);
#6637=VECTOR('',#24419,10.);
#6638=VECTOR('',#24420,10.);
#6639=VECTOR('',#24423,10.);
#6640=VECTOR('',#24424,10.);
#6641=VECTOR('',#24425,10.);
#6642=VECTOR('',#24428,10.);
#6643=VECTOR('',#24429,10.);
#6644=VECTOR('',#24430,10.);
#6645=VECTOR('',#24433,10.);
#6646=VECTOR('',#24434,10.);
#6647=VECTOR('',#24437,10.);
#6648=VECTOR('',#24438,10.);
#6649=VECTOR('',#24439,10.);
#6650=VECTOR('',#24440,10.);
#6651=VECTOR('',#24447,10.);
#6652=VECTOR('',#24450,10.);
#6653=VECTOR('',#24451,10.);
#6654=VECTOR('',#24452,10.);
#6655=VECTOR('',#24459,10.);
#6656=VECTOR('',#24462,10.);
#6657=VECTOR('',#24463,10.);
#6658=VECTOR('',#24464,10.);
#6659=VECTOR('',#24465,10.);
#6660=VECTOR('',#24468,10.);
#6661=VECTOR('',#24469,10.);
#6662=VECTOR('',#24470,10.);
#6663=VECTOR('',#24473,10.);
#6664=VECTOR('',#24474,10.);
#6665=VECTOR('',#24475,10.);
#6666=VECTOR('',#24478,10.);
#6667=VECTOR('',#24479,10.);
#6668=VECTOR('',#24480,10.);
#6669=VECTOR('',#24483,10.);
#6670=VECTOR('',#24484,10.);
#6671=VECTOR('',#24485,10.);
#6672=VECTOR('',#24488,10.);
#6673=VECTOR('',#24489,10.);
#6674=VECTOR('',#24490,10.);
#6675=VECTOR('',#24493,10.);
#6676=VECTOR('',#24494,10.);
#6677=VECTOR('',#24497,10.);
#6678=VECTOR('',#24498,10.);
#6679=VECTOR('',#24499,10.);
#6680=VECTOR('',#24502,10.);
#6681=VECTOR('',#24503,10.);
#6682=VECTOR('',#24504,10.);
#6683=VECTOR('',#24507,10.);
#6684=VECTOR('',#24508,10.);
#6685=VECTOR('',#24509,10.);
#6686=VECTOR('',#24512,10.);
#6687=VECTOR('',#24513,10.);
#6688=VECTOR('',#24514,10.);
#6689=VECTOR('',#24519,10.);
#6690=VECTOR('',#24524,10.);
#6691=VECTOR('',#24525,10.);
#6692=VECTOR('',#24526,10.);
#6693=VECTOR('',#24531,10.);
#6694=VECTOR('',#24536,10.);
#6695=VECTOR('',#24537,10.);
#6696=VECTOR('',#24540,10.);
#6697=VECTOR('',#24541,10.);
#6698=VECTOR('',#24542,10.);
#6699=VECTOR('',#24545,10.);
#6700=VECTOR('',#24546,10.);
#6701=VECTOR('',#24547,10.);
#6702=VECTOR('',#24550,10.);
#6703=VECTOR('',#24551,10.);
#6704=VECTOR('',#24552,10.);
#6705=VECTOR('',#24555,10.);
#6706=VECTOR('',#24556,10.);
#6707=VECTOR('',#24557,10.);
#6708=VECTOR('',#24560,10.);
#6709=VECTOR('',#24561,10.);
#6710=VECTOR('',#24562,10.);
#6711=VECTOR('',#24565,10.);
#6712=VECTOR('',#24566,10.);
#6713=VECTOR('',#24567,10.);
#6714=VECTOR('',#24570,10.);
#6715=VECTOR('',#24571,10.);
#6716=VECTOR('',#24572,10.);
#6717=VECTOR('',#24575,10.);
#6718=VECTOR('',#24576,10.);
#6719=VECTOR('',#24577,10.);
#6720=VECTOR('',#24582,10.);
#6721=VECTOR('',#24587,10.);
#6722=VECTOR('',#24588,10.);
#6723=VECTOR('',#24589,10.);
#6724=VECTOR('',#24592,10.);
#6725=VECTOR('',#24593,10.);
#6726=VECTOR('',#24594,10.);
#6727=VECTOR('',#24597,10.);
#6728=VECTOR('',#24598,10.);
#6729=VECTOR('',#24599,10.);
#6730=VECTOR('',#24602,10.);
#6731=VECTOR('',#24603,10.);
#6732=VECTOR('',#24604,10.);
#6733=VECTOR('',#24607,10.);
#6734=VECTOR('',#24608,10.);
#6735=VECTOR('',#24609,10.);
#6736=VECTOR('',#24612,10.);
#6737=VECTOR('',#24613,10.);
#6738=VECTOR('',#24614,10.);
#6739=VECTOR('',#24617,10.);
#6740=VECTOR('',#24618,10.);
#6741=VECTOR('',#24619,10.);
#6742=VECTOR('',#24622,10.);
#6743=VECTOR('',#24623,10.);
#6744=VECTOR('',#24624,10.);
#6745=VECTOR('',#24625,10.);
#6746=VECTOR('',#24630,10.);
#6747=VECTOR('',#24635,10.);
#6748=VECTOR('',#24636,10.);
#6749=VECTOR('',#24637,10.);
#6750=VECTOR('',#24642,10.);
#6751=VECTOR('',#24647,10.);
#6752=VECTOR('',#24648,10.);
#6753=VECTOR('',#24649,10.);
#6754=VECTOR('',#24650,10.);
#6755=VECTOR('',#24653,10.);
#6756=VECTOR('',#24654,10.);
#6757=VECTOR('',#24655,10.);
#6758=VECTOR('',#24658,10.);
#6759=VECTOR('',#24659,10.);
#6760=VECTOR('',#24660,10.);
#6761=VECTOR('',#24663,10.);
#6762=VECTOR('',#24664,10.);
#6763=VECTOR('',#24665,10.);
#6764=VECTOR('',#24668,10.);
#6765=VECTOR('',#24669,10.);
#6766=VECTOR('',#24670,10.);
#6767=VECTOR('',#24673,10.);
#6768=VECTOR('',#24674,10.);
#6769=VECTOR('',#24675,10.);
#6770=VECTOR('',#24678,10.);
#6771=VECTOR('',#24679,10.);
#6772=VECTOR('',#24682,10.);
#6773=VECTOR('',#24683,10.);
#6774=VECTOR('',#24684,10.);
#6775=VECTOR('',#24687,10.);
#6776=VECTOR('',#24688,10.);
#6777=VECTOR('',#24689,10.);
#6778=VECTOR('',#24692,10.);
#6779=VECTOR('',#24693,10.);
#6780=VECTOR('',#24694,10.);
#6781=VECTOR('',#24697,10.);
#6782=VECTOR('',#24698,10.);
#6783=VECTOR('',#24699,10.);
#6784=VECTOR('',#24702,10.);
#6785=VECTOR('',#24703,10.);
#6786=VECTOR('',#24708,3.25);
#6787=VECTOR('',#24713,10.);
#6788=VECTOR('',#24714,10.);
#6789=VECTOR('',#24715,10.);
#6790=VECTOR('',#24722,10.);
#6791=VECTOR('',#24725,10.);
#6792=VECTOR('',#24726,10.);
#6793=VECTOR('',#24727,10.);
#6794=VECTOR('',#24734,10.);
#6795=VECTOR('',#24737,10.);
#6796=VECTOR('',#24738,10.);
#6797=VECTOR('',#24741,10.);
#6798=VECTOR('',#24742,10.);
#6799=VECTOR('',#24743,10.);
#6800=VECTOR('',#24746,10.);
#6801=VECTOR('',#24747,10.);
#6802=VECTOR('',#24748,10.);
#6803=VECTOR('',#24751,10.);
#6804=VECTOR('',#24752,10.);
#6805=VECTOR('',#24753,10.);
#6806=VECTOR('',#24756,10.);
#6807=VECTOR('',#24757,10.);
#6808=VECTOR('',#24758,10.);
#6809=VECTOR('',#24761,10.);
#6810=VECTOR('',#24762,10.);
#6811=VECTOR('',#24763,10.);
#6812=VECTOR('',#24766,10.);
#6813=VECTOR('',#24767,10.);
#6814=VECTOR('',#24768,10.);
#6815=VECTOR('',#24771,10.);
#6816=VECTOR('',#24772,10.);
#6817=VECTOR('',#24773,10.);
#6818=VECTOR('',#24776,10.);
#6819=VECTOR('',#24777,10.);
#6820=VECTOR('',#24778,10.);
#6821=VECTOR('',#24785,10.);
#6822=VECTOR('',#24788,10.);
#6823=VECTOR('',#24789,10.);
#6824=VECTOR('',#24790,10.);
#6825=VECTOR('',#24793,10.);
#6826=VECTOR('',#24794,10.);
#6827=VECTOR('',#24795,10.);
#6828=VECTOR('',#24798,10.);
#6829=VECTOR('',#24799,10.);
#6830=VECTOR('',#24800,10.);
#6831=VECTOR('',#24803,10.);
#6832=VECTOR('',#24804,10.);
#6833=VECTOR('',#24805,10.);
#6834=VECTOR('',#24808,10.);
#6835=VECTOR('',#24809,10.);
#6836=VECTOR('',#24810,10.);
#6837=VECTOR('',#24813,10.);
#6838=VECTOR('',#24814,10.);
#6839=VECTOR('',#24815,10.);
#6840=VECTOR('',#24818,10.);
#6841=VECTOR('',#24819,10.);
#6842=VECTOR('',#24822,10.);
#6843=VECTOR('',#24823,10.);
#6844=VECTOR('',#24824,10.);
#6845=VECTOR('',#24825,10.);
#6846=VECTOR('',#24828,10.);
#6847=VECTOR('',#24829,10.);
#6848=VECTOR('',#24830,10.);
#6849=VECTOR('',#24833,10.);
#6850=VECTOR('',#24834,10.);
#6851=VECTOR('',#24835,10.);
#6852=VECTOR('',#24838,10.);
#6853=VECTOR('',#24839,10.);
#6854=VECTOR('',#24840,10.);
#6855=VECTOR('',#24841,10.);
#6856=VECTOR('',#24844,10.);
#6857=VECTOR('',#24845,10.);
#6858=VECTOR('',#24846,10.);
#6859=VECTOR('',#24849,10.);
#6860=VECTOR('',#24850,10.);
#6861=VECTOR('',#24851,10.);
#6862=VECTOR('',#24854,10.);
#6863=VECTOR('',#24855,10.);
#6864=VECTOR('',#24856,10.);
#6865=VECTOR('',#24859,10.);
#6866=VECTOR('',#24860,10.);
#6867=VECTOR('',#24861,10.);
#6868=VECTOR('',#24864,10.);
#6869=VECTOR('',#24865,10.);
#6870=VECTOR('',#24866,10.);
#6871=VECTOR('',#24869,10.);
#6872=VECTOR('',#24870,10.);
#6873=VECTOR('',#24871,10.);
#6874=VECTOR('',#24874,10.);
#6875=VECTOR('',#24875,10.);
#6876=VECTOR('',#24876,10.);
#6877=VECTOR('',#24879,10.);
#6878=VECTOR('',#24880,10.);
#6879=VECTOR('',#24881,10.);
#6880=VECTOR('',#24884,10.);
#6881=VECTOR('',#24885,10.);
#6882=VECTOR('',#24886,10.);
#6883=VECTOR('',#24889,10.);
#6884=VECTOR('',#24890,10.);
#6885=VECTOR('',#24891,10.);
#6886=VECTOR('',#24894,10.);
#6887=VECTOR('',#24895,10.);
#6888=VECTOR('',#24896,10.);
#6889=VECTOR('',#24899,10.);
#6890=VECTOR('',#24900,10.);
#6891=VECTOR('',#24901,10.);
#6892=VECTOR('',#24904,10.);
#6893=VECTOR('',#24905,10.);
#6894=VECTOR('',#24906,10.);
#6895=VECTOR('',#24909,10.);
#6896=VECTOR('',#24910,10.);
#6897=VECTOR('',#24911,10.);
#6898=VECTOR('',#24914,10.);
#6899=VECTOR('',#24915,10.);
#6900=VECTOR('',#24916,10.);
#6901=VECTOR('',#24919,10.);
#6902=VECTOR('',#24920,10.);
#6903=VECTOR('',#24921,10.);
#6904=VECTOR('',#24924,10.);
#6905=VECTOR('',#24925,10.);
#6906=VECTOR('',#24928,10.);
#6907=VECTOR('',#24929,10.);
#6908=VECTOR('',#24930,10.);
#6909=VECTOR('',#24931,10.);
#6910=VECTOR('',#24934,10.);
#6911=VECTOR('',#24935,10.);
#6912=VECTOR('',#24936,10.);
#6913=VECTOR('',#24939,10.);
#6914=VECTOR('',#24940,10.);
#6915=VECTOR('',#24941,10.);
#6916=VECTOR('',#24944,10.);
#6917=VECTOR('',#24945,10.);
#6918=VECTOR('',#24948,10.);
#6919=VECTOR('',#24949,10.);
#6920=VECTOR('',#24950,10.);
#6921=VECTOR('',#24951,10.);
#6922=VECTOR('',#24954,10.);
#6923=VECTOR('',#24955,10.);
#6924=VECTOR('',#24956,10.);
#6925=VECTOR('',#24959,10.);
#6926=VECTOR('',#24960,10.);
#6927=VECTOR('',#24961,10.);
#6928=VECTOR('',#24964,10.);
#6929=VECTOR('',#24965,10.);
#6930=VECTOR('',#24966,10.);
#6931=VECTOR('',#24969,10.);
#6932=VECTOR('',#24970,10.);
#6933=VECTOR('',#24971,10.);
#6934=VECTOR('',#24974,10.);
#6935=VECTOR('',#24975,10.);
#6936=VECTOR('',#24976,10.);
#6937=VECTOR('',#24979,10.);
#6938=VECTOR('',#24980,10.);
#6939=VECTOR('',#24981,10.);
#6940=VECTOR('',#24984,10.);
#6941=VECTOR('',#24985,10.);
#6942=VECTOR('',#24986,10.);
#6943=VECTOR('',#24989,10.);
#6944=VECTOR('',#24990,10.);
#6945=VECTOR('',#24991,10.);
#6946=VECTOR('',#24994,10.);
#6947=VECTOR('',#24995,10.);
#6948=VECTOR('',#24996,10.);
#6949=VECTOR('',#24999,10.);
#6950=VECTOR('',#25000,10.);
#6951=VECTOR('',#25005,3.25);
#6952=VECTOR('',#25010,10.);
#6953=VECTOR('',#25011,10.);
#6954=VECTOR('',#25012,10.);
#6955=VECTOR('',#25015,10.);
#6956=VECTOR('',#25016,10.);
#6957=VECTOR('',#25017,10.);
#6958=VECTOR('',#25020,10.);
#6959=VECTOR('',#25021,10.);
#6960=VECTOR('',#25022,10.);
#6961=VECTOR('',#25025,10.);
#6962=VECTOR('',#25026,10.);
#6963=VECTOR('',#25027,10.);
#6964=VECTOR('',#25030,10.);
#6965=VECTOR('',#25031,10.);
#6966=VECTOR('',#25032,10.);
#6967=VECTOR('',#25035,10.);
#6968=VECTOR('',#25036,10.);
#6969=VECTOR('',#25037,10.);
#6970=VECTOR('',#25040,10.);
#6971=VECTOR('',#25041,10.);
#6972=VECTOR('',#25042,10.);
#6973=VECTOR('',#25045,10.);
#6974=VECTOR('',#25046,10.);
#6975=VECTOR('',#25049,10.);
#6976=VECTOR('',#25050,10.);
#6977=VECTOR('',#25051,10.);
#6978=VECTOR('',#25052,10.);
#6979=VECTOR('',#25055,10.);
#6980=VECTOR('',#25056,10.);
#6981=VECTOR('',#25057,10.);
#6982=VECTOR('',#25060,10.);
#6983=VECTOR('',#25061,10.);
#6984=VECTOR('',#25062,10.);
#6985=VECTOR('',#25065,10.);
#6986=VECTOR('',#25066,10.);
#6987=VECTOR('',#25067,10.);
#6988=VECTOR('',#25068,10.);
#6989=VECTOR('',#25071,10.);
#6990=VECTOR('',#25072,10.);
#6991=VECTOR('',#25073,10.);
#6992=VECTOR('',#25076,10.);
#6993=VECTOR('',#25077,10.);
#6994=VECTOR('',#25078,10.);
#6995=VECTOR('',#25081,10.);
#6996=VECTOR('',#25082,10.);
#6997=VECTOR('',#25083,10.);
#6998=VECTOR('',#25086,10.);
#6999=VECTOR('',#25087,10.);
#7000=VECTOR('',#25088,10.);
#7001=VECTOR('',#25091,10.);
#7002=VECTOR('',#25092,10.);
#7003=VECTOR('',#25093,10.);
#7004=VECTOR('',#25096,10.);
#7005=VECTOR('',#25097,10.);
#7006=VECTOR('',#25098,10.);
#7007=VECTOR('',#25101,10.);
#7008=VECTOR('',#25102,10.);
#7009=VECTOR('',#25103,10.);
#7010=VECTOR('',#25106,10.);
#7011=VECTOR('',#25107,10.);
#7012=VECTOR('',#25108,10.);
#7013=VECTOR('',#25111,10.);
#7014=VECTOR('',#25112,10.);
#7015=VECTOR('',#25113,10.);
#7016=VECTOR('',#25116,10.);
#7017=VECTOR('',#25117,10.);
#7018=VECTOR('',#25118,10.);
#7019=VECTOR('',#25121,10.);
#7020=VECTOR('',#25122,10.);
#7021=VECTOR('',#25123,10.);
#7022=VECTOR('',#25126,10.);
#7023=VECTOR('',#25127,10.);
#7024=VECTOR('',#25128,10.);
#7025=VECTOR('',#25131,10.);
#7026=VECTOR('',#25132,10.);
#7027=VECTOR('',#25133,10.);
#7028=VECTOR('',#25136,10.);
#7029=VECTOR('',#25137,10.);
#7030=VECTOR('',#25138,10.);
#7031=VECTOR('',#25141,10.);
#7032=VECTOR('',#25142,10.);
#7033=VECTOR('',#25143,10.);
#7034=VECTOR('',#25146,10.);
#7035=VECTOR('',#25147,10.);
#7036=VECTOR('',#25148,10.);
#7037=VECTOR('',#25151,10.);
#7038=VECTOR('',#25152,10.);
#7039=VECTOR('',#25155,10.);
#7040=VECTOR('',#25156,10.);
#7041=VECTOR('',#25157,10.);
#7042=VECTOR('',#25158,10.);
#7043=VECTOR('',#25161,10.);
#7044=VECTOR('',#25162,10.);
#7045=VECTOR('',#25163,10.);
#7046=VECTOR('',#25166,10.);
#7047=VECTOR('',#25167,10.);
#7048=VECTOR('',#25168,10.);
#7049=VECTOR('',#25171,10.);
#7050=VECTOR('',#25172,10.);
#7051=VECTOR('',#25175,10.);
#7052=VECTOR('',#25176,10.);
#7053=VECTOR('',#25177,10.);
#7054=VECTOR('',#25178,10.);
#7055=VECTOR('',#25181,10.);
#7056=VECTOR('',#25182,10.);
#7057=VECTOR('',#25183,10.);
#7058=VECTOR('',#25186,10.);
#7059=VECTOR('',#25187,10.);
#7060=VECTOR('',#25188,10.);
#7061=VECTOR('',#25191,10.);
#7062=VECTOR('',#25192,10.);
#7063=VECTOR('',#25193,10.);
#7064=VECTOR('',#25196,10.);
#7065=VECTOR('',#25197,10.);
#7066=VECTOR('',#25198,10.);
#7067=VECTOR('',#25201,10.);
#7068=VECTOR('',#25202,10.);
#7069=VECTOR('',#25203,10.);
#7070=VECTOR('',#25206,10.);
#7071=VECTOR('',#25207,10.);
#7072=VECTOR('',#25208,10.);
#7073=VECTOR('',#25211,10.);
#7074=VECTOR('',#25212,10.);
#7075=VECTOR('',#25213,10.);
#7076=VECTOR('',#25216,10.);
#7077=VECTOR('',#25217,10.);
#7078=VECTOR('',#25218,10.);
#7079=VECTOR('',#25221,10.);
#7080=VECTOR('',#25222,10.);
#7081=VECTOR('',#25223,10.);
#7082=VECTOR('',#25226,10.);
#7083=VECTOR('',#25227,10.);
#7084=VECTOR('',#25232,3.25);
#7085=VECTOR('',#25237,10.);
#7086=VECTOR('',#25238,10.);
#7087=VECTOR('',#25239,10.);
#7088=VECTOR('',#25242,10.);
#7089=VECTOR('',#25243,10.);
#7090=VECTOR('',#25244,10.);
#7091=VECTOR('',#25247,10.);
#7092=VECTOR('',#25248,10.);
#7093=VECTOR('',#25249,10.);
#7094=VECTOR('',#25252,10.);
#7095=VECTOR('',#25253,10.);
#7096=VECTOR('',#25254,10.);
#7097=VECTOR('',#25257,10.);
#7098=VECTOR('',#25258,10.);
#7099=VECTOR('',#25259,10.);
#7100=VECTOR('',#25262,10.);
#7101=VECTOR('',#25263,10.);
#7102=VECTOR('',#25264,10.);
#7103=VECTOR('',#25267,10.);
#7104=VECTOR('',#25268,10.);
#7105=VECTOR('',#25269,10.);
#7106=VECTOR('',#25272,10.);
#7107=VECTOR('',#25273,10.);
#7108=VECTOR('',#25276,10.);
#7109=VECTOR('',#25277,10.);
#7110=VECTOR('',#25278,10.);
#7111=VECTOR('',#25279,10.);
#7112=VECTOR('',#25286,10.);
#7113=VECTOR('',#25289,10.);
#7114=VECTOR('',#25290,10.);
#7115=VECTOR('',#25291,10.);
#7116=VECTOR('',#25298,10.);
#7117=VECTOR('',#25301,10.);
#7118=VECTOR('',#25302,10.);
#7119=VECTOR('',#25303,10.);
#7120=VECTOR('',#25304,10.);
#7121=VECTOR('',#25307,10.);
#7122=VECTOR('',#25308,10.);
#7123=VECTOR('',#25309,10.);
#7124=VECTOR('',#25312,10.);
#7125=VECTOR('',#25313,10.);
#7126=VECTOR('',#25314,10.);
#7127=VECTOR('',#25317,10.);
#7128=VECTOR('',#25318,10.);
#7129=VECTOR('',#25319,10.);
#7130=VECTOR('',#25322,10.);
#7131=VECTOR('',#25323,10.);
#7132=VECTOR('',#25324,10.);
#7133=VECTOR('',#25327,10.);
#7134=VECTOR('',#25328,10.);
#7135=VECTOR('',#25329,10.);
#7136=VECTOR('',#25332,10.);
#7137=VECTOR('',#25333,10.);
#7138=VECTOR('',#25336,10.);
#7139=VECTOR('',#25337,10.);
#7140=VECTOR('',#25338,10.);
#7141=VECTOR('',#25341,10.);
#7142=VECTOR('',#25342,10.);
#7143=VECTOR('',#25343,10.);
#7144=VECTOR('',#25346,10.);
#7145=VECTOR('',#25347,10.);
#7146=VECTOR('',#25348,10.);
#7147=VECTOR('',#25351,10.);
#7148=VECTOR('',#25352,10.);
#7149=VECTOR('',#25353,10.);
#7150=VECTOR('',#25358,10.);
#7151=VECTOR('',#25363,10.);
#7152=VECTOR('',#25364,10.);
#7153=VECTOR('',#25365,10.);
#7154=VECTOR('',#25370,10.);
#7155=VECTOR('',#25375,10.);
#7156=VECTOR('',#25376,10.);
#7157=VECTOR('',#25379,10.);
#7158=VECTOR('',#25380,10.);
#7159=VECTOR('',#25381,10.);
#7160=VECTOR('',#25384,10.);
#7161=VECTOR('',#25385,10.);
#7162=VECTOR('',#25386,10.);
#7163=VECTOR('',#25389,10.);
#7164=VECTOR('',#25390,10.);
#7165=VECTOR('',#25391,10.);
#7166=VECTOR('',#25394,10.);
#7167=VECTOR('',#25395,10.);
#7168=VECTOR('',#25396,10.);
#7169=VECTOR('',#25399,10.);
#7170=VECTOR('',#25400,10.);
#7171=VECTOR('',#25401,10.);
#7172=VECTOR('',#25404,10.);
#7173=VECTOR('',#25405,10.);
#7174=VECTOR('',#25406,10.);
#7175=VECTOR('',#25409,10.);
#7176=VECTOR('',#25410,10.);
#7177=VECTOR('',#25411,10.);
#7178=VECTOR('',#25414,10.);
#7179=VECTOR('',#25415,10.);
#7180=VECTOR('',#25416,10.);
#7181=VECTOR('',#25421,10.);
#7182=VECTOR('',#25426,10.);
#7183=VECTOR('',#25427,10.);
#7184=VECTOR('',#25428,10.);
#7185=VECTOR('',#25431,10.);
#7186=VECTOR('',#25432,10.);
#7187=VECTOR('',#25433,10.);
#7188=VECTOR('',#25436,10.);
#7189=VECTOR('',#25437,10.);
#7190=VECTOR('',#25438,10.);
#7191=VECTOR('',#25441,10.);
#7192=VECTOR('',#25442,10.);
#7193=VECTOR('',#25443,10.);
#7194=VECTOR('',#25446,10.);
#7195=VECTOR('',#25447,10.);
#7196=VECTOR('',#25448,10.);
#7197=VECTOR('',#25451,10.);
#7198=VECTOR('',#25452,10.);
#7199=VECTOR('',#25453,10.);
#7200=VECTOR('',#25456,10.);
#7201=VECTOR('',#25457,10.);
#7202=VECTOR('',#25458,10.);
#7203=VECTOR('',#25461,10.);
#7204=VECTOR('',#25462,10.);
#7205=VECTOR('',#25463,10.);
#7206=VECTOR('',#25464,10.);
#7207=VECTOR('',#25465,10.);
#7208=VECTOR('',#25466,10.);
#7209=VECTOR('',#25467,10.);
#7210=VECTOR('',#25468,10.);
#7211=VECTOR('',#25469,10.);
#7212=VECTOR('',#25470,10.);
#7213=VECTOR('',#25471,10.);
#7214=VECTOR('',#25472,10.);
#7215=VECTOR('',#25473,10.);
#7216=VECTOR('',#25474,10.);
#7217=VECTOR('',#25475,10.);
#7218=VECTOR('',#25478,10.);
#7219=VECTOR('',#25479,10.);
#7220=VECTOR('',#25480,10.);
#7221=VECTOR('',#25481,10.);
#7222=VECTOR('',#25482,10.);
#7223=VECTOR('',#25483,10.);
#7224=VECTOR('',#25484,10.);
#7225=VECTOR('',#25485,10.);
#7226=VECTOR('',#25486,10.);
#7227=VECTOR('',#25487,10.);
#7228=VECTOR('',#25488,10.);
#7229=VECTOR('',#25489,10.);
#7230=VECTOR('',#25490,10.);
#7231=VECTOR('',#25493,10.);
#7232=VECTOR('',#25496,10.);
#7233=VECTOR('',#25499,10.);
#7234=VECTOR('',#25502,10.);
#7235=VECTOR('',#25507,10.);
#7236=VECTOR('',#25508,10.);
#7237=VECTOR('',#25509,10.);
#7238=VECTOR('',#25512,10.);
#7239=VECTOR('',#25517,10.);
#7240=VECTOR('',#25518,10.);
#7241=VECTOR('',#25521,10.);
#7242=VECTOR('',#25526,10.);
#7243=VECTOR('',#25527,10.);
#7244=VECTOR('',#25528,10.);
#7245=VECTOR('',#25531,10.);
#7246=VECTOR('',#25532,10.);
#7247=VECTOR('',#25535,10.);
#7248=VECTOR('',#25536,10.);
#7249=VECTOR('',#25539,10.);
#7250=VECTOR('',#25540,10.);
#7251=VECTOR('',#25543,10.);
#7252=VECTOR('',#25544,10.);
#7253=VECTOR('',#25547,10.);
#7254=VECTOR('',#25548,10.);
#7255=VECTOR('',#25551,10.);
#7256=VECTOR('',#25554,10.);
#7257=VECTOR('',#25555,10.);
#7258=VECTOR('',#25558,10.);
#7259=VECTOR('',#25559,10.);
#7260=VECTOR('',#25562,10.);
#7261=VECTOR('',#25563,10.);
#7262=VECTOR('',#25566,10.);
#7263=VECTOR('',#25567,10.);
#7264=VECTOR('',#25570,10.);
#7265=VECTOR('',#25575,3.25);
#7266=VECTOR('',#25578,10.);
#7267=VECTOR('',#25579,10.);
#7268=VECTOR('',#25584,10.);
#7269=VECTOR('',#25587,10.);
#7270=VECTOR('',#25588,10.);
#7271=VECTOR('',#25593,10.);
#7272=VECTOR('',#25596,10.);
#7273=VECTOR('',#25599,10.);
#7274=VECTOR('',#25600,10.);
#7275=VECTOR('',#25603,10.);
#7276=VECTOR('',#25604,10.);
#7277=VECTOR('',#25607,10.);
#7278=VECTOR('',#25608,10.);
#7279=VECTOR('',#25611,10.);
#7280=VECTOR('',#25612,10.);
#7281=VECTOR('',#25615,10.);
#7282=VECTOR('',#25616,10.);
#7283=VECTOR('',#25619,10.);
#7284=VECTOR('',#25620,10.);
#7285=VECTOR('',#25623,10.);
#7286=VECTOR('',#25624,10.);
#7287=VECTOR('',#25627,10.);
#7288=VECTOR('',#25628,10.);
#7289=VECTOR('',#25633,10.);
#7290=VECTOR('',#25636,10.);
#7291=VECTOR('',#25637,10.);
#7292=VECTOR('',#25640,10.);
#7293=VECTOR('',#25641,10.);
#7294=VECTOR('',#25644,10.);
#7295=VECTOR('',#25645,10.);
#7296=VECTOR('',#25648,10.);
#7297=VECTOR('',#25649,10.);
#7298=VECTOR('',#25652,10.);
#7299=VECTOR('',#25653,10.);
#7300=VECTOR('',#25656,10.);
#7301=VECTOR('',#25657,10.);
#7302=VECTOR('',#25660,10.);
#7303=VECTOR('',#25667,8.00000000000001);
#7304=VECTOR('',#25672,8.00000000000001);
#7305=VECTOR('',#25675,8.00000000000001);
#7306=VECTOR('',#25678,8.00000000000001);
#7307=VECTOR('',#25681,8.00000000000001);
#7308=VECTOR('',#25684,8.00000000000001);
#7309=VECTOR('',#25687,8.00000000000001);
#7310=VECTOR('',#25690,8.00000000000001);
#7311=VECTOR('',#25693,8.00000000000001);
#7312=VECTOR('',#25696,8.00000000000001);
#7313=VECTOR('',#25699,8.00000000000001);
#7314=VECTOR('',#25702,8.00000000000001);
#7315=VECTOR('',#25705,8.00000000000001);
#7316=VECTOR('',#25708,8.00000000000001);
#7317=VECTOR('',#25711,8.00000000000001);
#7318=VECTOR('',#25714,8.00000000000001);
#7319=VECTOR('',#25717,8.00000000000001);
#7320=VECTOR('',#25720,8.00000000000001);
#7321=VECTOR('',#25723,8.00000000000001);
#7322=VECTOR('',#25726,8.00000000000001);
#7323=VECTOR('',#25729,8.00000000000001);
#7324=VECTOR('',#25732,8.00000000000001);
#7325=VECTOR('',#25735,8.00000000000001);
#7326=VECTOR('',#25738,8.00000000000001);
#7327=VECTOR('',#25741,8.00000000000001);
#7328=VECTOR('',#25744,8.00000000000001);
#7329=VECTOR('',#25747,8.00000000000001);
#7330=VECTOR('',#25750,8.00000000000001);
#7331=VECTOR('',#25753,8.00000000000001);
#7332=VECTOR('',#25756,8.00000000000001);
#7333=VECTOR('',#25759,8.00000000000001);
#7334=VECTOR('',#25762,8.00000000000001);
#7335=VECTOR('',#25765,8.00000000000001);
#7336=VECTOR('',#25768,8.00000000000001);
#7337=VECTOR('',#25771,8.00000000000001);
#7338=VECTOR('',#25774,8.00000000000001);
#7339=VECTOR('',#25777,8.00000000000001);
#7340=VECTOR('',#25780,8.00000000000001);
#7341=VECTOR('',#25783,8.00000000000001);
#7342=VECTOR('',#25786,8.00000000000001);
#7343=VECTOR('',#25789,8.00000000000001);
#7344=VECTOR('',#25792,8.00000000000001);
#7345=VECTOR('',#25795,8.00000000000001);
#7346=VECTOR('',#25798,8.00000000000001);
#7347=VECTOR('',#25801,8.00000000000001);
#7348=VECTOR('',#25804,8.00000000000001);
#7349=VECTOR('',#25807,8.00000000000001);
#7350=VECTOR('',#25810,8.00000000000001);
#7351=VECTOR('',#25813,8.00000000000001);
#7352=VECTOR('',#25816,8.00000000000001);
#7353=VECTOR('',#25819,8.00000000000001);
#7354=VECTOR('',#25822,8.00000000000001);
#7355=VECTOR('',#25825,8.00000000000001);
#7356=VECTOR('',#25828,8.00000000000001);
#7357=VECTOR('',#25831,8.00000000000001);
#7358=VECTOR('',#25834,8.00000000000001);
#7359=VECTOR('',#25837,8.00000000000001);
#7360=VECTOR('',#25840,8.00000000000001);
#7361=VECTOR('',#25843,8.00000000000001);
#7362=VECTOR('',#25846,8.00000000000001);
#7363=VECTOR('',#25849,8.00000000000001);
#7364=VECTOR('',#25852,8.00000000000001);
#7365=VECTOR('',#25855,8.00000000000001);
#7366=VECTOR('',#25858,8.00000000000001);
#7367=VECTOR('',#25861,8.00000000000001);
#7368=VECTOR('',#25864,8.00000000000001);
#7369=VECTOR('',#25867,8.00000000000001);
#7370=VECTOR('',#25870,8.00000000000001);
#7371=VECTOR('',#25873,8.00000000000001);
#7372=VECTOR('',#25876,8.00000000000001);
#7373=VECTOR('',#25879,8.00000000000001);
#7374=VECTOR('',#25882,8.00000000000001);
#7375=VECTOR('',#25885,8.00000000000001);
#7376=VECTOR('',#25888,8.00000000000001);
#7377=VECTOR('',#25891,8.00000000000001);
#7378=VECTOR('',#25894,8.00000000000001);
#7379=VECTOR('',#25897,8.00000000000001);
#7380=VECTOR('',#25900,8.00000000000001);
#7381=VECTOR('',#25903,8.00000000000001);
#7382=VECTOR('',#25906,8.00000000000001);
#7383=VECTOR('',#25909,8.00000000000001);
#7384=VECTOR('',#25912,8.00000000000001);
#7385=VECTOR('',#25915,8.00000000000001);
#7386=VECTOR('',#25918,8.00000000000001);
#7387=VECTOR('',#25921,8.00000000000001);
#7388=VECTOR('',#25924,8.00000000000001);
#7389=VECTOR('',#25927,8.00000000000001);
#7390=VECTOR('',#25930,8.00000000000001);
#7391=VECTOR('',#25933,8.00000000000001);
#7392=VECTOR('',#25936,8.00000000000001);
#7393=VECTOR('',#25939,8.00000000000001);
#7394=VECTOR('',#25942,8.00000000000001);
#7395=VECTOR('',#25945,8.00000000000001);
#7396=VECTOR('',#25948,8.00000000000001);
#7397=VECTOR('',#25951,8.00000000000001);
#7398=VECTOR('',#25954,8.00000000000001);
#7399=VECTOR('',#25957,8.00000000000001);
#7400=VECTOR('',#25960,8.00000000000001);
#7401=VECTOR('',#25963,8.00000000000001);
#7402=VECTOR('',#25966,8.00000000000001);
#7403=VECTOR('',#25969,8.00000000000001);
#7404=VECTOR('',#25974,6.);
#7405=VECTOR('',#25975,6.);
#7406=VECTOR('',#25982,6.);
#7407=VECTOR('',#25985,6.);
#7408=VECTOR('',#25988,6.);
#7409=VECTOR('',#25991,6.);
#7410=VECTOR('',#25994,6.);
#7411=VECTOR('',#25997,6.);
#7412=VECTOR('',#26000,6.);
#7413=VECTOR('',#26003,6.);
#7414=VECTOR('',#26006,6.);
#7415=VECTOR('',#26011,4.91825);
#7416=VECTOR('',#26016,4.91825);
#7417=VECTOR('',#26019,4.91825);
#7418=VECTOR('',#26022,4.91825);
#7419=VECTOR('',#26025,4.91825);
#7420=VECTOR('',#26028,4.91825);
#7421=VECTOR('',#26031,4.91825);
#7422=VECTOR('',#26034,4.91825);
#7423=VECTOR('',#26037,4.91825);
#7424=VECTOR('',#26040,4.91825);
#7425=VECTOR('',#26043,5.6435);
#7426=VECTOR('',#26048,5.6435);
#7427=VECTOR('',#26051,5.6435);
#7428=VECTOR('',#26054,5.6435);
#7429=VECTOR('',#26057,5.6435);
#7430=VECTOR('',#26060,5.6435);
#7431=VECTOR('',#26063,5.6435);
#7432=VECTOR('',#26066,5.6435);
#7433=VECTOR('',#26069,5.6435);
#7434=VECTOR('',#26072,5.6435);
#7435=VECTOR('',#26075,5.6435);
#7436=VECTOR('',#26078,5.6435);
#7437=VECTOR('',#26081,5.6435);
#7438=VECTOR('',#26084,5.6435);
#7439=VECTOR('',#26087,5.6435);
#7440=VECTOR('',#26090,5.6435);
#7441=VECTOR('',#26093,5.6435);
#7442=VECTOR('',#26096,5.6435);
#7443=VECTOR('',#26099,5.6435);
#7444=VECTOR('',#26102,5.6435);
#7445=VECTOR('',#26105,5.6435);
#7446=VECTOR('',#26108,5.6435);
#7447=VECTOR('',#26111,5.6435);
#7448=VECTOR('',#26114,5.6435);
#7449=VECTOR('',#26117,5.6435);
#7450=VECTOR('',#26120,5.6435);
#7451=VECTOR('',#26123,5.6435);
#7452=VECTOR('',#26126,5.6435);
#7453=VECTOR('',#26129,5.6435);
#7454=VECTOR('',#26132,5.6435);
#7455=VECTOR('',#26135,5.6435);
#7456=VECTOR('',#26138,5.6435);
#7457=VECTOR('',#26141,5.6435);
#7458=VECTOR('',#26144,5.6435);
#7459=VECTOR('',#26147,5.6435);
#7460=VECTOR('',#26150,5.6435);
#7461=VECTOR('',#26153,5.6435);
#7462=VECTOR('',#26156,5.6435);
#7463=VECTOR('',#26159,5.6435);
#7464=VECTOR('',#26162,5.6435);
#7465=VECTOR('',#26165,5.6435);
#7466=VECTOR('',#26168,5.6435);
#7467=VECTOR('',#26171,5.6435);
#7468=VECTOR('',#26174,5.6435);
#7469=VECTOR('',#26177,5.6435);
#7470=VECTOR('',#26180,5.6435);
#7471=VECTOR('',#26183,5.6435);
#7472=VECTOR('',#26186,5.6435);
#7473=VECTOR('',#26189,5.6435);
#7474=VECTOR('',#26192,5.6435);
#7475=VECTOR('',#26195,5.6435);
#7476=VECTOR('',#26198,5.6435);
#7477=VECTOR('',#26201,5.6435);
#7478=VECTOR('',#26204,5.6435);
#7479=VECTOR('',#26207,5.6435);
#7480=VECTOR('',#26210,5.6435);
#7481=VECTOR('',#26213,5.6435);
#7482=VECTOR('',#26216,5.6435);
#7483=VECTOR('',#26219,5.6435);
#7484=VECTOR('',#26222,5.6435);
#7485=VECTOR('',#26225,5.6435);
#7486=VECTOR('',#26228,5.6435);
#7487=VECTOR('',#26231,5.6435);
#7488=VECTOR('',#26234,5.6435);
#7489=VECTOR('',#26237,5.6435);
#7490=VECTOR('',#26240,5.6435);
#7491=VECTOR('',#26243,5.6435);
#7492=VECTOR('',#26246,5.6435);
#7493=VECTOR('',#26249,5.6435);
#7494=VECTOR('',#26252,5.6435);
#7495=VECTOR('',#26255,5.6435);
#7496=VECTOR('',#26258,5.6435);
#7497=VECTOR('',#26261,5.6435);
#7498=VECTOR('',#26264,5.6435);
#7499=VECTOR('',#26267,5.6435);
#7500=VECTOR('',#26270,5.6435);
#7501=VECTOR('',#26273,5.6435);
#7502=VECTOR('',#26276,5.6435);
#7503=VECTOR('',#26279,5.6435);
#7504=VECTOR('',#26282,5.6435);
#7505=VECTOR('',#26285,5.6435);
#7506=VECTOR('',#26288,5.6435);
#7507=VECTOR('',#26291,5.6435);
#7508=VECTOR('',#26294,5.6435);
#7509=VECTOR('',#26297,5.6435);
#7510=VECTOR('',#26300,5.6435);
#7511=VECTOR('',#26303,5.6435);
#7512=VECTOR('',#26306,5.6435);
#7513=VECTOR('',#26309,5.6435);
#7514=VECTOR('',#26312,5.6435);
#7515=VECTOR('',#26315,5.6435);
#7516=VECTOR('',#26318,5.6435);
#7517=VECTOR('',#26321,5.6435);
#7518=VECTOR('',#26324,5.6435);
#7519=VECTOR('',#26327,5.6435);
#7520=VECTOR('',#26330,5.6435);
#7521=VECTOR('',#26333,5.6435);
#7522=VECTOR('',#26336,5.6435);
#7523=VECTOR('',#26339,5.6435);
#7524=VECTOR('',#26342,5.6435);
#7525=VECTOR('',#26347,4.50000000000001);
#7526=VECTOR('',#26352,5.00000000000001);
#7527=VECTOR('',#26361,4.5);
#7528=VECTOR('',#26366,5.);
#7529=VECTOR('',#26401,10.);
#7530=VECTOR('',#26404,10.);
#7531=VECTOR('',#26405,10.);
#7532=VECTOR('',#26406,10.);
#7533=VECTOR('',#26413,3.00000000000001);
#7534=VECTOR('',#26420,3.00000000000001);
#7535=VECTOR('',#26427,3.);
#7536=VECTOR('',#26434,3.);
#7537=VECTOR('',#26441,3.);
#7538=VECTOR('',#26448,3.);
#7539=VECTOR('',#26455,3.00000000000001);
#7540=VECTOR('',#26462,3.00000000000001);
#7541=VECTOR('',#26469,3.00000000000001);
#7542=VECTOR('',#26476,3.00000000000001);
#7543=VECTOR('',#26483,3.);
#7544=VECTOR('',#26490,3.);
#7545=VECTOR('',#26497,3.);
#7546=VECTOR('',#26504,3.);
#7547=VECTOR('',#26511,3.00000000000001);
#7548=VECTOR('',#26518,3.00000000000001);
#7549=VECTOR('',#26525,8.25000000000001);
#7550=VECTOR('',#26530,10.);
#7551=VECTOR('',#26531,10.);
#7552=VECTOR('',#26534,10.);
#7553=VECTOR('',#26535,10.);
#7554=VECTOR('',#26540,10.);
#7555=VECTOR('',#26543,10.);
#7556=VECTOR('',#26544,10.);
#7557=VECTOR('',#26547,10.);
#7558=VECTOR('',#26548,10.);
#7559=VECTOR('',#26551,10.);
#7560=VECTOR('',#26554,10.);
#7561=VECTOR('',#26555,10.);
#7562=VECTOR('',#26556,10.);
#7563=VECTOR('',#26557,10.);
#7564=VECTOR('',#26560,10.);
#7565=VECTOR('',#26561,10.);
#7566=VECTOR('',#26562,10.);
#7567=VECTOR('',#26565,10.);
#7568=VECTOR('',#26566,10.);
#7569=VECTOR('',#26567,10.);
#7570=VECTOR('',#26570,10.);
#7571=VECTOR('',#26571,10.);
#7572=VECTOR('',#26572,10.);
#7573=VECTOR('',#26575,10.);
#7574=VECTOR('',#26576,10.);
#7575=VECTOR('',#26577,10.);
#7576=VECTOR('',#26580,10.);
#7577=VECTOR('',#26581,10.);
#7578=VECTOR('',#26582,10.);
#7579=VECTOR('',#26585,10.);
#7580=VECTOR('',#26586,10.);
#7581=VECTOR('',#26587,10.);
#7582=VECTOR('',#26590,10.);
#7583=VECTOR('',#26593,10.);
#7584=VECTOR('',#26600,10.);
#7585=VECTOR('',#26601,10.);
#7586=VECTOR('',#26602,10.);
#7587=VECTOR('',#26603,10.);
#7588=VECTOR('',#26608,10.);
#7589=VECTOR('',#26615,10.);
#7590=VECTOR('',#26622,10.);
#7591=VECTOR('',#26627,10.);
#7592=VECTOR('',#26628,10.);
#7593=VECTOR('',#26629,10.);
#7594=VECTOR('',#26634,10.);
#7595=VECTOR('',#26641,10.);
#7596=VECTOR('',#26648,10.);
#7597=VECTOR('',#26653,10.);
#7598=VECTOR('',#26654,10.);
#7599=VECTOR('',#26655,10.);
#7600=VECTOR('',#26660,10.);
#7601=VECTOR('',#26665,10.);
#7602=VECTOR('',#26666,10.);
#7603=VECTOR('',#26667,10.);
#7604=VECTOR('',#26672,10.);
#7605=VECTOR('',#26677,10.);
#7606=VECTOR('',#26678,10.);
#7607=VECTOR('',#26679,10.);
#7608=VECTOR('',#26684,10.);
#7609=VECTOR('',#26689,10.);
#7610=VECTOR('',#26690,10.);
#7611=VECTOR('',#26691,10.);
#7612=VECTOR('',#26694,10.);
#7613=VECTOR('',#26695,10.);
#7614=VECTOR('',#26696,10.);
#7615=VECTOR('',#26699,10.);
#7616=VECTOR('',#26700,10.);
#7617=VECTOR('',#26701,10.);
#7618=VECTOR('',#26702,10.);
#7619=VECTOR('',#26705,10.);
#7620=VECTOR('',#26708,10.);
#7621=VECTOR('',#26711,10.);
#7622=VECTOR('',#26718,10.);
#7623=VECTOR('',#26725,10.);
#7624=VECTOR('',#26728,10.);
#7625=VECTOR('',#26729,10.);
#7626=VECTOR('',#26730,10.);
#7627=VECTOR('',#26733,10.);
#7628=VECTOR('',#26738,10.);
#7629=VECTOR('',#26743,10.);
#7630=VECTOR('',#26748,10.);
#7631=VECTOR('',#26749,10.);
#7632=VECTOR('',#26752,10.);
#7633=VECTOR('',#26757,10.);
#7634=VECTOR('',#26762,10.);
#7635=VECTOR('',#26767,10.);
#7636=VECTOR('',#26768,10.);
#7637=VECTOR('',#26771,10.);
#7638=VECTOR('',#26776,10.);
#7639=VECTOR('',#26777,10.);
#7640=VECTOR('',#26780,10.);
#7641=VECTOR('',#26785,10.);
#7642=VECTOR('',#26786,10.);
#7643=VECTOR('',#26789,10.);
#7644=VECTOR('',#26794,10.);
#7645=VECTOR('',#26795,10.);
#7646=VECTOR('',#26798,10.);
#7647=VECTOR('',#26799,10.);
#7648=VECTOR('',#26802,10.);
#7649=VECTOR('',#26805,10.);
#7650=VECTOR('',#26814,17.5);
#7651=VECTOR('',#26819,10.);
#7652=VECTOR('',#26820,10.);
#7653=VECTOR('',#26821,10.);
#7654=VECTOR('',#26822,10.);
#7655=VECTOR('',#26825,10.);
#7656=VECTOR('',#26826,10.);
#7657=VECTOR('',#26827,10.);
#7658=VECTOR('',#26830,10.);
#7659=VECTOR('',#26831,10.);
#7660=VECTOR('',#26832,10.);
#7661=VECTOR('',#26835,10.);
#7662=VECTOR('',#26836,10.);
#7663=VECTOR('',#26847,20.);
#7664=VECTOR('',#26852,10.);
#7665=VECTOR('',#26853,10.);
#7666=VECTOR('',#26854,10.);
#7667=VECTOR('',#26855,10.);
#7668=VECTOR('',#26858,10.);
#7669=VECTOR('',#26859,10.);
#7670=VECTOR('',#26860,10.);
#7671=VECTOR('',#26863,10.);
#7672=VECTOR('',#26864,10.);
#7673=VECTOR('',#26865,10.);
#7674=VECTOR('',#26868,10.);
#7675=VECTOR('',#26869,10.);
#7676=VECTOR('',#26880,17.5);
#7677=VECTOR('',#26885,10.);
#7678=VECTOR('',#26886,10.);
#7679=VECTOR('',#26887,10.);
#7680=VECTOR('',#26888,10.);
#7681=VECTOR('',#26891,10.);
#7682=VECTOR('',#26892,10.);
#7683=VECTOR('',#26893,10.);
#7684=VECTOR('',#26896,10.);
#7685=VECTOR('',#26897,10.);
#7686=VECTOR('',#26898,10.);
#7687=VECTOR('',#26901,10.);
#7688=VECTOR('',#26902,10.);
#7689=VECTOR('',#26911,10.);
#7690=VECTOR('',#26912,10.);
#7691=VECTOR('',#26913,10.);
#7692=VECTOR('',#26914,10.);
#7693=VECTOR('',#26919,10.);
#7694=VECTOR('',#26926,10.);
#7695=VECTOR('',#26933,10.);
#7696=VECTOR('',#26938,10.);
#7697=VECTOR('',#26939,10.);
#7698=VECTOR('',#26940,10.);
#7699=VECTOR('',#26945,10.);
#7700=VECTOR('',#26952,10.);
#7701=VECTOR('',#26959,10.);
#7702=VECTOR('',#26964,10.);
#7703=VECTOR('',#26965,10.);
#7704=VECTOR('',#26966,10.);
#7705=VECTOR('',#26971,10.);
#7706=VECTOR('',#26976,10.);
#7707=VECTOR('',#26977,10.);
#7708=VECTOR('',#26978,10.);
#7709=VECTOR('',#26983,10.);
#7710=VECTOR('',#26988,10.);
#7711=VECTOR('',#26989,10.);
#7712=VECTOR('',#26990,10.);
#7713=VECTOR('',#26995,10.);
#7714=VECTOR('',#27000,10.);
#7715=VECTOR('',#27001,10.);
#7716=VECTOR('',#27002,10.);
#7717=VECTOR('',#27005,10.);
#7718=VECTOR('',#27006,10.);
#7719=VECTOR('',#27007,10.);
#7720=VECTOR('',#27010,10.);
#7721=VECTOR('',#27011,10.);
#7722=VECTOR('',#27018,10.);
#7723=VECTOR('',#27025,10.);
#7724=VECTOR('',#27028,10.);
#7725=VECTOR('',#27031,10.);
#7726=VECTOR('',#27034,10.);
#7727=VECTOR('',#27035,10.);
#7728=VECTOR('',#27036,10.);
#7729=VECTOR('',#27039,10.);
#7730=VECTOR('',#27040,10.);
#7731=VECTOR('',#27041,10.);
#7732=VECTOR('',#27046,10.);
#7733=VECTOR('',#27051,10.);
#7734=VECTOR('',#27056,10.);
#7735=VECTOR('',#27059,10.);
#7736=VECTOR('',#27060,10.);
#7737=VECTOR('',#27065,10.);
#7738=VECTOR('',#27070,10.);
#7739=VECTOR('',#27075,10.);
#7740=VECTOR('',#27078,10.);
#7741=VECTOR('',#27079,10.);
#7742=VECTOR('',#27084,10.);
#7743=VECTOR('',#27087,10.);
#7744=VECTOR('',#27088,10.);
#7745=VECTOR('',#27093,10.);
#7746=VECTOR('',#27096,10.);
#7747=VECTOR('',#27097,10.);
#7748=VECTOR('',#27102,10.);
#7749=VECTOR('',#27105,10.);
#7750=VECTOR('',#27106,10.);
#7751=VECTOR('',#27109,10.);
#7752=VECTOR('',#27110,10.);
#7753=VECTOR('',#27113,10.);
#7754=VECTOR('',#27116,10.);
#7755=VERTEX_POINT('',#27150);
#7756=VERTEX_POINT('',#27151);
#7757=VERTEX_POINT('',#27153);
#7758=VERTEX_POINT('',#27155);
#7759=VERTEX_POINT('',#27157);
#7760=VERTEX_POINT('',#27159);
#7761=VERTEX_POINT('',#27161);
#7762=VERTEX_POINT('',#27163);
#7763=VERTEX_POINT('',#27165);
#7764=VERTEX_POINT('',#27167);
#7765=VERTEX_POINT('',#27169);
#7766=VERTEX_POINT('',#27171);
#7767=VERTEX_POINT('',#27173);
#7768=VERTEX_POINT('',#27175);
#7769=VERTEX_POINT('',#27177);
#7770=VERTEX_POINT('',#27179);
#7771=VERTEX_POINT('',#27181);
#7772=VERTEX_POINT('',#27183);
#7773=VERTEX_POINT('',#27185);
#7774=VERTEX_POINT('',#27187);
#7775=VERTEX_POINT('',#27189);
#7776=VERTEX_POINT('',#27191);
#7777=VERTEX_POINT('',#27193);
#7778=VERTEX_POINT('',#27195);
#7779=VERTEX_POINT('',#27197);
#7780=VERTEX_POINT('',#27199);
#7781=VERTEX_POINT('',#27201);
#7782=VERTEX_POINT('',#27203);
#7783=VERTEX_POINT('',#27205);
#7784=VERTEX_POINT('',#27207);
#7785=VERTEX_POINT('',#27209);
#7786=VERTEX_POINT('',#27211);
#7787=VERTEX_POINT('',#27213);
#7788=VERTEX_POINT('',#27215);
#7789=VERTEX_POINT('',#27217);
#7790=VERTEX_POINT('',#27219);
#7791=VERTEX_POINT('',#27223);
#7792=VERTEX_POINT('',#27225);
#7793=VERTEX_POINT('',#27229);
#7794=VERTEX_POINT('',#27233);
#7795=VERTEX_POINT('',#27237);
#7796=VERTEX_POINT('',#27241);
#7797=VERTEX_POINT('',#27245);
#7798=VERTEX_POINT('',#27249);
#7799=VERTEX_POINT('',#27253);
#7800=VERTEX_POINT('',#27257);
#7801=VERTEX_POINT('',#27261);
#7802=VERTEX_POINT('',#27265);
#7803=VERTEX_POINT('',#27269);
#7804=VERTEX_POINT('',#27273);
#7805=VERTEX_POINT('',#27277);
#7806=VERTEX_POINT('',#27281);
#7807=VERTEX_POINT('',#27285);
#7808=VERTEX_POINT('',#27289);
#7809=VERTEX_POINT('',#27291);
#7810=VERTEX_POINT('',#27295);
#7811=VERTEX_POINT('',#27299);
#7812=VERTEX_POINT('',#27303);
#7813=VERTEX_POINT('',#27307);
#7814=VERTEX_POINT('',#27311);
#7815=VERTEX_POINT('',#27315);
#7816=VERTEX_POINT('',#27321);
#7817=VERTEX_POINT('',#27325);
#7818=VERTEX_POINT('',#27329);
#7819=VERTEX_POINT('',#27333);
#7820=VERTEX_POINT('',#27337);
#7821=VERTEX_POINT('',#27341);
#7822=VERTEX_POINT('',#27345);
#7823=VERTEX_POINT('',#27349);
#7824=VERTEX_POINT('',#27353);
#7825=VERTEX_POINT('',#27357);
#7826=VERTEX_POINT('',#27361);
#7827=VERTEX_POINT('',#27368);
#7828=VERTEX_POINT('',#27369);
#7829=VERTEX_POINT('',#27371);
#7830=VERTEX_POINT('',#27373);
#7831=VERTEX_POINT('',#27377);
#7832=VERTEX_POINT('',#27379);
#7833=VERTEX_POINT('',#27383);
#7834=VERTEX_POINT('',#27385);
#7835=VERTEX_POINT('',#27389);
#7836=VERTEX_POINT('',#27391);
#7837=VERTEX_POINT('',#27395);
#7838=VERTEX_POINT('',#27397);
#7839=VERTEX_POINT('',#27401);
#7840=VERTEX_POINT('',#27403);
#7841=VERTEX_POINT('',#27407);
#7842=VERTEX_POINT('',#27409);
#7843=VERTEX_POINT('',#27413);
#7844=VERTEX_POINT('',#27414);
#7845=VERTEX_POINT('',#27416);
#7846=VERTEX_POINT('',#27418);
#7847=VERTEX_POINT('',#27420);
#7848=VERTEX_POINT('',#27422);
#7849=VERTEX_POINT('',#27424);
#7850=VERTEX_POINT('',#27426);
#7851=VERTEX_POINT('',#27428);
#7852=VERTEX_POINT('',#27430);
#7853=VERTEX_POINT('',#27433);
#7854=VERTEX_POINT('',#27435);
#7855=VERTEX_POINT('',#27437);
#7856=VERTEX_POINT('',#27439);
#7857=VERTEX_POINT('',#27441);
#7858=VERTEX_POINT('',#27443);
#7859=VERTEX_POINT('',#27445);
#7860=VERTEX_POINT('',#27447);
#7861=VERTEX_POINT('',#27449);
#7862=VERTEX_POINT('',#27451);
#7863=VERTEX_POINT('',#27453);
#7864=VERTEX_POINT('',#27455);
#7865=VERTEX_POINT('',#27457);
#7866=VERTEX_POINT('',#27459);
#7867=VERTEX_POINT('',#27461);
#7868=VERTEX_POINT('',#27463);
#7869=VERTEX_POINT('',#27465);
#7870=VERTEX_POINT('',#27467);
#7871=VERTEX_POINT('',#27469);
#7872=VERTEX_POINT('',#27471);
#7873=VERTEX_POINT('',#27473);
#7874=VERTEX_POINT('',#27475);
#7875=VERTEX_POINT('',#27477);
#7876=VERTEX_POINT('',#27479);
#7877=VERTEX_POINT('',#27481);
#7878=VERTEX_POINT('',#27483);
#7879=VERTEX_POINT('',#27487);
#7880=VERTEX_POINT('',#27489);
#7881=VERTEX_POINT('',#27493);
#7882=VERTEX_POINT('',#27497);
#7883=VERTEX_POINT('',#27501);
#7884=VERTEX_POINT('',#27504);
#7885=VERTEX_POINT('',#27506);
#7886=VERTEX_POINT('',#27509);
#7887=VERTEX_POINT('',#27513);
#7888=VERTEX_POINT('',#27517);
#7889=VERTEX_POINT('',#27519);
#7890=VERTEX_POINT('',#27521);
#7891=VERTEX_POINT('',#27523);
#7892=VERTEX_POINT('',#27525);
#7893=VERTEX_POINT('',#27527);
#7894=VERTEX_POINT('',#27529);
#7895=VERTEX_POINT('',#27531);
#7896=VERTEX_POINT('',#27533);
#7897=VERTEX_POINT('',#27535);
#7898=VERTEX_POINT('',#27537);
#7899=VERTEX_POINT('',#27539);
#7900=VERTEX_POINT('',#27541);
#7901=VERTEX_POINT('',#27543);
#7902=VERTEX_POINT('',#27545);
#7903=VERTEX_POINT('',#27547);
#7904=VERTEX_POINT('',#27549);
#7905=VERTEX_POINT('',#27551);
#7906=VERTEX_POINT('',#27553);
#7907=VERTEX_POINT('',#27555);
#7908=VERTEX_POINT('',#27557);
#7909=VERTEX_POINT('',#27560);
#7910=VERTEX_POINT('',#27562);
#7911=VERTEX_POINT('',#27564);
#7912=VERTEX_POINT('',#27566);
#7913=VERTEX_POINT('',#27568);
#7914=VERTEX_POINT('',#27570);
#7915=VERTEX_POINT('',#27572);
#7916=VERTEX_POINT('',#27574);
#7917=VERTEX_POINT('',#27586);
#7918=VERTEX_POINT('',#27588);
#7919=VERTEX_POINT('',#27592);
#7920=VERTEX_POINT('',#27596);
#7921=VERTEX_POINT('',#27600);
#7922=VERTEX_POINT('',#27604);
#7923=VERTEX_POINT('',#27658);
#7924=VERTEX_POINT('',#27659);
#7925=VERTEX_POINT('',#27661);
#7926=VERTEX_POINT('',#27663);
#7927=VERTEX_POINT('',#27667);
#7928=VERTEX_POINT('',#27669);
#7929=VERTEX_POINT('',#27673);
#7930=VERTEX_POINT('',#27675);
#7931=VERTEX_POINT('',#27679);
#7932=VERTEX_POINT('',#27681);
#7933=VERTEX_POINT('',#27685);
#7934=VERTEX_POINT('',#27687);
#7935=VERTEX_POINT('',#27691);
#7936=VERTEX_POINT('',#27693);
#7937=VERTEX_POINT('',#27697);
#7938=VERTEX_POINT('',#27699);
#7939=VERTEX_POINT('',#27703);
#7940=VERTEX_POINT('',#27705);
#7941=VERTEX_POINT('',#27709);
#7942=VERTEX_POINT('',#27710);
#7943=VERTEX_POINT('',#27712);
#7944=VERTEX_POINT('',#27714);
#7945=VERTEX_POINT('',#27718);
#7946=VERTEX_POINT('',#27720);
#7947=VERTEX_POINT('',#27724);
#7948=VERTEX_POINT('',#27726);
#7949=VERTEX_POINT('',#27730);
#7950=VERTEX_POINT('',#27732);
#7951=VERTEX_POINT('',#27736);
#7952=VERTEX_POINT('',#27738);
#7953=VERTEX_POINT('',#27742);
#7954=VERTEX_POINT('',#27744);
#7955=VERTEX_POINT('',#27748);
#7956=VERTEX_POINT('',#27750);
#7957=VERTEX_POINT('',#27754);
#7958=VERTEX_POINT('',#27756);
#7959=VERTEX_POINT('',#27760);
#7960=VERTEX_POINT('',#27761);
#7961=VERTEX_POINT('',#27763);
#7962=VERTEX_POINT('',#27765);
#7963=VERTEX_POINT('',#27767);
#7964=VERTEX_POINT('',#27769);
#7965=VERTEX_POINT('',#27771);
#7966=VERTEX_POINT('',#27773);
#7967=VERTEX_POINT('',#27775);
#7968=VERTEX_POINT('',#27777);
#7969=VERTEX_POINT('',#27779);
#7970=VERTEX_POINT('',#27781);
#7971=VERTEX_POINT('',#27783);
#7972=VERTEX_POINT('',#27785);
#7973=VERTEX_POINT('',#27787);
#7974=VERTEX_POINT('',#27789);
#7975=VERTEX_POINT('',#27791);
#7976=VERTEX_POINT('',#27793);
#7977=VERTEX_POINT('',#27801);
#7978=VERTEX_POINT('',#27805);
#7979=VERTEX_POINT('',#27809);
#7980=VERTEX_POINT('',#27813);
#7981=VERTEX_POINT('',#27817);
#7982=VERTEX_POINT('',#27821);
#7983=VERTEX_POINT('',#27825);
#7984=VERTEX_POINT('',#27829);
#7985=VERTEX_POINT('',#27833);
#7986=VERTEX_POINT('',#27837);
#7987=VERTEX_POINT('',#27841);
#7988=VERTEX_POINT('',#27845);
#7989=VERTEX_POINT('',#27849);
#7990=VERTEX_POINT('',#27853);
#7991=VERTEX_POINT('',#27857);
#7992=VERTEX_POINT('',#27861);
#7993=VERTEX_POINT('',#27865);
#7994=VERTEX_POINT('',#27869);
#7995=VERTEX_POINT('',#27877);
#7996=VERTEX_POINT('',#27878);
#7997=VERTEX_POINT('',#27880);
#7998=VERTEX_POINT('',#27882);
#7999=VERTEX_POINT('',#27884);
#8000=VERTEX_POINT('',#27886);
#8001=VERTEX_POINT('',#27888);
#8002=VERTEX_POINT('',#27890);
#8003=VERTEX_POINT('',#27892);
#8004=VERTEX_POINT('',#27894);
#8005=VERTEX_POINT('',#27896);
#8006=VERTEX_POINT('',#27898);
#8007=VERTEX_POINT('',#27900);
#8008=VERTEX_POINT('',#27902);
#8009=VERTEX_POINT('',#27904);
#8010=VERTEX_POINT('',#27906);
#8011=VERTEX_POINT('',#27908);
#8012=VERTEX_POINT('',#27910);
#8013=VERTEX_POINT('',#27912);
#8014=VERTEX_POINT('',#27914);
#8015=VERTEX_POINT('',#27916);
#8016=VERTEX_POINT('',#27918);
#8017=VERTEX_POINT('',#27920);
#8018=VERTEX_POINT('',#27922);
#8019=VERTEX_POINT('',#27924);
#8020=VERTEX_POINT('',#27926);
#8021=VERTEX_POINT('',#27928);
#8022=VERTEX_POINT('',#27930);
#8023=VERTEX_POINT('',#27932);
#8024=VERTEX_POINT('',#27934);
#8025=VERTEX_POINT('',#27936);
#8026=VERTEX_POINT('',#27938);
#8027=VERTEX_POINT('',#27940);
#8028=VERTEX_POINT('',#27942);
#8029=VERTEX_POINT('',#27944);
#8030=VERTEX_POINT('',#27946);
#8031=VERTEX_POINT('',#27950);
#8032=VERTEX_POINT('',#27952);
#8033=VERTEX_POINT('',#27956);
#8034=VERTEX_POINT('',#27960);
#8035=VERTEX_POINT('',#27964);
#8036=VERTEX_POINT('',#27968);
#8037=VERTEX_POINT('',#27972);
#8038=VERTEX_POINT('',#27976);
#8039=VERTEX_POINT('',#27980);
#8040=VERTEX_POINT('',#27984);
#8041=VERTEX_POINT('',#27988);
#8042=VERTEX_POINT('',#27992);
#8043=VERTEX_POINT('',#27996);
#8044=VERTEX_POINT('',#28000);
#8045=VERTEX_POINT('',#28004);
#8046=VERTEX_POINT('',#28008);
#8047=VERTEX_POINT('',#28012);
#8048=VERTEX_POINT('',#28016);
#8049=VERTEX_POINT('',#28018);
#8050=VERTEX_POINT('',#28022);
#8051=VERTEX_POINT('',#28026);
#8052=VERTEX_POINT('',#28030);
#8053=VERTEX_POINT('',#28034);
#8054=VERTEX_POINT('',#28038);
#8055=VERTEX_POINT('',#28042);
#8056=VERTEX_POINT('',#28048);
#8057=VERTEX_POINT('',#28052);
#8058=VERTEX_POINT('',#28056);
#8059=VERTEX_POINT('',#28060);
#8060=VERTEX_POINT('',#28064);
#8061=VERTEX_POINT('',#28068);
#8062=VERTEX_POINT('',#28072);
#8063=VERTEX_POINT('',#28076);
#8064=VERTEX_POINT('',#28080);
#8065=VERTEX_POINT('',#28084);
#8066=VERTEX_POINT('',#28088);
#8067=VERTEX_POINT('',#28095);
#8068=VERTEX_POINT('',#28096);
#8069=VERTEX_POINT('',#28098);
#8070=VERTEX_POINT('',#28100);
#8071=VERTEX_POINT('',#28104);
#8072=VERTEX_POINT('',#28106);
#8073=VERTEX_POINT('',#28110);
#8074=VERTEX_POINT('',#28112);
#8075=VERTEX_POINT('',#28116);
#8076=VERTEX_POINT('',#28118);
#8077=VERTEX_POINT('',#28122);
#8078=VERTEX_POINT('',#28124);
#8079=VERTEX_POINT('',#28128);
#8080=VERTEX_POINT('',#28130);
#8081=VERTEX_POINT('',#28134);
#8082=VERTEX_POINT('',#28136);
#8083=VERTEX_POINT('',#28140);
#8084=VERTEX_POINT('',#28141);
#8085=VERTEX_POINT('',#28143);
#8086=VERTEX_POINT('',#28145);
#8087=VERTEX_POINT('',#28147);
#8088=VERTEX_POINT('',#28149);
#8089=VERTEX_POINT('',#28151);
#8090=VERTEX_POINT('',#28153);
#8091=VERTEX_POINT('',#28155);
#8092=VERTEX_POINT('',#28157);
#8093=VERTEX_POINT('',#28159);
#8094=VERTEX_POINT('',#28161);
#8095=VERTEX_POINT('',#28163);
#8096=VERTEX_POINT('',#28165);
#8097=VERTEX_POINT('',#28167);
#8098=VERTEX_POINT('',#28169);
#8099=VERTEX_POINT('',#28171);
#8100=VERTEX_POINT('',#28173);
#8101=VERTEX_POINT('',#28175);
#8102=VERTEX_POINT('',#28177);
#8103=VERTEX_POINT('',#28179);
#8104=VERTEX_POINT('',#28181);
#8105=VERTEX_POINT('',#28183);
#8106=VERTEX_POINT('',#28185);
#8107=VERTEX_POINT('',#28187);
#8108=VERTEX_POINT('',#28189);
#8109=VERTEX_POINT('',#28191);
#8110=VERTEX_POINT('',#28193);
#8111=VERTEX_POINT('',#28196);
#8112=VERTEX_POINT('',#28198);
#8113=VERTEX_POINT('',#28200);
#8114=VERTEX_POINT('',#28202);
#8115=VERTEX_POINT('',#28204);
#8116=VERTEX_POINT('',#28206);
#8117=VERTEX_POINT('',#28208);
#8118=VERTEX_POINT('',#28210);
#8119=VERTEX_POINT('',#28214);
#8120=VERTEX_POINT('',#28216);
#8121=VERTEX_POINT('',#28220);
#8122=VERTEX_POINT('',#28224);
#8123=VERTEX_POINT('',#28228);
#8124=VERTEX_POINT('',#28231);
#8125=VERTEX_POINT('',#28233);
#8126=VERTEX_POINT('',#28236);
#8127=VERTEX_POINT('',#28240);
#8128=VERTEX_POINT('',#28244);
#8129=VERTEX_POINT('',#28246);
#8130=VERTEX_POINT('',#28248);
#8131=VERTEX_POINT('',#28250);
#8132=VERTEX_POINT('',#28252);
#8133=VERTEX_POINT('',#28254);
#8134=VERTEX_POINT('',#28256);
#8135=VERTEX_POINT('',#28258);
#8136=VERTEX_POINT('',#28261);
#8137=VERTEX_POINT('',#28263);
#8138=VERTEX_POINT('',#28265);
#8139=VERTEX_POINT('',#28267);
#8140=VERTEX_POINT('',#28269);
#8141=VERTEX_POINT('',#28271);
#8142=VERTEX_POINT('',#28273);
#8143=VERTEX_POINT('',#28275);
#8144=VERTEX_POINT('',#28277);
#8145=VERTEX_POINT('',#28279);
#8146=VERTEX_POINT('',#28281);
#8147=VERTEX_POINT('',#28283);
#8148=VERTEX_POINT('',#28285);
#8149=VERTEX_POINT('',#28287);
#8150=VERTEX_POINT('',#28289);
#8151=VERTEX_POINT('',#28291);
#8152=VERTEX_POINT('',#28293);
#8153=VERTEX_POINT('',#28295);
#8154=VERTEX_POINT('',#28297);
#8155=VERTEX_POINT('',#28299);
#8156=VERTEX_POINT('',#28301);
#8157=VERTEX_POINT('',#28313);
#8158=VERTEX_POINT('',#28315);
#8159=VERTEX_POINT('',#28319);
#8160=VERTEX_POINT('',#28323);
#8161=VERTEX_POINT('',#28327);
#8162=VERTEX_POINT('',#28331);
#8163=VERTEX_POINT('',#28385);
#8164=VERTEX_POINT('',#28386);
#8165=VERTEX_POINT('',#28388);
#8166=VERTEX_POINT('',#28390);
#8167=VERTEX_POINT('',#28394);
#8168=VERTEX_POINT('',#28396);
#8169=VERTEX_POINT('',#28400);
#8170=VERTEX_POINT('',#28402);
#8171=VERTEX_POINT('',#28406);
#8172=VERTEX_POINT('',#28408);
#8173=VERTEX_POINT('',#28412);
#8174=VERTEX_POINT('',#28414);
#8175=VERTEX_POINT('',#28418);
#8176=VERTEX_POINT('',#28420);
#8177=VERTEX_POINT('',#28424);
#8178=VERTEX_POINT('',#28426);
#8179=VERTEX_POINT('',#28430);
#8180=VERTEX_POINT('',#28432);
#8181=VERTEX_POINT('',#28436);
#8182=VERTEX_POINT('',#28437);
#8183=VERTEX_POINT('',#28439);
#8184=VERTEX_POINT('',#28441);
#8185=VERTEX_POINT('',#28445);
#8186=VERTEX_POINT('',#28447);
#8187=VERTEX_POINT('',#28451);
#8188=VERTEX_POINT('',#28453);
#8189=VERTEX_POINT('',#28457);
#8190=VERTEX_POINT('',#28459);
#8191=VERTEX_POINT('',#28463);
#8192=VERTEX_POINT('',#28465);
#8193=VERTEX_POINT('',#28469);
#8194=VERTEX_POINT('',#28471);
#8195=VERTEX_POINT('',#28475);
#8196=VERTEX_POINT('',#28477);
#8197=VERTEX_POINT('',#28481);
#8198=VERTEX_POINT('',#28483);
#8199=VERTEX_POINT('',#28487);
#8200=VERTEX_POINT('',#28488);
#8201=VERTEX_POINT('',#28492);
#8202=VERTEX_POINT('',#28494);
#8203=VERTEX_POINT('',#28496);
#8204=VERTEX_POINT('',#28498);
#8205=VERTEX_POINT('',#28500);
#8206=VERTEX_POINT('',#28502);
#8207=VERTEX_POINT('',#28504);
#8208=VERTEX_POINT('',#28506);
#8209=VERTEX_POINT('',#28508);
#8210=VERTEX_POINT('',#28510);
#8211=VERTEX_POINT('',#28512);
#8212=VERTEX_POINT('',#28514);
#8213=VERTEX_POINT('',#28516);
#8214=VERTEX_POINT('',#28518);
#8215=VERTEX_POINT('',#28520);
#8216=VERTEX_POINT('',#28522);
#8217=VERTEX_POINT('',#28528);
#8218=VERTEX_POINT('',#28532);
#8219=VERTEX_POINT('',#28536);
#8220=VERTEX_POINT('',#28540);
#8221=VERTEX_POINT('',#28544);
#8222=VERTEX_POINT('',#28548);
#8223=VERTEX_POINT('',#28552);
#8224=VERTEX_POINT('',#28556);
#8225=VERTEX_POINT('',#28560);
#8226=VERTEX_POINT('',#28564);
#8227=VERTEX_POINT('',#28568);
#8228=VERTEX_POINT('',#28572);
#8229=VERTEX_POINT('',#28576);
#8230=VERTEX_POINT('',#28580);
#8231=VERTEX_POINT('',#28584);
#8232=VERTEX_POINT('',#28588);
#8233=VERTEX_POINT('',#28592);
#8234=VERTEX_POINT('',#28596);
#8235=VERTEX_POINT('',#28604);
#8236=VERTEX_POINT('',#28606);
#8237=VERTEX_POINT('',#28610);
#8238=VERTEX_POINT('',#28614);
#8239=VERTEX_POINT('',#28616);
#8240=VERTEX_POINT('',#28620);
#8241=VERTEX_POINT('',#28624);
#8242=VERTEX_POINT('',#28625);
#8243=VERTEX_POINT('',#28627);
#8244=VERTEX_POINT('',#28629);
#8245=VERTEX_POINT('',#28631);
#8246=VERTEX_POINT('',#28633);
#8247=VERTEX_POINT('',#28635);
#8248=VERTEX_POINT('',#28637);
#8249=VERTEX_POINT('',#28639);
#8250=VERTEX_POINT('',#28641);
#8251=VERTEX_POINT('',#28644);
#8252=VERTEX_POINT('',#28646);
#8253=VERTEX_POINT('',#28648);
#8254=VERTEX_POINT('',#28650);
#8255=VERTEX_POINT('',#28652);
#8256=VERTEX_POINT('',#28654);
#8257=VERTEX_POINT('',#28656);
#8258=VERTEX_POINT('',#28660);
#8259=VERTEX_POINT('',#28662);
#8260=VERTEX_POINT('',#28666);
#8261=VERTEX_POINT('',#28670);
#8262=VERTEX_POINT('',#28672);
#8263=VERTEX_POINT('',#28674);
#8264=VERTEX_POINT('',#28676);
#8265=VERTEX_POINT('',#28678);
#8266=VERTEX_POINT('',#28680);
#8267=VERTEX_POINT('',#28682);
#8268=VERTEX_POINT('',#28684);
#8269=VERTEX_POINT('',#28686);
#8270=VERTEX_POINT('',#28688);
#8271=VERTEX_POINT('',#28690);
#8272=VERTEX_POINT('',#28692);
#8273=VERTEX_POINT('',#28694);
#8274=VERTEX_POINT('',#28696);
#8275=VERTEX_POINT('',#28698);
#8276=VERTEX_POINT('',#28700);
#8277=VERTEX_POINT('',#28702);
#8278=VERTEX_POINT('',#28704);
#8279=VERTEX_POINT('',#28706);
#8280=VERTEX_POINT('',#28708);
#8281=VERTEX_POINT('',#28710);
#8282=VERTEX_POINT('',#28712);
#8283=VERTEX_POINT('',#28714);
#8284=VERTEX_POINT('',#28716);
#8285=VERTEX_POINT('',#28718);
#8286=VERTEX_POINT('',#28720);
#8287=VERTEX_POINT('',#28722);
#8288=VERTEX_POINT('',#28724);
#8289=VERTEX_POINT('',#28726);
#8290=VERTEX_POINT('',#28728);
#8291=VERTEX_POINT('',#28730);
#8292=VERTEX_POINT('',#28732);
#8293=VERTEX_POINT('',#28734);
#8294=VERTEX_POINT('',#28738);
#8295=VERTEX_POINT('',#28740);
#8296=VERTEX_POINT('',#28744);
#8297=VERTEX_POINT('',#28745);
#8298=VERTEX_POINT('',#28750);
#8299=VERTEX_POINT('',#28752);
#8300=VERTEX_POINT('',#28756);
#8301=VERTEX_POINT('',#28758);
#8302=VERTEX_POINT('',#28762);
#8303=VERTEX_POINT('',#28764);
#8304=VERTEX_POINT('',#28768);
#8305=VERTEX_POINT('',#28770);
#8306=VERTEX_POINT('',#28774);
#8307=VERTEX_POINT('',#28776);
#8308=VERTEX_POINT('',#28780);
#8309=VERTEX_POINT('',#28781);
#8310=VERTEX_POINT('',#28786);
#8311=VERTEX_POINT('',#28788);
#8312=VERTEX_POINT('',#28792);
#8313=VERTEX_POINT('',#28793);
#8314=VERTEX_POINT('',#28798);
#8315=VERTEX_POINT('',#28800);
#8316=VERTEX_POINT('',#28804);
#8317=VERTEX_POINT('',#28806);
#8318=VERTEX_POINT('',#28810);
#8319=VERTEX_POINT('',#28812);
#8320=VERTEX_POINT('',#28816);
#8321=VERTEX_POINT('',#28818);
#8322=VERTEX_POINT('',#28822);
#8323=VERTEX_POINT('',#28824);
#8324=VERTEX_POINT('',#28828);
#8325=VERTEX_POINT('',#28829);
#8326=VERTEX_POINT('',#28900);
#8327=VERTEX_POINT('',#28901);
#8328=VERTEX_POINT('',#28904);
#8329=VERTEX_POINT('',#28906);
#8330=VERTEX_POINT('',#28910);
#8331=VERTEX_POINT('',#28912);
#8332=VERTEX_POINT('',#28914);
#8333=VERTEX_POINT('',#28918);
#8334=VERTEX_POINT('',#28919);
#8335=VERTEX_POINT('',#28924);
#8336=VERTEX_POINT('',#28928);
#8337=VERTEX_POINT('',#28932);
#8338=VERTEX_POINT('',#28936);
#8339=VERTEX_POINT('',#28938);
#8340=VERTEX_POINT('',#28942);
#8341=VERTEX_POINT('',#28944);
#8342=VERTEX_POINT('',#28954);
#8343=VERTEX_POINT('',#28956);
#8344=VERTEX_POINT('',#28960);
#8345=VERTEX_POINT('',#28962);
#8346=VERTEX_POINT('',#28966);
#8347=VERTEX_POINT('',#28970);
#8348=VERTEX_POINT('',#28974);
#8349=VERTEX_POINT('',#28975);
#8350=VERTEX_POINT('',#28977);
#8351=VERTEX_POINT('',#28984);
#8352=VERTEX_POINT('',#28988);
#8353=VERTEX_POINT('',#28994);
#8354=VERTEX_POINT('',#28995);
#8355=VERTEX_POINT('',#28998);
#8356=VERTEX_POINT('',#28999);
#8357=VERTEX_POINT('',#29002);
#8358=VERTEX_POINT('',#29003);
#8359=VERTEX_POINT('',#29006);
#8360=VERTEX_POINT('',#29007);
#8361=VERTEX_POINT('',#29010);
#8362=VERTEX_POINT('',#29011);
#8363=VERTEX_POINT('',#29014);
#8364=VERTEX_POINT('',#29015);
#8365=VERTEX_POINT('',#29018);
#8366=VERTEX_POINT('',#29019);
#8367=VERTEX_POINT('',#29022);
#8368=VERTEX_POINT('',#29023);
#8369=VERTEX_POINT('',#29026);
#8370=VERTEX_POINT('',#29028);
#8371=VERTEX_POINT('',#29032);
#8372=VERTEX_POINT('',#29034);
#8373=VERTEX_POINT('',#29038);
#8374=VERTEX_POINT('',#29042);
#8375=VERTEX_POINT('',#29044);
#8376=VERTEX_POINT('',#29048);
#8377=VERTEX_POINT('',#29052);
#8378=VERTEX_POINT('',#29053);
#8379=VERTEX_POINT('',#29055);
#8380=VERTEX_POINT('',#29057);
#8381=VERTEX_POINT('',#29059);
#8382=VERTEX_POINT('',#29061);
#8383=VERTEX_POINT('',#29063);
#8384=VERTEX_POINT('',#29065);
#8385=VERTEX_POINT('',#29067);
#8386=VERTEX_POINT('',#29069);
#8387=VERTEX_POINT('',#29072);
#8388=VERTEX_POINT('',#29074);
#8389=VERTEX_POINT('',#29076);
#8390=VERTEX_POINT('',#29078);
#8391=VERTEX_POINT('',#29080);
#8392=VERTEX_POINT('',#29082);
#8393=VERTEX_POINT('',#29084);
#8394=VERTEX_POINT('',#29088);
#8395=VERTEX_POINT('',#29090);
#8396=VERTEX_POINT('',#29096);
#8397=VERTEX_POINT('',#29098);
#8398=VERTEX_POINT('',#29100);
#8399=VERTEX_POINT('',#29102);
#8400=VERTEX_POINT('',#29104);
#8401=VERTEX_POINT('',#29106);
#8402=VERTEX_POINT('',#29108);
#8403=VERTEX_POINT('',#29110);
#8404=VERTEX_POINT('',#29112);
#8405=VERTEX_POINT('',#29114);
#8406=VERTEX_POINT('',#29116);
#8407=VERTEX_POINT('',#29118);
#8408=VERTEX_POINT('',#29120);
#8409=VERTEX_POINT('',#29122);
#8410=VERTEX_POINT('',#29124);
#8411=VERTEX_POINT('',#29126);
#8412=VERTEX_POINT('',#29128);
#8413=VERTEX_POINT('',#29130);
#8414=VERTEX_POINT('',#29132);
#8415=VERTEX_POINT('',#29134);
#8416=VERTEX_POINT('',#29136);
#8417=VERTEX_POINT('',#29138);
#8418=VERTEX_POINT('',#29140);
#8419=VERTEX_POINT('',#29142);
#8420=VERTEX_POINT('',#29144);
#8421=VERTEX_POINT('',#29146);
#8422=VERTEX_POINT('',#29148);
#8423=VERTEX_POINT('',#29150);
#8424=VERTEX_POINT('',#29152);
#8425=VERTEX_POINT('',#29154);
#8426=VERTEX_POINT('',#29156);
#8427=VERTEX_POINT('',#29158);
#8428=VERTEX_POINT('',#29160);
#8429=VERTEX_POINT('',#29164);
#8430=VERTEX_POINT('',#29166);
#8431=VERTEX_POINT('',#29170);
#8432=VERTEX_POINT('',#29171);
#8433=VERTEX_POINT('',#29176);
#8434=VERTEX_POINT('',#29178);
#8435=VERTEX_POINT('',#29182);
#8436=VERTEX_POINT('',#29184);
#8437=VERTEX_POINT('',#29188);
#8438=VERTEX_POINT('',#29190);
#8439=VERTEX_POINT('',#29194);
#8440=VERTEX_POINT('',#29196);
#8441=VERTEX_POINT('',#29200);
#8442=VERTEX_POINT('',#29202);
#8443=VERTEX_POINT('',#29206);
#8444=VERTEX_POINT('',#29207);
#8445=VERTEX_POINT('',#29212);
#8446=VERTEX_POINT('',#29214);
#8447=VERTEX_POINT('',#29218);
#8448=VERTEX_POINT('',#29219);
#8449=VERTEX_POINT('',#29224);
#8450=VERTEX_POINT('',#29226);
#8451=VERTEX_POINT('',#29230);
#8452=VERTEX_POINT('',#29232);
#8453=VERTEX_POINT('',#29236);
#8454=VERTEX_POINT('',#29238);
#8455=VERTEX_POINT('',#29242);
#8456=VERTEX_POINT('',#29244);
#8457=VERTEX_POINT('',#29248);
#8458=VERTEX_POINT('',#29250);
#8459=VERTEX_POINT('',#29254);
#8460=VERTEX_POINT('',#29255);
#8461=VERTEX_POINT('',#29327);
#8462=VERTEX_POINT('',#29328);
#8463=VERTEX_POINT('',#29330);
#8464=VERTEX_POINT('',#29332);
#8465=VERTEX_POINT('',#29336);
#8466=VERTEX_POINT('',#29338);
#8467=VERTEX_POINT('',#29342);
#8468=VERTEX_POINT('',#29344);
#8469=VERTEX_POINT('',#29348);
#8470=VERTEX_POINT('',#29349);
#8471=VERTEX_POINT('',#29351);
#8472=VERTEX_POINT('',#29353);
#8473=VERTEX_POINT('',#29357);
#8474=VERTEX_POINT('',#29359);
#8475=VERTEX_POINT('',#29363);
#8476=VERTEX_POINT('',#29365);
#8477=VERTEX_POINT('',#29369);
#8478=VERTEX_POINT('',#29371);
#8479=VERTEX_POINT('',#29375);
#8480=VERTEX_POINT('',#29377);
#8481=VERTEX_POINT('',#29381);
#8482=VERTEX_POINT('',#29383);
#8483=VERTEX_POINT('',#29387);
#8484=VERTEX_POINT('',#29388);
#8485=VERTEX_POINT('',#29390);
#8486=VERTEX_POINT('',#29392);
#8487=VERTEX_POINT('',#29396);
#8488=VERTEX_POINT('',#29398);
#8489=VERTEX_POINT('',#29402);
#8490=VERTEX_POINT('',#29404);
#8491=VERTEX_POINT('',#29408);
#8492=VERTEX_POINT('',#29410);
#8493=VERTEX_POINT('',#29414);
#8494=VERTEX_POINT('',#29415);
#8495=VERTEX_POINT('',#29417);
#8496=VERTEX_POINT('',#29419);
#8497=VERTEX_POINT('',#29423);
#8498=VERTEX_POINT('',#29425);
#8499=VERTEX_POINT('',#29429);
#8500=VERTEX_POINT('',#29431);
#8501=VERTEX_POINT('',#29435);
#8502=VERTEX_POINT('',#29437);
#8503=VERTEX_POINT('',#29441);
#8504=VERTEX_POINT('',#29443);
#8505=VERTEX_POINT('',#29450);
#8506=VERTEX_POINT('',#29451);
#8507=VERTEX_POINT('',#29453);
#8508=VERTEX_POINT('',#29455);
#8509=VERTEX_POINT('',#29459);
#8510=VERTEX_POINT('',#29461);
#8511=VERTEX_POINT('',#29465);
#8512=VERTEX_POINT('',#29467);
#8513=VERTEX_POINT('',#29474);
#8514=VERTEX_POINT('',#29475);
#8515=VERTEX_POINT('',#29477);
#8516=VERTEX_POINT('',#29479);
#8517=VERTEX_POINT('',#29483);
#8518=VERTEX_POINT('',#29485);
#8519=VERTEX_POINT('',#29489);
#8520=VERTEX_POINT('',#29491);
#8521=VERTEX_POINT('',#29495);
#8522=VERTEX_POINT('',#29497);
#8523=VERTEX_POINT('',#29501);
#8524=VERTEX_POINT('',#29503);
#8525=VERTEX_POINT('',#29507);
#8526=VERTEX_POINT('',#29509);
#8527=VERTEX_POINT('',#29513);
#8528=VERTEX_POINT('',#29514);
#8529=VERTEX_POINT('',#29516);
#8530=VERTEX_POINT('',#29518);
#8531=VERTEX_POINT('',#29522);
#8532=VERTEX_POINT('',#29524);
#8533=VERTEX_POINT('',#29528);
#8534=VERTEX_POINT('',#29530);
#8535=VERTEX_POINT('',#29537);
#8536=VERTEX_POINT('',#29539);
#8537=VERTEX_POINT('',#29543);
#8538=VERTEX_POINT('',#29545);
#8539=VERTEX_POINT('',#29549);
#8540=VERTEX_POINT('',#29550);
#8541=VERTEX_POINT('',#29552);
#8542=VERTEX_POINT('',#29554);
#8543=VERTEX_POINT('',#29558);
#8544=VERTEX_POINT('',#29560);
#8545=VERTEX_POINT('',#29564);
#8546=VERTEX_POINT('',#29566);
#8547=VERTEX_POINT('',#29570);
#8548=VERTEX_POINT('',#29572);
#8549=VERTEX_POINT('',#29576);
#8550=VERTEX_POINT('',#29578);
#8551=VERTEX_POINT('',#29585);
#8552=VERTEX_POINT('',#29586);
#8553=VERTEX_POINT('',#29588);
#8554=VERTEX_POINT('',#29590);
#8555=VERTEX_POINT('',#29594);
#8556=VERTEX_POINT('',#29596);
#8557=VERTEX_POINT('',#29600);
#8558=VERTEX_POINT('',#29602);
#8559=VERTEX_POINT('',#29606);
#8560=VERTEX_POINT('',#29608);
#8561=VERTEX_POINT('',#29612);
#8562=VERTEX_POINT('',#29613);
#8563=VERTEX_POINT('',#29615);
#8564=VERTEX_POINT('',#29617);
#8565=VERTEX_POINT('',#29621);
#8566=VERTEX_POINT('',#29623);
#8567=VERTEX_POINT('',#29627);
#8568=VERTEX_POINT('',#29629);
#8569=VERTEX_POINT('',#29633);
#8570=VERTEX_POINT('',#29635);
#8571=VERTEX_POINT('',#29639);
#8572=VERTEX_POINT('',#29641);
#8573=VERTEX_POINT('',#29645);
#8574=VERTEX_POINT('',#29647);
#8575=VERTEX_POINT('',#29654);
#8576=VERTEX_POINT('',#29656);
#8577=VERTEX_POINT('',#29660);
#8578=VERTEX_POINT('',#29662);
#8579=VERTEX_POINT('',#29666);
#8580=VERTEX_POINT('',#29668);
#8581=VERTEX_POINT('',#29672);
#8582=VERTEX_POINT('',#29674);
#8583=VERTEX_POINT('',#29678);
#8584=VERTEX_POINT('',#29680);
#8585=VERTEX_POINT('',#29684);
#8586=VERTEX_POINT('',#29686);
#8587=VERTEX_POINT('',#29690);
#8588=VERTEX_POINT('',#29692);
#8589=VERTEX_POINT('',#29699);
#8590=VERTEX_POINT('',#29701);
#8591=VERTEX_POINT('',#29705);
#8592=VERTEX_POINT('',#29707);
#8593=VERTEX_POINT('',#29711);
#8594=VERTEX_POINT('',#29713);
#8595=VERTEX_POINT('',#29717);
#8596=VERTEX_POINT('',#29719);
#8597=VERTEX_POINT('',#29723);
#8598=VERTEX_POINT('',#29725);
#8599=VERTEX_POINT('',#29729);
#8600=VERTEX_POINT('',#29731);
#8601=VERTEX_POINT('',#29735);
#8602=VERTEX_POINT('',#29737);
#8603=VERTEX_POINT('',#29741);
#8604=VERTEX_POINT('',#29743);
#8605=VERTEX_POINT('',#29747);
#8606=VERTEX_POINT('',#29749);
#8607=VERTEX_POINT('',#29753);
#8608=VERTEX_POINT('',#29755);
#8609=VERTEX_POINT('',#29759);
#8610=VERTEX_POINT('',#29761);
#8611=VERTEX_POINT('',#29765);
#8612=VERTEX_POINT('',#29767);
#8613=VERTEX_POINT('',#29771);
#8614=VERTEX_POINT('',#29773);
#8615=VERTEX_POINT('',#29777);
#8616=VERTEX_POINT('',#29779);
#8617=VERTEX_POINT('',#29783);
#8618=VERTEX_POINT('',#29785);
#8619=VERTEX_POINT('',#29789);
#8620=VERTEX_POINT('',#29791);
#8621=VERTEX_POINT('',#29795);
#8622=VERTEX_POINT('',#29796);
#8623=VERTEX_POINT('',#29798);
#8624=VERTEX_POINT('',#29800);
#8625=VERTEX_POINT('',#29804);
#8626=VERTEX_POINT('',#29806);
#8627=VERTEX_POINT('',#29810);
#8628=VERTEX_POINT('',#29812);
#8629=VERTEX_POINT('',#29816);
#8630=VERTEX_POINT('',#29818);
#8631=VERTEX_POINT('',#29822);
#8632=VERTEX_POINT('',#29823);
#8633=VERTEX_POINT('',#29825);
#8634=VERTEX_POINT('',#29827);
#8635=VERTEX_POINT('',#29831);
#8636=VERTEX_POINT('',#29833);
#8637=VERTEX_POINT('',#29837);
#8638=VERTEX_POINT('',#29839);
#8639=VERTEX_POINT('',#29843);
#8640=VERTEX_POINT('',#29845);
#8641=VERTEX_POINT('',#29849);
#8642=VERTEX_POINT('',#29851);
#8643=VERTEX_POINT('',#29855);
#8644=VERTEX_POINT('',#29857);
#8645=VERTEX_POINT('',#29864);
#8646=VERTEX_POINT('',#29866);
#8647=VERTEX_POINT('',#29870);
#8648=VERTEX_POINT('',#29872);
#8649=VERTEX_POINT('',#29876);
#8650=VERTEX_POINT('',#29878);
#8651=VERTEX_POINT('',#29882);
#8652=VERTEX_POINT('',#29884);
#8653=VERTEX_POINT('',#29891);
#8654=VERTEX_POINT('',#29893);
#8655=VERTEX_POINT('',#29897);
#8656=VERTEX_POINT('',#29899);
#8657=VERTEX_POINT('',#29903);
#8658=VERTEX_POINT('',#29905);
#8659=VERTEX_POINT('',#29909);
#8660=VERTEX_POINT('',#29911);
#8661=VERTEX_POINT('',#29915);
#8662=VERTEX_POINT('',#29917);
#8663=VERTEX_POINT('',#29924);
#8664=VERTEX_POINT('',#29926);
#8665=VERTEX_POINT('',#29930);
#8666=VERTEX_POINT('',#29932);
#8667=VERTEX_POINT('',#29936);
#8668=VERTEX_POINT('',#29938);
#8669=VERTEX_POINT('',#29942);
#8670=VERTEX_POINT('',#29944);
#8671=VERTEX_POINT('',#29948);
#8672=VERTEX_POINT('',#29950);
#8673=VERTEX_POINT('',#29954);
#8674=VERTEX_POINT('',#29956);
#8675=VERTEX_POINT('',#29960);
#8676=VERTEX_POINT('',#29962);
#8677=VERTEX_POINT('',#29966);
#8678=VERTEX_POINT('',#29968);
#8679=VERTEX_POINT('',#29972);
#8680=VERTEX_POINT('',#29974);
#8681=VERTEX_POINT('',#29978);
#8682=VERTEX_POINT('',#29980);
#8683=VERTEX_POINT('',#29984);
#8684=VERTEX_POINT('',#29986);
#8685=VERTEX_POINT('',#29990);
#8686=VERTEX_POINT('',#29992);
#8687=VERTEX_POINT('',#29996);
#8688=VERTEX_POINT('',#29998);
#8689=VERTEX_POINT('',#30002);
#8690=VERTEX_POINT('',#30004);
#8691=VERTEX_POINT('',#30008);
#8692=VERTEX_POINT('',#30010);
#8693=VERTEX_POINT('',#30017);
#8694=VERTEX_POINT('',#30018);
#8695=VERTEX_POINT('',#30020);
#8696=VERTEX_POINT('',#30022);
#8697=VERTEX_POINT('',#30026);
#8698=VERTEX_POINT('',#30028);
#8699=VERTEX_POINT('',#30032);
#8700=VERTEX_POINT('',#30034);
#8701=VERTEX_POINT('',#30038);
#8702=VERTEX_POINT('',#30039);
#8703=VERTEX_POINT('',#30041);
#8704=VERTEX_POINT('',#30043);
#8705=VERTEX_POINT('',#30047);
#8706=VERTEX_POINT('',#30049);
#8707=VERTEX_POINT('',#30053);
#8708=VERTEX_POINT('',#30055);
#8709=VERTEX_POINT('',#30059);
#8710=VERTEX_POINT('',#30061);
#8711=VERTEX_POINT('',#30065);
#8712=VERTEX_POINT('',#30067);
#8713=VERTEX_POINT('',#30071);
#8714=VERTEX_POINT('',#30073);
#8715=VERTEX_POINT('',#30077);
#8716=VERTEX_POINT('',#30079);
#8717=VERTEX_POINT('',#30083);
#8718=VERTEX_POINT('',#30085);
#8719=VERTEX_POINT('',#30089);
#8720=VERTEX_POINT('',#30091);
#8721=VERTEX_POINT('',#30095);
#8722=VERTEX_POINT('',#30097);
#8723=VERTEX_POINT('',#30101);
#8724=VERTEX_POINT('',#30103);
#8725=VERTEX_POINT('',#30107);
#8726=VERTEX_POINT('',#30109);
#8727=VERTEX_POINT('',#30113);
#8728=VERTEX_POINT('',#30115);
#8729=VERTEX_POINT('',#30119);
#8730=VERTEX_POINT('',#30121);
#8731=VERTEX_POINT('',#30125);
#8732=VERTEX_POINT('',#30127);
#8733=VERTEX_POINT('',#30131);
#8734=VERTEX_POINT('',#30133);
#8735=VERTEX_POINT('',#30137);
#8736=VERTEX_POINT('',#30139);
#8737=VERTEX_POINT('',#30146);
#8738=VERTEX_POINT('',#30147);
#8739=VERTEX_POINT('',#30149);
#8740=VERTEX_POINT('',#30151);
#8741=VERTEX_POINT('',#30155);
#8742=VERTEX_POINT('',#30157);
#8743=VERTEX_POINT('',#30161);
#8744=VERTEX_POINT('',#30163);
#8745=VERTEX_POINT('',#30170);
#8746=VERTEX_POINT('',#30171);
#8747=VERTEX_POINT('',#30173);
#8748=VERTEX_POINT('',#30175);
#8749=VERTEX_POINT('',#30179);
#8750=VERTEX_POINT('',#30181);
#8751=VERTEX_POINT('',#30185);
#8752=VERTEX_POINT('',#30187);
#8753=VERTEX_POINT('',#30191);
#8754=VERTEX_POINT('',#30193);
#8755=VERTEX_POINT('',#30197);
#8756=VERTEX_POINT('',#30199);
#8757=VERTEX_POINT('',#30203);
#8758=VERTEX_POINT('',#30205);
#8759=VERTEX_POINT('',#30209);
#8760=VERTEX_POINT('',#30211);
#8761=VERTEX_POINT('',#30215);
#8762=VERTEX_POINT('',#30217);
#8763=VERTEX_POINT('',#30221);
#8764=VERTEX_POINT('',#30223);
#8765=VERTEX_POINT('',#30227);
#8766=VERTEX_POINT('',#30229);
#8767=VERTEX_POINT('',#30236);
#8768=VERTEX_POINT('',#30238);
#8769=VERTEX_POINT('',#30242);
#8770=VERTEX_POINT('',#30244);
#8771=VERTEX_POINT('',#30248);
#8772=VERTEX_POINT('',#30250);
#8773=VERTEX_POINT('',#30254);
#8774=VERTEX_POINT('',#30256);
#8775=VERTEX_POINT('',#30260);
#8776=VERTEX_POINT('',#30262);
#8777=VERTEX_POINT('',#30266);
#8778=VERTEX_POINT('',#30268);
#8779=VERTEX_POINT('',#30272);
#8780=VERTEX_POINT('',#30274);
#8781=VERTEX_POINT('',#30278);
#8782=VERTEX_POINT('',#30280);
#8783=VERTEX_POINT('',#30287);
#8784=VERTEX_POINT('',#30288);
#8785=VERTEX_POINT('',#30290);
#8786=VERTEX_POINT('',#30292);
#8787=VERTEX_POINT('',#30296);
#8788=VERTEX_POINT('',#30298);
#8789=VERTEX_POINT('',#30302);
#8790=VERTEX_POINT('',#30304);
#8791=VERTEX_POINT('',#30308);
#8792=VERTEX_POINT('',#30309);
#8793=VERTEX_POINT('',#30311);
#8794=VERTEX_POINT('',#30313);
#8795=VERTEX_POINT('',#30317);
#8796=VERTEX_POINT('',#30319);
#8797=VERTEX_POINT('',#30323);
#8798=VERTEX_POINT('',#30325);
#8799=VERTEX_POINT('',#30329);
#8800=VERTEX_POINT('',#30331);
#8801=VERTEX_POINT('',#30335);
#8802=VERTEX_POINT('',#30337);
#8803=VERTEX_POINT('',#30341);
#8804=VERTEX_POINT('',#30343);
#8805=VERTEX_POINT('',#30347);
#8806=VERTEX_POINT('',#30349);
#8807=VERTEX_POINT('',#30353);
#8808=VERTEX_POINT('',#30355);
#8809=VERTEX_POINT('',#30359);
#8810=VERTEX_POINT('',#30361);
#8811=VERTEX_POINT('',#30365);
#8812=VERTEX_POINT('',#30367);
#8813=VERTEX_POINT('',#30371);
#8814=VERTEX_POINT('',#30373);
#8815=VERTEX_POINT('',#30377);
#8816=VERTEX_POINT('',#30379);
#8817=VERTEX_POINT('',#30383);
#8818=VERTEX_POINT('',#30385);
#8819=VERTEX_POINT('',#30389);
#8820=VERTEX_POINT('',#30391);
#8821=VERTEX_POINT('',#30395);
#8822=VERTEX_POINT('',#30397);
#8823=VERTEX_POINT('',#30401);
#8824=VERTEX_POINT('',#30403);
#8825=VERTEX_POINT('',#30407);
#8826=VERTEX_POINT('',#30409);
#8827=VERTEX_POINT('',#30416);
#8828=VERTEX_POINT('',#30417);
#8829=VERTEX_POINT('',#30419);
#8830=VERTEX_POINT('',#30421);
#8831=VERTEX_POINT('',#30425);
#8832=VERTEX_POINT('',#30427);
#8833=VERTEX_POINT('',#30431);
#8834=VERTEX_POINT('',#30433);
#8835=VERTEX_POINT('',#30440);
#8836=VERTEX_POINT('',#30441);
#8837=VERTEX_POINT('',#30443);
#8838=VERTEX_POINT('',#30445);
#8839=VERTEX_POINT('',#30449);
#8840=VERTEX_POINT('',#30451);
#8841=VERTEX_POINT('',#30455);
#8842=VERTEX_POINT('',#30457);
#8843=VERTEX_POINT('',#30461);
#8844=VERTEX_POINT('',#30463);
#8845=VERTEX_POINT('',#30467);
#8846=VERTEX_POINT('',#30469);
#8847=VERTEX_POINT('',#30473);
#8848=VERTEX_POINT('',#30475);
#8849=VERTEX_POINT('',#30479);
#8850=VERTEX_POINT('',#30481);
#8851=VERTEX_POINT('',#30485);
#8852=VERTEX_POINT('',#30487);
#8853=VERTEX_POINT('',#30491);
#8854=VERTEX_POINT('',#30493);
#8855=VERTEX_POINT('',#30497);
#8856=VERTEX_POINT('',#30499);
#8857=VERTEX_POINT('',#30506);
#8858=VERTEX_POINT('',#30508);
#8859=VERTEX_POINT('',#30512);
#8860=VERTEX_POINT('',#30514);
#8861=VERTEX_POINT('',#30518);
#8862=VERTEX_POINT('',#30520);
#8863=VERTEX_POINT('',#30524);
#8864=VERTEX_POINT('',#30526);
#8865=VERTEX_POINT('',#30530);
#8866=VERTEX_POINT('',#30532);
#8867=VERTEX_POINT('',#30536);
#8868=VERTEX_POINT('',#30538);
#8869=VERTEX_POINT('',#30542);
#8870=VERTEX_POINT('',#30544);
#8871=VERTEX_POINT('',#30548);
#8872=VERTEX_POINT('',#30550);
#8873=VERTEX_POINT('',#30557);
#8874=VERTEX_POINT('',#30558);
#8875=VERTEX_POINT('',#30560);
#8876=VERTEX_POINT('',#30562);
#8877=VERTEX_POINT('',#30566);
#8878=VERTEX_POINT('',#30568);
#8879=VERTEX_POINT('',#30572);
#8880=VERTEX_POINT('',#30574);
#8881=VERTEX_POINT('',#30578);
#8882=VERTEX_POINT('',#30580);
#8883=VERTEX_POINT('',#30584);
#8884=VERTEX_POINT('',#30585);
#8885=VERTEX_POINT('',#30587);
#8886=VERTEX_POINT('',#30589);
#8887=VERTEX_POINT('',#30593);
#8888=VERTEX_POINT('',#30595);
#8889=VERTEX_POINT('',#30599);
#8890=VERTEX_POINT('',#30601);
#8891=VERTEX_POINT('',#30605);
#8892=VERTEX_POINT('',#30607);
#8893=VERTEX_POINT('',#30611);
#8894=VERTEX_POINT('',#30613);
#8895=VERTEX_POINT('',#30617);
#8896=VERTEX_POINT('',#30619);
#8897=VERTEX_POINT('',#30626);
#8898=VERTEX_POINT('',#30628);
#8899=VERTEX_POINT('',#30632);
#8900=VERTEX_POINT('',#30634);
#8901=VERTEX_POINT('',#30638);
#8902=VERTEX_POINT('',#30640);
#8903=VERTEX_POINT('',#30644);
#8904=VERTEX_POINT('',#30646);
#8905=VERTEX_POINT('',#30650);
#8906=VERTEX_POINT('',#30652);
#8907=VERTEX_POINT('',#30656);
#8908=VERTEX_POINT('',#30658);
#8909=VERTEX_POINT('',#30662);
#8910=VERTEX_POINT('',#30664);
#8911=VERTEX_POINT('',#30671);
#8912=VERTEX_POINT('',#30673);
#8913=VERTEX_POINT('',#30677);
#8914=VERTEX_POINT('',#30679);
#8915=VERTEX_POINT('',#30683);
#8916=VERTEX_POINT('',#30685);
#8917=VERTEX_POINT('',#30689);
#8918=VERTEX_POINT('',#30691);
#8919=VERTEX_POINT('',#30695);
#8920=VERTEX_POINT('',#30697);
#8921=VERTEX_POINT('',#30701);
#8922=VERTEX_POINT('',#30703);
#8923=VERTEX_POINT('',#30707);
#8924=VERTEX_POINT('',#30709);
#8925=VERTEX_POINT('',#30713);
#8926=VERTEX_POINT('',#30715);
#8927=VERTEX_POINT('',#30719);
#8928=VERTEX_POINT('',#30721);
#8929=VERTEX_POINT('',#30725);
#8930=VERTEX_POINT('',#30727);
#8931=VERTEX_POINT('',#30731);
#8932=VERTEX_POINT('',#30733);
#8933=VERTEX_POINT('',#30737);
#8934=VERTEX_POINT('',#30739);
#8935=VERTEX_POINT('',#30743);
#8936=VERTEX_POINT('',#30745);
#8937=VERTEX_POINT('',#30749);
#8938=VERTEX_POINT('',#30751);
#8939=VERTEX_POINT('',#30755);
#8940=VERTEX_POINT('',#30757);
#8941=VERTEX_POINT('',#30761);
#8942=VERTEX_POINT('',#30763);
#8943=VERTEX_POINT('',#30767);
#8944=VERTEX_POINT('',#30769);
#8945=VERTEX_POINT('',#30771);
#8946=VERTEX_POINT('',#30773);
#8947=VERTEX_POINT('',#30775);
#8948=VERTEX_POINT('',#30777);
#8949=VERTEX_POINT('',#30779);
#8950=VERTEX_POINT('',#30781);
#8951=VERTEX_POINT('',#30783);
#8952=VERTEX_POINT('',#30785);
#8953=VERTEX_POINT('',#30787);
#8954=VERTEX_POINT('',#30789);
#8955=VERTEX_POINT('',#30791);
#8956=VERTEX_POINT('',#30793);
#8957=VERTEX_POINT('',#30795);
#8958=VERTEX_POINT('',#30797);
#8959=VERTEX_POINT('',#30799);
#8960=VERTEX_POINT('',#30801);
#8961=VERTEX_POINT('',#30803);
#8962=VERTEX_POINT('',#30805);
#8963=VERTEX_POINT('',#30807);
#8964=VERTEX_POINT('',#30809);
#8965=VERTEX_POINT('',#30811);
#8966=VERTEX_POINT('',#30814);
#8967=VERTEX_POINT('',#30816);
#8968=VERTEX_POINT('',#30818);
#8969=VERTEX_POINT('',#30820);
#8970=VERTEX_POINT('',#30823);
#8971=VERTEX_POINT('',#30824);
#8972=VERTEX_POINT('',#30826);
#8973=VERTEX_POINT('',#30828);
#8974=VERTEX_POINT('',#30830);
#8975=VERTEX_POINT('',#30832);
#8976=VERTEX_POINT('',#30834);
#8977=VERTEX_POINT('',#30836);
#8978=VERTEX_POINT('',#30839);
#8979=VERTEX_POINT('',#30842);
#8980=VERTEX_POINT('',#30844);
#8981=VERTEX_POINT('',#30848);
#8982=VERTEX_POINT('',#30852);
#8983=VERTEX_POINT('',#30856);
#8984=VERTEX_POINT('',#30860);
#8985=VERTEX_POINT('',#30862);
#8986=VERTEX_POINT('',#30866);
#8987=VERTEX_POINT('',#30870);
#8988=VERTEX_POINT('',#30874);
#8989=VERTEX_POINT('',#30878);
#8990=VERTEX_POINT('',#30882);
#8991=VERTEX_POINT('',#30888);
#8992=VERTEX_POINT('',#30892);
#8993=VERTEX_POINT('',#30896);
#8994=VERTEX_POINT('',#30900);
#8995=VERTEX_POINT('',#30906);
#8996=VERTEX_POINT('',#30910);
#8997=VERTEX_POINT('',#30914);
#8998=VERTEX_POINT('',#30918);
#8999=VERTEX_POINT('',#30922);
#9000=VERTEX_POINT('',#30928);
#9001=VERTEX_POINT('',#30932);
#9002=VERTEX_POINT('',#30936);
#9003=VERTEX_POINT('',#30940);
#9004=VERTEX_POINT('',#30944);
#9005=VERTEX_POINT('',#30948);
#9006=VERTEX_POINT('',#30952);
#9007=VERTEX_POINT('',#30956);
#9008=VERTEX_POINT('',#30960);
#9009=VERTEX_POINT('',#30964);
#9010=VERTEX_POINT('',#30968);
#9011=VERTEX_POINT('',#30972);
#9012=VERTEX_POINT('',#30976);
#9013=VERTEX_POINT('',#30980);
#9014=VERTEX_POINT('',#30984);
#9015=VERTEX_POINT('',#30992);
#9016=VERTEX_POINT('',#30993);
#9017=VERTEX_POINT('',#30995);
#9018=VERTEX_POINT('',#31009);
#9019=VERTEX_POINT('',#31016);
#9020=VERTEX_POINT('',#31017);
#9021=VERTEX_POINT('',#31070);
#9022=VERTEX_POINT('',#31071);
#9023=VERTEX_POINT('',#31127);
#9024=VERTEX_POINT('',#31128);
#9025=VERTEX_POINT('',#31181);
#9026=VERTEX_POINT('',#31182);
#9027=VERTEX_POINT('',#31235);
#9028=VERTEX_POINT('',#31236);
#9029=VERTEX_POINT('',#31289);
#9030=VERTEX_POINT('',#31290);
#9031=VERTEX_POINT('',#31340);
#9032=VERTEX_POINT('',#31341);
#9033=VERTEX_POINT('',#31394);
#9034=VERTEX_POINT('',#31395);
#9035=VERTEX_POINT('',#31448);
#9036=VERTEX_POINT('',#31449);
#9037=VERTEX_POINT('',#31502);
#9038=VERTEX_POINT('',#31503);
#9039=VERTEX_POINT('',#31556);
#9040=VERTEX_POINT('',#31557);
#9041=VERTEX_POINT('',#31610);
#9042=VERTEX_POINT('',#31611);
#9043=VERTEX_POINT('',#31664);
#9044=VERTEX_POINT('',#31665);
#9045=VERTEX_POINT('',#31718);
#9046=VERTEX_POINT('',#31719);
#9047=VERTEX_POINT('',#31772);
#9048=VERTEX_POINT('',#31773);
#9049=VERTEX_POINT('',#31826);
#9050=VERTEX_POINT('',#31827);
#9051=VERTEX_POINT('',#31880);
#9052=VERTEX_POINT('',#31881);
#9053=VERTEX_POINT('',#31937);
#9054=VERTEX_POINT('',#31938);
#9055=VERTEX_POINT('',#31991);
#9056=VERTEX_POINT('',#31992);
#9057=VERTEX_POINT('',#32045);
#9058=VERTEX_POINT('',#32046);
#9059=VERTEX_POINT('',#32099);
#9060=VERTEX_POINT('',#32100);
#9061=VERTEX_POINT('',#32150);
#9062=VERTEX_POINT('',#32151);
#9063=VERTEX_POINT('',#32204);
#9064=VERTEX_POINT('',#32205);
#9065=VERTEX_POINT('',#32258);
#9066=VERTEX_POINT('',#32259);
#9067=VERTEX_POINT('',#32312);
#9068=VERTEX_POINT('',#32313);
#9069=VERTEX_POINT('',#32366);
#9070=VERTEX_POINT('',#32367);
#9071=VERTEX_POINT('',#32420);
#9072=VERTEX_POINT('',#32421);
#9073=VERTEX_POINT('',#32477);
#9074=VERTEX_POINT('',#32478);
#9075=VERTEX_POINT('',#32531);
#9076=VERTEX_POINT('',#32532);
#9077=VERTEX_POINT('',#32585);
#9078=VERTEX_POINT('',#32586);
#9079=VERTEX_POINT('',#32642);
#9080=VERTEX_POINT('',#32643);
#9081=VERTEX_POINT('',#32696);
#9082=VERTEX_POINT('',#32697);
#9083=VERTEX_POINT('',#32750);
#9084=VERTEX_POINT('',#32751);
#9085=VERTEX_POINT('',#32804);
#9086=VERTEX_POINT('',#32805);
#9087=VERTEX_POINT('',#32858);
#9088=VERTEX_POINT('',#32859);
#9089=VERTEX_POINT('',#32912);
#9090=VERTEX_POINT('',#32913);
#9091=VERTEX_POINT('',#32963);
#9092=VERTEX_POINT('',#32964);
#9093=VERTEX_POINT('',#33017);
#9094=VERTEX_POINT('',#33018);
#9095=VERTEX_POINT('',#33071);
#9096=VERTEX_POINT('',#33072);
#9097=VERTEX_POINT('',#33125);
#9098=VERTEX_POINT('',#33126);
#9099=VERTEX_POINT('',#33182);
#9100=VERTEX_POINT('',#33183);
#9101=VERTEX_POINT('',#33236);
#9102=VERTEX_POINT('',#33237);
#9103=VERTEX_POINT('',#33290);
#9104=VERTEX_POINT('',#33291);
#9105=VERTEX_POINT('',#33344);
#9106=VERTEX_POINT('',#33345);
#9107=VERTEX_POINT('',#33398);
#9108=VERTEX_POINT('',#33399);
#9109=VERTEX_POINT('',#33452);
#9110=VERTEX_POINT('',#33453);
#9111=VERTEX_POINT('',#33506);
#9112=VERTEX_POINT('',#33507);
#9113=VERTEX_POINT('',#33560);
#9114=VERTEX_POINT('',#33561);
#9115=VERTEX_POINT('',#33614);
#9116=VERTEX_POINT('',#33615);
#9117=VERTEX_POINT('',#33668);
#9118=VERTEX_POINT('',#33669);
#9119=VERTEX_POINT('',#33722);
#9120=VERTEX_POINT('',#33723);
#9121=VERTEX_POINT('',#33773);
#9122=VERTEX_POINT('',#33774);
#9123=VERTEX_POINT('',#33827);
#9124=VERTEX_POINT('',#33828);
#9125=VERTEX_POINT('',#33881);
#9126=VERTEX_POINT('',#33882);
#9127=VERTEX_POINT('',#33935);
#9128=VERTEX_POINT('',#33936);
#9129=VERTEX_POINT('',#33989);
#9130=VERTEX_POINT('',#33990);
#9131=VERTEX_POINT('',#34043);
#9132=VERTEX_POINT('',#34044);
#9133=VERTEX_POINT('',#34097);
#9134=VERTEX_POINT('',#34098);
#9135=VERTEX_POINT('',#34148);
#9136=VERTEX_POINT('',#34149);
#9137=VERTEX_POINT('',#34202);
#9138=VERTEX_POINT('',#34203);
#9139=VERTEX_POINT('',#34256);
#9140=VERTEX_POINT('',#34257);
#9141=VERTEX_POINT('',#34310);
#9142=VERTEX_POINT('',#34311);
#9143=VERTEX_POINT('',#34361);
#9144=VERTEX_POINT('',#34362);
#9145=VERTEX_POINT('',#34415);
#9146=VERTEX_POINT('',#34416);
#9147=VERTEX_POINT('',#34469);
#9148=VERTEX_POINT('',#34470);
#9149=VERTEX_POINT('',#34523);
#9150=VERTEX_POINT('',#34524);
#9151=VERTEX_POINT('',#34577);
#9152=VERTEX_POINT('',#34578);
#9153=VERTEX_POINT('',#34631);
#9154=VERTEX_POINT('',#34632);
#9155=VERTEX_POINT('',#34688);
#9156=VERTEX_POINT('',#34689);
#9157=VERTEX_POINT('',#34742);
#9158=VERTEX_POINT('',#34743);
#9159=VERTEX_POINT('',#34796);
#9160=VERTEX_POINT('',#34797);
#9161=VERTEX_POINT('',#34850);
#9162=VERTEX_POINT('',#34851);
#9163=VERTEX_POINT('',#34904);
#9164=VERTEX_POINT('',#34905);
#9165=VERTEX_POINT('',#34961);
#9166=VERTEX_POINT('',#34962);
#9167=VERTEX_POINT('',#35015);
#9168=VERTEX_POINT('',#35016);
#9169=VERTEX_POINT('',#35072);
#9170=VERTEX_POINT('',#35073);
#9171=VERTEX_POINT('',#35126);
#9172=VERTEX_POINT('',#35127);
#9173=VERTEX_POINT('',#35177);
#9174=VERTEX_POINT('',#35178);
#9175=VERTEX_POINT('',#35231);
#9176=VERTEX_POINT('',#35232);
#9177=VERTEX_POINT('',#35285);
#9178=VERTEX_POINT('',#35286);
#9179=VERTEX_POINT('',#35339);
#9180=VERTEX_POINT('',#35340);
#9181=VERTEX_POINT('',#35393);
#9182=VERTEX_POINT('',#35394);
#9183=VERTEX_POINT('',#35447);
#9184=VERTEX_POINT('',#35448);
#9185=VERTEX_POINT('',#35504);
#9186=VERTEX_POINT('',#35505);
#9187=VERTEX_POINT('',#35558);
#9188=VERTEX_POINT('',#35559);
#9189=VERTEX_POINT('',#35612);
#9190=VERTEX_POINT('',#35613);
#9191=VERTEX_POINT('',#35666);
#9192=VERTEX_POINT('',#35667);
#9193=VERTEX_POINT('',#35720);
#9194=VERTEX_POINT('',#35721);
#9195=VERTEX_POINT('',#35774);
#9196=VERTEX_POINT('',#35775);
#9197=VERTEX_POINT('',#35828);
#9198=VERTEX_POINT('',#35829);
#9199=VERTEX_POINT('',#35882);
#9200=VERTEX_POINT('',#35883);
#9201=VERTEX_POINT('',#35936);
#9202=VERTEX_POINT('',#35937);
#9203=VERTEX_POINT('',#35987);
#9204=VERTEX_POINT('',#35988);
#9205=VERTEX_POINT('',#36041);
#9206=VERTEX_POINT('',#36042);
#9207=VERTEX_POINT('',#36095);
#9208=VERTEX_POINT('',#36096);
#9209=VERTEX_POINT('',#36149);
#9210=VERTEX_POINT('',#36150);
#9211=VERTEX_POINT('',#36203);
#9212=VERTEX_POINT('',#36204);
#9213=VERTEX_POINT('',#36260);
#9214=VERTEX_POINT('',#36261);
#9215=VERTEX_POINT('',#36314);
#9216=VERTEX_POINT('',#36315);
#9217=VERTEX_POINT('',#36368);
#9218=VERTEX_POINT('',#36369);
#9219=VERTEX_POINT('',#36371);
#9220=VERTEX_POINT('',#36421);
#9221=VERTEX_POINT('',#36422);
#9222=VERTEX_POINT('',#36424);
#9223=VERTEX_POINT('',#36442);
#9224=VERTEX_POINT('',#36445);
#9225=VERTEX_POINT('',#36451);
#9226=VERTEX_POINT('',#36467);
#9227=VERTEX_POINT('',#36468);
#9228=VERTEX_POINT('',#36530);
#9229=VERTEX_POINT('',#36531);
#9230=VERTEX_POINT('',#36591);
#9231=VERTEX_POINT('',#36592);
#9232=VERTEX_POINT('',#36655);
#9233=VERTEX_POINT('',#36656);
#9234=VERTEX_POINT('',#36719);
#9235=VERTEX_POINT('',#36720);
#9236=VERTEX_POINT('',#36782);
#9237=VERTEX_POINT('',#36783);
#9238=VERTEX_POINT('',#36843);
#9239=VERTEX_POINT('',#36844);
#9240=VERTEX_POINT('',#36907);
#9241=VERTEX_POINT('',#36908);
#9242=VERTEX_POINT('',#36970);
#9243=VERTEX_POINT('',#36971);
#9244=VERTEX_POINT('',#36973);
#9245=VERTEX_POINT('',#37031);
#9246=VERTEX_POINT('',#37032);
#9247=VERTEX_POINT('',#37034);
#9248=VERTEX_POINT('',#37047);
#9249=VERTEX_POINT('',#37059);
#9250=VERTEX_POINT('',#37060);
#9251=VERTEX_POINT('',#37096);
#9252=VERTEX_POINT('',#37097);
#9253=VERTEX_POINT('',#37134);
#9254=VERTEX_POINT('',#37135);
#9255=VERTEX_POINT('',#37172);
#9256=VERTEX_POINT('',#37173);
#9257=VERTEX_POINT('',#37208);
#9258=VERTEX_POINT('',#37209);
#9259=VERTEX_POINT('',#37246);
#9260=VERTEX_POINT('',#37247);
#9261=VERTEX_POINT('',#37284);
#9262=VERTEX_POINT('',#37285);
#9263=VERTEX_POINT('',#37322);
#9264=VERTEX_POINT('',#37323);
#9265=VERTEX_POINT('',#37358);
#9266=VERTEX_POINT('',#37359);
#9267=VERTEX_POINT('',#37396);
#9268=VERTEX_POINT('',#37397);
#9269=VERTEX_POINT('',#37399);
#9270=VERTEX_POINT('',#37409);
#9271=VERTEX_POINT('',#37419);
#9272=VERTEX_POINT('',#37420);
#9273=VERTEX_POINT('',#37445);
#9274=VERTEX_POINT('',#37446);
#9275=VERTEX_POINT('',#37482);
#9276=VERTEX_POINT('',#37483);
#9277=VERTEX_POINT('',#37525);
#9278=VERTEX_POINT('',#37526);
#9279=VERTEX_POINT('',#37579);
#9280=VERTEX_POINT('',#37580);
#9281=VERTEX_POINT('',#37630);
#9282=VERTEX_POINT('',#37631);
#9283=VERTEX_POINT('',#37656);
#9284=VERTEX_POINT('',#37657);
#9285=VERTEX_POINT('',#37684);
#9286=VERTEX_POINT('',#37685);
#9287=VERTEX_POINT('',#37721);
#9288=VERTEX_POINT('',#37722);
#9289=VERTEX_POINT('',#37775);
#9290=VERTEX_POINT('',#37776);
#9291=VERTEX_POINT('',#37815);
#9292=VERTEX_POINT('',#37816);
#9293=VERTEX_POINT('',#37843);
#9294=VERTEX_POINT('',#37844);
#9295=VERTEX_POINT('',#37880);
#9296=VERTEX_POINT('',#37881);
#9297=VERTEX_POINT('',#37920);
#9298=VERTEX_POINT('',#37921);
#9299=VERTEX_POINT('',#37977);
#9300=VERTEX_POINT('',#37978);
#9301=VERTEX_POINT('',#38031);
#9302=VERTEX_POINT('',#38032);
#9303=VERTEX_POINT('',#38071);
#9304=VERTEX_POINT('',#38072);
#9305=VERTEX_POINT('',#38097);
#9306=VERTEX_POINT('',#38098);
#9307=VERTEX_POINT('',#38124);
#9308=VERTEX_POINT('',#38125);
#9309=VERTEX_POINT('',#38164);
#9310=VERTEX_POINT('',#38165);
#9311=VERTEX_POINT('',#38218);
#9312=VERTEX_POINT('',#38219);
#9313=VERTEX_POINT('',#38262);
#9314=VERTEX_POINT('',#38263);
#9315=VERTEX_POINT('',#38288);
#9316=VERTEX_POINT('',#38289);
#9317=VERTEX_POINT('',#38314);
#9318=VERTEX_POINT('',#38315);
#9319=VERTEX_POINT('',#38339);
#9320=VERTEX_POINT('',#38340);
#9321=VERTEX_POINT('',#38367);
#9322=VERTEX_POINT('',#38368);
#9323=VERTEX_POINT('',#38393);
#9324=VERTEX_POINT('',#38394);
#9325=VERTEX_POINT('',#38419);
#9326=VERTEX_POINT('',#38420);
#9327=VERTEX_POINT('',#38446);
#9328=VERTEX_POINT('',#38447);
#9329=VERTEX_POINT('',#38472);
#9330=VERTEX_POINT('',#38473);
#9331=VERTEX_POINT('',#38509);
#9332=VERTEX_POINT('',#38510);
#9333=VERTEX_POINT('',#38549);
#9334=VERTEX_POINT('',#38550);
#9335=VERTEX_POINT('',#38593);
#9336=VERTEX_POINT('',#38594);
#9337=VERTEX_POINT('',#38618);
#9338=VERTEX_POINT('',#38619);
#9339=VERTEX_POINT('',#38644);
#9340=VERTEX_POINT('',#38645);
#9341=VERTEX_POINT('',#38672);
#9342=VERTEX_POINT('',#38673);
#9343=VERTEX_POINT('',#38698);
#9344=VERTEX_POINT('',#38699);
#9345=VERTEX_POINT('',#38735);
#9346=VERTEX_POINT('',#38736);
#9347=VERTEX_POINT('',#38760);
#9348=VERTEX_POINT('',#38761);
#9349=VERTEX_POINT('',#38788);
#9350=VERTEX_POINT('',#38789);
#9351=VERTEX_POINT('',#38814);
#9352=VERTEX_POINT('',#38815);
#9353=VERTEX_POINT('',#38840);
#9354=VERTEX_POINT('',#38841);
#9355=VERTEX_POINT('',#38868);
#9356=VERTEX_POINT('',#38869);
#9357=VERTEX_POINT('',#38893);
#9358=VERTEX_POINT('',#38894);
#9359=VERTEX_POINT('',#38930);
#9360=VERTEX_POINT('',#38931);
#9361=VERTEX_POINT('',#38956);
#9362=VERTEX_POINT('',#38957);
#9363=VERTEX_POINT('',#38984);
#9364=VERTEX_POINT('',#38985);
#9365=VERTEX_POINT('',#39010);
#9366=VERTEX_POINT('',#39011);
#9367=VERTEX_POINT('',#39035);
#9368=VERTEX_POINT('',#39036);
#9369=VERTEX_POINT('',#39063);
#9370=VERTEX_POINT('',#39064);
#9371=VERTEX_POINT('',#39088);
#9372=VERTEX_POINT('',#39089);
#9373=VERTEX_POINT('',#39125);
#9374=VERTEX_POINT('',#39126);
#9375=VERTEX_POINT('',#39151);
#9376=VERTEX_POINT('',#39152);
#9377=VERTEX_POINT('',#39179);
#9378=VERTEX_POINT('',#39180);
#9379=VERTEX_POINT('',#39205);
#9380=VERTEX_POINT('',#39206);
#9381=VERTEX_POINT('',#39230);
#9382=VERTEX_POINT('',#39231);
#9383=VERTEX_POINT('',#39258);
#9384=VERTEX_POINT('',#39259);
#9385=VERTEX_POINT('',#39284);
#9386=VERTEX_POINT('',#39285);
#9387=VERTEX_POINT('',#39321);
#9388=VERTEX_POINT('',#39322);
#9389=VERTEX_POINT('',#39347);
#9390=VERTEX_POINT('',#39348);
#9391=VERTEX_POINT('',#39374);
#9392=VERTEX_POINT('',#39375);
#9393=VERTEX_POINT('',#39400);
#9394=VERTEX_POINT('',#39401);
#9395=VERTEX_POINT('',#39426);
#9396=VERTEX_POINT('',#39427);
#9397=VERTEX_POINT('',#39454);
#9398=VERTEX_POINT('',#39455);
#9399=VERTEX_POINT('',#39479);
#9400=VERTEX_POINT('',#39480);
#9401=VERTEX_POINT('',#39505);
#9402=VERTEX_POINT('',#39506);
#9403=VERTEX_POINT('',#39531);
#9404=VERTEX_POINT('',#39532);
#9405=VERTEX_POINT('',#39559);
#9406=VERTEX_POINT('',#39560);
#9407=VERTEX_POINT('',#39585);
#9408=VERTEX_POINT('',#39586);
#9409=VERTEX_POINT('',#39611);
#9410=VERTEX_POINT('',#39612);
#9411=VERTEX_POINT('',#39638);
#9412=VERTEX_POINT('',#39639);
#9413=VERTEX_POINT('',#39664);
#9414=VERTEX_POINT('',#39665);
#9415=VERTEX_POINT('',#39690);
#9416=VERTEX_POINT('',#39691);
#9417=VERTEX_POINT('',#39716);
#9418=VERTEX_POINT('',#39717);
#9419=VERTEX_POINT('',#39743);
#9420=VERTEX_POINT('',#39744);
#9421=VERTEX_POINT('',#39769);
#9422=VERTEX_POINT('',#39770);
#9423=VERTEX_POINT('',#39806);
#9424=VERTEX_POINT('',#39807);
#9425=VERTEX_POINT('',#39834);
#9426=VERTEX_POINT('',#39835);
#9427=VERTEX_POINT('',#39860);
#9428=VERTEX_POINT('',#39861);
#9429=VERTEX_POINT('',#39886);
#9430=VERTEX_POINT('',#39887);
#9431=VERTEX_POINT('',#39911);
#9432=VERTEX_POINT('',#39912);
#9433=VERTEX_POINT('',#39939);
#9434=VERTEX_POINT('',#39940);
#9435=VERTEX_POINT('',#39965);
#9436=VERTEX_POINT('',#39966);
#9437=VERTEX_POINT('',#40002);
#9438=VERTEX_POINT('',#40003);
#9439=VERTEX_POINT('',#40029);
#9440=VERTEX_POINT('',#40030);
#9441=VERTEX_POINT('',#40055);
#9442=VERTEX_POINT('',#40056);
#9443=VERTEX_POINT('',#40092);
#9444=VERTEX_POINT('',#40093);
#9445=VERTEX_POINT('',#40118);
#9446=VERTEX_POINT('',#40119);
#9447=VERTEX_POINT('',#40146);
#9448=VERTEX_POINT('',#40147);
#9449=VERTEX_POINT('',#40171);
#9450=VERTEX_POINT('',#40172);
#9451=VERTEX_POINT('',#40197);
#9452=VERTEX_POINT('',#40198);
#9453=VERTEX_POINT('',#40225);
#9454=VERTEX_POINT('',#40226);
#9455=VERTEX_POINT('',#40251);
#9456=VERTEX_POINT('',#40252);
#9457=VERTEX_POINT('',#40288);
#9458=VERTEX_POINT('',#40289);
#9459=VERTEX_POINT('',#40313);
#9460=VERTEX_POINT('',#40314);
#9461=VERTEX_POINT('',#40341);
#9462=VERTEX_POINT('',#40342);
#9463=VERTEX_POINT('',#40367);
#9464=VERTEX_POINT('',#40368);
#9465=VERTEX_POINT('',#40393);
#9466=VERTEX_POINT('',#40394);
#9467=VERTEX_POINT('',#40420);
#9468=VERTEX_POINT('',#40421);
#9469=VERTEX_POINT('',#40446);
#9470=VERTEX_POINT('',#40448);
#9471=VERTEX_POINT('',#40452);
#9472=VERTEX_POINT('',#40457);
#9473=VERTEX_POINT('',#40459);
#9474=VERTEX_POINT('',#40463);
#9475=VERTEX_POINT('',#40468);
#9476=VERTEX_POINT('',#43480);
#9477=VERTEX_POINT('',#43551);
#9478=VERTEX_POINT('',#43575);
#9479=VERTEX_POINT('',#44095);
#9480=VERTEX_POINT('',#44133);
#9481=VERTEX_POINT('',#47629);
#9482=VERTEX_POINT('',#47630);
#9483=VERTEX_POINT('',#47632);
#9484=VERTEX_POINT('',#47634);
#9485=VERTEX_POINT('',#47636);
#9486=VERTEX_POINT('',#47638);
#9487=VERTEX_POINT('',#47641);
#9488=VERTEX_POINT('',#47644);
#9489=VERTEX_POINT('',#47646);
#9490=VERTEX_POINT('',#47650);
#9491=VERTEX_POINT('',#47652);
#9492=VERTEX_POINT('',#47656);
#9493=VERTEX_POINT('',#47658);
#9494=VERTEX_POINT('',#47662);
#9495=VERTEX_POINT('',#47664);
#9496=VERTEX_POINT('',#47668);
#9497=VERTEX_POINT('',#47670);
#9498=VERTEX_POINT('',#47674);
#9499=VERTEX_POINT('',#47676);
#9500=VERTEX_POINT('',#47680);
#9501=VERTEX_POINT('',#47682);
#9502=VERTEX_POINT('',#47686);
#9503=VERTEX_POINT('',#47688);
#9504=VERTEX_POINT('',#47692);
#9505=VERTEX_POINT('',#47694);
#9506=VERTEX_POINT('',#47698);
#9507=VERTEX_POINT('',#47700);
#9508=VERTEX_POINT('',#47704);
#9509=VERTEX_POINT('',#47706);
#9510=VERTEX_POINT('',#47710);
#9511=VERTEX_POINT('',#47712);
#9512=VERTEX_POINT('',#47716);
#9513=VERTEX_POINT('',#47718);
#9514=VERTEX_POINT('',#47722);
#9515=VERTEX_POINT('',#47724);
#9516=VERTEX_POINT('',#47728);
#9517=VERTEX_POINT('',#47730);
#9518=VERTEX_POINT('',#47734);
#9519=VERTEX_POINT('',#47736);
#9520=VERTEX_POINT('',#47740);
#9521=VERTEX_POINT('',#47744);
#9522=VERTEX_POINT('',#47745);
#9523=VERTEX_POINT('',#47750);
#9524=VERTEX_POINT('',#47754);
#9525=VERTEX_POINT('',#47758);
#9526=VERTEX_POINT('',#47762);
#9527=VERTEX_POINT('',#47768);
#9528=VERTEX_POINT('',#47769);
#9529=VERTEX_POINT('',#47771);
#9530=VERTEX_POINT('',#47773);
#9531=VERTEX_POINT('',#47777);
#9532=VERTEX_POINT('',#47779);
#9533=VERTEX_POINT('',#47783);
#9534=VERTEX_POINT('',#47785);
#9535=VERTEX_POINT('',#47789);
#9536=VERTEX_POINT('',#47791);
#9537=VERTEX_POINT('',#47795);
#9538=VERTEX_POINT('',#47797);
#9539=VERTEX_POINT('',#47801);
#9540=VERTEX_POINT('',#47803);
#9541=VERTEX_POINT('',#47807);
#9542=VERTEX_POINT('',#47809);
#9543=VERTEX_POINT('',#47819);
#9544=VERTEX_POINT('',#47820);
#9545=VERTEX_POINT('',#47822);
#9546=VERTEX_POINT('',#47824);
#9547=VERTEX_POINT('',#47828);
#9548=VERTEX_POINT('',#47830);
#9549=VERTEX_POINT('',#47834);
#9550=VERTEX_POINT('',#47836);
#9551=VERTEX_POINT('',#47840);
#9552=VERTEX_POINT('',#47842);
#9553=VERTEX_POINT('',#47846);
#9554=VERTEX_POINT('',#47848);
#9555=VERTEX_POINT('',#47852);
#9556=VERTEX_POINT('',#47854);
#9557=VERTEX_POINT('',#47858);
#9558=VERTEX_POINT('',#47860);
#9559=VERTEX_POINT('',#47864);
#9560=VERTEX_POINT('',#47866);
#9561=VERTEX_POINT('',#47870);
#9562=VERTEX_POINT('',#47872);
#9563=VERTEX_POINT('',#47876);
#9564=VERTEX_POINT('',#47878);
#9565=VERTEX_POINT('',#47882);
#9566=VERTEX_POINT('',#47884);
#9567=VERTEX_POINT('',#47888);
#9568=VERTEX_POINT('',#47890);
#9569=VERTEX_POINT('',#47894);
#9570=VERTEX_POINT('',#47896);
#9571=VERTEX_POINT('',#47900);
#9572=VERTEX_POINT('',#47902);
#9573=VERTEX_POINT('',#47906);
#9574=VERTEX_POINT('',#47908);
#9575=VERTEX_POINT('',#47912);
#9576=VERTEX_POINT('',#47914);
#9577=VERTEX_POINT('',#47918);
#9578=VERTEX_POINT('',#47920);
#9579=VERTEX_POINT('',#47922);
#9580=VERTEX_POINT('',#47924);
#9581=VERTEX_POINT('',#47926);
#9582=VERTEX_POINT('',#47928);
#9583=VERTEX_POINT('',#47930);
#9584=VERTEX_POINT('',#47932);
#9585=VERTEX_POINT('',#47934);
#9586=VERTEX_POINT('',#47936);
#9587=VERTEX_POINT('',#47938);
#9588=VERTEX_POINT('',#47940);
#9589=VERTEX_POINT('',#47942);
#9590=VERTEX_POINT('',#47944);
#9591=VERTEX_POINT('',#47946);
#9592=VERTEX_POINT('',#47948);
#9593=VERTEX_POINT('',#47950);
#9594=VERTEX_POINT('',#47954);
#9595=VERTEX_POINT('',#47956);
#9596=VERTEX_POINT('',#47960);
#9597=VERTEX_POINT('',#47964);
#9598=VERTEX_POINT('',#47968);
#9599=VERTEX_POINT('',#47972);
#9600=VERTEX_POINT('',#47976);
#9601=VERTEX_POINT('',#47980);
#9602=VERTEX_POINT('',#47984);
#9603=VERTEX_POINT('',#47988);
#9604=VERTEX_POINT('',#47992);
#9605=VERTEX_POINT('',#47996);
#9606=VERTEX_POINT('',#48000);
#9607=VERTEX_POINT('',#48004);
#9608=VERTEX_POINT('',#48008);
#9609=VERTEX_POINT('',#48012);
#9610=VERTEX_POINT('',#48016);
#9611=VERTEX_POINT('',#48026);
#9612=VERTEX_POINT('',#48028);
#9613=VERTEX_POINT('',#48032);
#9614=VERTEX_POINT('',#48033);
#9615=VERTEX_POINT('',#48035);
#9616=VERTEX_POINT('',#48037);
#9617=VERTEX_POINT('',#48041);
#9618=VERTEX_POINT('',#48043);
#9619=VERTEX_POINT('',#48047);
#9620=VERTEX_POINT('',#48049);
#9621=VERTEX_POINT('',#48059);
#9622=VERTEX_POINT('',#48061);
#9623=VERTEX_POINT('',#48065);
#9624=VERTEX_POINT('',#48066);
#9625=VERTEX_POINT('',#48068);
#9626=VERTEX_POINT('',#48070);
#9627=VERTEX_POINT('',#48074);
#9628=VERTEX_POINT('',#48076);
#9629=VERTEX_POINT('',#48080);
#9630=VERTEX_POINT('',#48082);
#9631=VERTEX_POINT('',#48092);
#9632=VERTEX_POINT('',#48094);
#9633=VERTEX_POINT('',#48098);
#9634=VERTEX_POINT('',#48099);
#9635=VERTEX_POINT('',#48101);
#9636=VERTEX_POINT('',#48103);
#9637=VERTEX_POINT('',#48107);
#9638=VERTEX_POINT('',#48109);
#9639=VERTEX_POINT('',#48113);
#9640=VERTEX_POINT('',#48115);
#9641=VERTEX_POINT('',#48125);
#9642=VERTEX_POINT('',#48126);
#9643=VERTEX_POINT('',#48128);
#9644=VERTEX_POINT('',#48130);
#9645=VERTEX_POINT('',#48134);
#9646=VERTEX_POINT('',#48136);
#9647=VERTEX_POINT('',#48140);
#9648=VERTEX_POINT('',#48142);
#9649=VERTEX_POINT('',#48146);
#9650=VERTEX_POINT('',#48148);
#9651=VERTEX_POINT('',#48152);
#9652=VERTEX_POINT('',#48154);
#9653=VERTEX_POINT('',#48158);
#9654=VERTEX_POINT('',#48160);
#9655=VERTEX_POINT('',#48164);
#9656=VERTEX_POINT('',#48166);
#9657=VERTEX_POINT('',#48170);
#9658=VERTEX_POINT('',#48172);
#9659=VERTEX_POINT('',#48176);
#9660=VERTEX_POINT('',#48178);
#9661=VERTEX_POINT('',#48182);
#9662=VERTEX_POINT('',#48184);
#9663=VERTEX_POINT('',#48188);
#9664=VERTEX_POINT('',#48190);
#9665=VERTEX_POINT('',#48194);
#9666=VERTEX_POINT('',#48196);
#9667=VERTEX_POINT('',#48200);
#9668=VERTEX_POINT('',#48202);
#9669=VERTEX_POINT('',#48206);
#9670=VERTEX_POINT('',#48208);
#9671=VERTEX_POINT('',#48212);
#9672=VERTEX_POINT('',#48214);
#9673=VERTEX_POINT('',#48218);
#9674=VERTEX_POINT('',#48220);
#9675=VERTEX_POINT('',#48224);
#9676=VERTEX_POINT('',#48226);
#9677=VERTEX_POINT('',#48228);
#9678=VERTEX_POINT('',#48230);
#9679=VERTEX_POINT('',#48232);
#9680=VERTEX_POINT('',#48234);
#9681=VERTEX_POINT('',#48236);
#9682=VERTEX_POINT('',#48238);
#9683=VERTEX_POINT('',#48240);
#9684=VERTEX_POINT('',#48242);
#9685=VERTEX_POINT('',#48244);
#9686=VERTEX_POINT('',#48246);
#9687=VERTEX_POINT('',#48248);
#9688=VERTEX_POINT('',#48250);
#9689=VERTEX_POINT('',#48252);
#9690=VERTEX_POINT('',#48254);
#9691=VERTEX_POINT('',#48256);
#9692=VERTEX_POINT('',#48260);
#9693=VERTEX_POINT('',#48262);
#9694=VERTEX_POINT('',#48266);
#9695=VERTEX_POINT('',#48270);
#9696=VERTEX_POINT('',#48274);
#9697=VERTEX_POINT('',#48278);
#9698=VERTEX_POINT('',#48282);
#9699=VERTEX_POINT('',#48286);
#9700=VERTEX_POINT('',#48290);
#9701=VERTEX_POINT('',#48294);
#9702=VERTEX_POINT('',#48298);
#9703=VERTEX_POINT('',#48302);
#9704=VERTEX_POINT('',#48306);
#9705=VERTEX_POINT('',#48310);
#9706=VERTEX_POINT('',#48314);
#9707=VERTEX_POINT('',#48318);
#9708=VERTEX_POINT('',#48322);
#9709=EDGE_CURVE('',#7755,#7756,#3993,.T.);
#9710=EDGE_CURVE('',#7756,#7757,#3994,.T.);
#9711=EDGE_CURVE('',#7757,#7758,#3995,.T.);
#9712=EDGE_CURVE('',#7758,#7759,#3996,.T.);
#9713=EDGE_CURVE('',#7759,#7760,#3389,.T.);
#9714=EDGE_CURVE('',#7760,#7761,#3997,.T.);
#9715=EDGE_CURVE('',#7761,#7762,#3390,.T.);
#9716=EDGE_CURVE('',#7762,#7763,#3998,.T.);
#9717=EDGE_CURVE('',#7763,#7764,#3391,.T.);
#9718=EDGE_CURVE('',#7764,#7765,#3392,.T.);
#9719=EDGE_CURVE('',#7765,#7766,#3393,.T.);
#9720=EDGE_CURVE('',#7766,#7767,#3999,.T.);
#9721=EDGE_CURVE('',#7767,#7768,#3394,.T.);
#9722=EDGE_CURVE('',#7768,#7769,#3395,.T.);
#9723=EDGE_CURVE('',#7769,#7770,#3396,.T.);
#9724=EDGE_CURVE('',#7770,#7771,#4000,.T.);
#9725=EDGE_CURVE('',#7771,#7772,#4001,.T.);
#9726=EDGE_CURVE('',#7772,#7773,#4002,.T.);
#9727=EDGE_CURVE('',#7773,#7774,#3397,.T.);
#9728=EDGE_CURVE('',#7774,#7775,#3398,.T.);
#9729=EDGE_CURVE('',#7775,#7776,#3399,.T.);
#9730=EDGE_CURVE('',#7776,#7777,#4003,.T.);
#9731=EDGE_CURVE('',#7777,#7778,#3400,.T.);
#9732=EDGE_CURVE('',#7778,#7779,#3401,.T.);
#9733=EDGE_CURVE('',#7779,#7780,#3402,.T.);
#9734=EDGE_CURVE('',#7780,#7781,#4004,.T.);
#9735=EDGE_CURVE('',#7781,#7782,#3403,.T.);
#9736=EDGE_CURVE('',#7782,#7783,#4005,.T.);
#9737=EDGE_CURVE('',#7783,#7784,#3404,.T.);
#9738=EDGE_CURVE('',#7784,#7785,#4006,.T.);
#9739=EDGE_CURVE('',#7785,#7786,#4007,.T.);
#9740=EDGE_CURVE('',#7786,#7787,#4008,.T.);
#9741=EDGE_CURVE('',#7787,#7788,#4009,.T.);
#9742=EDGE_CURVE('',#7788,#7789,#4010,.T.);
#9743=EDGE_CURVE('',#7789,#7790,#4011,.T.);
#9744=EDGE_CURVE('',#7790,#7755,#4012,.T.);
#9745=EDGE_CURVE('',#7772,#7791,#4013,.T.);
#9746=EDGE_CURVE('',#7791,#7792,#4014,.T.);
#9747=EDGE_CURVE('',#7773,#7792,#4015,.T.);
#9748=EDGE_CURVE('',#7792,#7793,#3405,.T.);
#9749=EDGE_CURVE('',#7774,#7793,#4016,.T.);
#9750=EDGE_CURVE('',#7793,#7794,#3406,.T.);
#9751=EDGE_CURVE('',#7775,#7794,#4017,.T.);
#9752=EDGE_CURVE('',#7794,#7795,#3407,.T.);
#9753=EDGE_CURVE('',#7776,#7795,#4018,.T.);
#9754=EDGE_CURVE('',#7795,#7796,#4019,.T.);
#9755=EDGE_CURVE('',#7777,#7796,#4020,.T.);
#9756=EDGE_CURVE('',#7796,#7797,#3408,.T.);
#9757=EDGE_CURVE('',#7778,#7797,#4021,.T.);
#9758=EDGE_CURVE('',#7797,#7798,#3409,.T.);
#9759=EDGE_CURVE('',#7779,#7798,#4022,.T.);
#9760=EDGE_CURVE('',#7798,#7799,#3410,.T.);
#9761=EDGE_CURVE('',#7780,#7799,#4023,.T.);
#9762=EDGE_CURVE('',#7799,#7800,#4024,.T.);
#9763=EDGE_CURVE('',#7781,#7800,#4025,.T.);
#9764=EDGE_CURVE('',#7800,#7801,#3411,.T.);
#9765=EDGE_CURVE('',#7782,#7801,#4026,.T.);
#9766=EDGE_CURVE('',#7801,#7802,#4027,.T.);
#9767=EDGE_CURVE('',#7783,#7802,#4028,.T.);
#9768=EDGE_CURVE('',#7802,#7803,#3412,.T.);
#9769=EDGE_CURVE('',#7784,#7803,#4029,.T.);
#9770=EDGE_CURVE('',#7803,#7804,#4030,.T.);
#9771=EDGE_CURVE('',#7785,#7804,#4031,.T.);
#9772=EDGE_CURVE('',#7804,#7805,#4032,.T.);
#9773=EDGE_CURVE('',#7786,#7805,#4033,.T.);
#9774=EDGE_CURVE('',#7805,#7806,#4034,.T.);
#9775=EDGE_CURVE('',#7787,#7806,#4035,.T.);
#9776=EDGE_CURVE('',#7806,#7807,#4036,.T.);
#9777=EDGE_CURVE('',#7788,#7807,#4037,.T.);
#9778=EDGE_CURVE('',#7755,#7808,#4038,.T.);
#9779=EDGE_CURVE('',#7808,#7809,#4039,.T.);
#9780=EDGE_CURVE('',#7756,#7809,#4040,.T.);
#9781=EDGE_CURVE('',#7809,#7810,#4041,.T.);
#9782=EDGE_CURVE('',#7757,#7810,#4042,.T.);
#9783=EDGE_CURVE('',#7810,#7811,#4043,.T.);
#9784=EDGE_CURVE('',#7758,#7811,#4044,.T.);
#9785=EDGE_CURVE('',#7811,#7812,#4045,.T.);
#9786=EDGE_CURVE('',#7759,#7812,#4046,.T.);
#9787=EDGE_CURVE('',#7812,#7813,#3413,.T.);
#9788=EDGE_CURVE('',#7760,#7813,#4047,.T.);
#9789=EDGE_CURVE('',#7807,#7814,#4048,.T.);
#9790=EDGE_CURVE('',#7789,#7814,#4049,.T.);
#9791=EDGE_CURVE('',#7814,#7815,#4050,.T.);
#9792=EDGE_CURVE('',#7790,#7815,#4051,.T.);
#9793=EDGE_CURVE('',#7815,#7808,#4052,.T.);
#9794=EDGE_CURVE('',#7813,#7816,#4053,.T.);
#9795=EDGE_CURVE('',#7816,#7761,#4054,.T.);
#9796=EDGE_CURVE('',#7771,#7817,#4055,.T.);
#9797=EDGE_CURVE('',#7817,#7791,#4056,.T.);
#9798=EDGE_CURVE('',#7770,#7818,#4057,.T.);
#9799=EDGE_CURVE('',#7818,#7817,#4058,.T.);
#9800=EDGE_CURVE('',#7769,#7819,#4059,.T.);
#9801=EDGE_CURVE('',#7819,#7818,#3414,.T.);
#9802=EDGE_CURVE('',#7768,#7820,#4060,.T.);
#9803=EDGE_CURVE('',#7820,#7819,#3415,.T.);
#9804=EDGE_CURVE('',#7767,#7821,#4061,.T.);
#9805=EDGE_CURVE('',#7821,#7820,#3416,.T.);
#9806=EDGE_CURVE('',#7766,#7822,#4062,.T.);
#9807=EDGE_CURVE('',#7822,#7821,#4063,.T.);
#9808=EDGE_CURVE('',#7765,#7823,#4064,.T.);
#9809=EDGE_CURVE('',#7823,#7822,#3417,.T.);
#9810=EDGE_CURVE('',#7764,#7824,#4065,.T.);
#9811=EDGE_CURVE('',#7824,#7823,#3418,.T.);
#9812=EDGE_CURVE('',#7763,#7825,#4066,.T.);
#9813=EDGE_CURVE('',#7825,#7824,#3419,.T.);
#9814=EDGE_CURVE('',#7762,#7826,#4067,.T.);
#9815=EDGE_CURVE('',#7826,#7825,#4068,.T.);
#9816=EDGE_CURVE('',#7816,#7826,#3420,.T.);
#9817=EDGE_CURVE('',#7827,#7828,#4069,.T.);
#9818=EDGE_CURVE('',#7829,#7828,#4070,.T.);
#9819=EDGE_CURVE('',#7830,#7829,#4071,.T.);
#9820=EDGE_CURVE('',#7830,#7827,#4072,.T.);
#9821=EDGE_CURVE('',#7828,#7831,#3421,.T.);
#9822=EDGE_CURVE('',#7832,#7831,#4073,.T.);
#9823=EDGE_CURVE('',#7829,#7832,#3422,.T.);
#9824=EDGE_CURVE('',#7831,#7833,#3423,.T.);
#9825=EDGE_CURVE('',#7834,#7833,#4074,.T.);
#9826=EDGE_CURVE('',#7832,#7834,#3424,.T.);
#9827=EDGE_CURVE('',#7833,#7835,#3425,.T.);
#9828=EDGE_CURVE('',#7836,#7835,#4075,.T.);
#9829=EDGE_CURVE('',#7834,#7836,#3426,.T.);
#9830=EDGE_CURVE('',#7835,#7837,#4076,.T.);
#9831=EDGE_CURVE('',#7838,#7837,#4077,.T.);
#9832=EDGE_CURVE('',#7836,#7838,#4078,.T.);
#9833=EDGE_CURVE('',#7837,#7839,#3427,.T.);
#9834=EDGE_CURVE('',#7840,#7839,#4079,.T.);
#9835=EDGE_CURVE('',#7838,#7840,#3428,.T.);
#9836=EDGE_CURVE('',#7839,#7841,#3429,.T.);
#9837=EDGE_CURVE('',#7842,#7841,#4080,.T.);
#9838=EDGE_CURVE('',#7840,#7842,#3430,.T.);
#9839=EDGE_CURVE('',#7843,#7844,#4081,.T.);
#9840=EDGE_CURVE('',#7845,#7843,#4082,.T.);
#9841=EDGE_CURVE('',#7846,#7845,#4083,.T.);
#9842=EDGE_CURVE('',#7847,#7846,#4084,.T.);
#9843=EDGE_CURVE('',#7848,#7847,#4085,.T.);
#9844=EDGE_CURVE('',#7849,#7848,#3431,.T.);
#9845=EDGE_CURVE('',#7850,#7849,#4086,.T.);
#9846=EDGE_CURVE('',#7851,#7850,#3432,.T.);
#9847=EDGE_CURVE('',#7852,#7851,#4087,.T.);
#9848=EDGE_CURVE('',#7841,#7852,#3433,.T.);
#9849=EDGE_CURVE('',#7853,#7827,#4088,.T.);
#9850=EDGE_CURVE('',#7854,#7853,#4089,.T.);
#9851=EDGE_CURVE('',#7855,#7854,#3434,.T.);
#9852=EDGE_CURVE('',#7856,#7855,#3435,.T.);
#9853=EDGE_CURVE('',#7857,#7856,#3436,.T.);
#9854=EDGE_CURVE('',#7858,#7857,#4090,.T.);
#9855=EDGE_CURVE('',#7859,#7858,#3437,.T.);
#9856=EDGE_CURVE('',#7860,#7859,#3438,.T.);
#9857=EDGE_CURVE('',#7861,#7860,#3439,.T.);
#9858=EDGE_CURVE('',#7862,#7861,#4091,.T.);
#9859=EDGE_CURVE('',#7863,#7862,#3440,.T.);
#9860=EDGE_CURVE('',#7864,#7863,#4092,.T.);
#9861=EDGE_CURVE('',#7865,#7864,#3441,.T.);
#9862=EDGE_CURVE('',#7866,#7865,#4093,.T.);
#9863=EDGE_CURVE('',#7867,#7866,#4094,.T.);
#9864=EDGE_CURVE('',#7868,#7867,#4095,.T.);
#9865=EDGE_CURVE('',#7869,#7868,#4096,.T.);
#9866=EDGE_CURVE('',#7869,#7870,#4097,.T.);
#9867=EDGE_CURVE('',#7870,#7871,#4098,.T.);
#9868=EDGE_CURVE('',#7871,#7872,#4099,.T.);
#9869=EDGE_CURVE('',#7872,#7873,#4100,.T.);
#9870=EDGE_CURVE('',#7873,#7874,#3442,.T.);
#9871=EDGE_CURVE('',#7875,#7874,#4101,.T.);
#9872=EDGE_CURVE('',#7876,#7875,#3443,.T.);
#9873=EDGE_CURVE('',#7877,#7876,#4102,.T.);
#9874=EDGE_CURVE('',#7878,#7877,#4103,.T.);
#9875=EDGE_CURVE('',#7844,#7878,#4104,.T.);
#9876=EDGE_CURVE('',#7879,#7844,#4105,.T.);
#9877=EDGE_CURVE('',#7879,#7880,#4106,.T.);
#9878=EDGE_CURVE('',#7880,#7843,#4107,.T.);
#9879=EDGE_CURVE('',#7881,#7878,#4108,.T.);
#9880=EDGE_CURVE('',#7881,#7879,#4109,.T.);
#9881=EDGE_CURVE('',#7882,#7877,#4110,.T.);
#9882=EDGE_CURVE('',#7882,#7881,#4111,.T.);
#9883=EDGE_CURVE('',#7883,#7876,#4112,.T.);
#9884=EDGE_CURVE('',#7883,#7882,#4113,.T.);
#9885=EDGE_CURVE('',#7884,#7884,#3444,.T.);
#9886=EDGE_CURVE('',#7885,#7885,#3445,.T.);
#9887=EDGE_CURVE('',#7886,#7875,#4114,.T.);
#9888=EDGE_CURVE('',#7886,#7883,#3446,.T.);
#9889=EDGE_CURVE('',#7887,#7874,#4115,.T.);
#9890=EDGE_CURVE('',#7886,#7887,#4116,.T.);
#9891=EDGE_CURVE('',#7887,#7888,#3447,.T.);
#9892=EDGE_CURVE('',#7888,#7889,#4117,.T.);
#9893=EDGE_CURVE('',#7889,#7890,#4118,.T.);
#9894=EDGE_CURVE('',#7890,#7891,#4119,.T.);
#9895=EDGE_CURVE('',#7891,#7892,#4120,.T.);
#9896=EDGE_CURVE('',#7892,#7893,#4121,.T.);
#9897=EDGE_CURVE('',#7893,#7894,#4122,.T.);
#9898=EDGE_CURVE('',#7894,#7895,#4123,.T.);
#9899=EDGE_CURVE('',#7895,#7896,#4124,.T.);
#9900=EDGE_CURVE('',#7896,#7897,#3448,.T.);
#9901=EDGE_CURVE('',#7897,#7898,#4125,.T.);
#9902=EDGE_CURVE('',#7898,#7899,#3449,.T.);
#9903=EDGE_CURVE('',#7899,#7900,#4126,.T.);
#9904=EDGE_CURVE('',#7900,#7901,#3450,.T.);
#9905=EDGE_CURVE('',#7901,#7902,#3451,.T.);
#9906=EDGE_CURVE('',#7902,#7903,#3452,.T.);
#9907=EDGE_CURVE('',#7903,#7904,#4127,.T.);
#9908=EDGE_CURVE('',#7904,#7905,#3453,.T.);
#9909=EDGE_CURVE('',#7905,#7906,#3454,.T.);
#9910=EDGE_CURVE('',#7906,#7907,#3455,.T.);
#9911=EDGE_CURVE('',#7907,#7908,#4128,.T.);
#9912=EDGE_CURVE('',#7908,#7830,#4129,.T.);
#9913=EDGE_CURVE('',#7842,#7909,#3456,.T.);
#9914=EDGE_CURVE('',#7909,#7910,#4130,.T.);
#9915=EDGE_CURVE('',#7910,#7911,#3457,.T.);
#9916=EDGE_CURVE('',#7911,#7912,#4131,.T.);
#9917=EDGE_CURVE('',#7912,#7913,#3458,.T.);
#9918=EDGE_CURVE('',#7913,#7914,#4132,.T.);
#9919=EDGE_CURVE('',#7914,#7915,#4133,.T.);
#9920=EDGE_CURVE('',#7915,#7916,#4134,.T.);
#9921=EDGE_CURVE('',#7916,#7880,#4135,.T.);
#9922=EDGE_CURVE('',#7891,#7870,#4136,.T.);
#9923=EDGE_CURVE('',#7869,#7892,#4137,.T.);
#9924=EDGE_CURVE('',#7890,#7871,#4138,.T.);
#9925=EDGE_CURVE('',#7889,#7872,#4139,.T.);
#9926=EDGE_CURVE('',#7888,#7873,#4140,.T.);
#9927=EDGE_CURVE('',#7917,#7917,#3459,.T.);
#9928=EDGE_CURVE('',#7918,#7918,#3460,.T.);
#9929=EDGE_CURVE('',#7885,#7919,#4141,.T.);
#9930=EDGE_CURVE('',#7919,#7919,#3461,.T.);
#9931=EDGE_CURVE('',#7918,#7920,#4142,.T.);
#9932=EDGE_CURVE('',#7920,#7920,#3462,.T.);
#9933=EDGE_CURVE('',#7884,#7921,#4143,.T.);
#9934=EDGE_CURVE('',#7921,#7921,#3463,.T.);
#9935=EDGE_CURVE('',#7917,#7922,#4144,.T.);
#9936=EDGE_CURVE('',#7922,#7922,#3464,.T.);
#9937=EDGE_CURVE('',#7916,#7845,#4145,.T.);
#9938=EDGE_CURVE('',#7915,#7846,#4146,.T.);
#9939=EDGE_CURVE('',#7914,#7847,#4147,.T.);
#9940=EDGE_CURVE('',#7913,#7848,#4148,.T.);
#9941=EDGE_CURVE('',#7912,#7849,#4149,.T.);
#9942=EDGE_CURVE('',#7911,#7850,#4150,.T.);
#9943=EDGE_CURVE('',#7910,#7851,#4151,.T.);
#9944=EDGE_CURVE('',#7909,#7852,#4152,.T.);
#9945=EDGE_CURVE('',#7893,#7868,#4153,.T.);
#9946=EDGE_CURVE('',#7894,#7867,#4154,.T.);
#9947=EDGE_CURVE('',#7895,#7866,#4155,.T.);
#9948=EDGE_CURVE('',#7896,#7865,#4156,.T.);
#9949=EDGE_CURVE('',#7897,#7864,#4157,.T.);
#9950=EDGE_CURVE('',#7863,#7898,#4158,.T.);
#9951=EDGE_CURVE('',#7899,#7862,#4159,.T.);
#9952=EDGE_CURVE('',#7900,#7861,#4160,.T.);
#9953=EDGE_CURVE('',#7901,#7860,#4161,.T.);
#9954=EDGE_CURVE('',#7902,#7859,#4162,.T.);
#9955=EDGE_CURVE('',#7903,#7858,#4163,.T.);
#9956=EDGE_CURVE('',#7904,#7857,#4164,.T.);
#9957=EDGE_CURVE('',#7905,#7856,#4165,.T.);
#9958=EDGE_CURVE('',#7906,#7855,#4166,.T.);
#9959=EDGE_CURVE('',#7907,#7854,#4167,.T.);
#9960=EDGE_CURVE('',#7908,#7853,#4168,.T.);
#9961=EDGE_CURVE('',#7923,#7924,#3465,.T.);
#9962=EDGE_CURVE('',#7925,#7924,#4169,.T.);
#9963=EDGE_CURVE('',#7925,#7926,#3466,.T.);
#9964=EDGE_CURVE('',#7926,#7923,#4170,.T.);
#9965=EDGE_CURVE('',#7924,#7927,#4171,.T.);
#9966=EDGE_CURVE('',#7928,#7927,#4172,.T.);
#9967=EDGE_CURVE('',#7928,#7925,#4173,.T.);
#9968=EDGE_CURVE('',#7927,#7929,#3467,.T.);
#9969=EDGE_CURVE('',#7930,#7929,#4174,.T.);
#9970=EDGE_CURVE('',#7930,#7928,#3468,.T.);
#9971=EDGE_CURVE('',#7929,#7931,#4175,.T.);
#9972=EDGE_CURVE('',#7932,#7931,#4176,.T.);
#9973=EDGE_CURVE('',#7932,#7930,#4177,.T.);
#9974=EDGE_CURVE('',#7931,#7933,#3469,.T.);
#9975=EDGE_CURVE('',#7934,#7933,#4178,.T.);
#9976=EDGE_CURVE('',#7934,#7932,#3470,.T.);
#9977=EDGE_CURVE('',#7933,#7935,#4179,.T.);
#9978=EDGE_CURVE('',#7936,#7935,#4180,.T.);
#9979=EDGE_CURVE('',#7936,#7934,#4181,.T.);
#9980=EDGE_CURVE('',#7935,#7937,#4182,.T.);
#9981=EDGE_CURVE('',#7938,#7937,#4183,.T.);
#9982=EDGE_CURVE('',#7938,#7936,#4184,.T.);
#9983=EDGE_CURVE('',#7937,#7939,#4185,.T.);
#9984=EDGE_CURVE('',#7940,#7939,#4186,.T.);
#9985=EDGE_CURVE('',#7940,#7938,#4187,.T.);
#9986=EDGE_CURVE('',#7941,#7942,#4188,.T.);
#9987=EDGE_CURVE('',#7943,#7941,#4189,.T.);
#9988=EDGE_CURVE('',#7943,#7944,#4190,.T.);
#9989=EDGE_CURVE('',#7944,#7942,#4191,.T.);
#9990=EDGE_CURVE('',#7945,#7941,#4192,.T.);
#9991=EDGE_CURVE('',#7946,#7945,#4193,.T.);
#9992=EDGE_CURVE('',#7946,#7943,#4194,.T.);
#9993=EDGE_CURVE('',#7947,#7945,#4195,.T.);
#9994=EDGE_CURVE('',#7948,#7947,#4196,.T.);
#9995=EDGE_CURVE('',#7948,#7946,#4197,.T.);
#9996=EDGE_CURVE('',#7947,#7949,#4198,.T.);
#9997=EDGE_CURVE('',#7950,#7949,#4199,.T.);
#9998=EDGE_CURVE('',#7950,#7948,#4200,.T.);
#9999=EDGE_CURVE('',#7949,#7951,#4201,.T.);
#10000=EDGE_CURVE('',#7952,#7951,#4202,.T.);
#10001=EDGE_CURVE('',#7952,#7950,#4203,.T.);
#10002=EDGE_CURVE('',#7951,#7953,#4204,.T.);
#10003=EDGE_CURVE('',#7954,#7953,#4205,.T.);
#10004=EDGE_CURVE('',#7954,#7952,#4206,.T.);
#10005=EDGE_CURVE('',#7953,#7955,#4207,.T.);
#10006=EDGE_CURVE('',#7956,#7955,#4208,.T.);
#10007=EDGE_CURVE('',#7956,#7954,#4209,.T.);
#10008=EDGE_CURVE('',#7955,#7957,#3471,.T.);
#10009=EDGE_CURVE('',#7958,#7957,#4210,.T.);
#10010=EDGE_CURVE('',#7958,#7956,#3472,.T.);
#10011=EDGE_CURVE('',#7959,#7960,#3473,.T.);
#10012=EDGE_CURVE('',#7961,#7959,#4211,.T.);
#10013=EDGE_CURVE('',#7962,#7961,#3474,.T.);
#10014=EDGE_CURVE('',#7963,#7962,#3475,.T.);
#10015=EDGE_CURVE('',#7964,#7963,#3476,.T.);
#10016=EDGE_CURVE('',#7965,#7964,#4212,.T.);
#10017=EDGE_CURVE('',#7966,#7965,#3477,.T.);
#10018=EDGE_CURVE('',#7967,#7966,#3478,.T.);
#10019=EDGE_CURVE('',#7968,#7967,#3479,.T.);
#10020=EDGE_CURVE('',#7969,#7968,#4213,.T.);
#10021=EDGE_CURVE('',#7970,#7969,#4214,.T.);
#10022=EDGE_CURVE('',#7971,#7970,#4215,.T.);
#10023=EDGE_CURVE('',#7972,#7971,#3480,.T.);
#10024=EDGE_CURVE('',#7973,#7972,#3481,.T.);
#10025=EDGE_CURVE('',#7974,#7973,#3482,.T.);
#10026=EDGE_CURVE('',#7975,#7974,#4216,.T.);
#10027=EDGE_CURVE('',#7976,#7975,#3483,.T.);
#10028=EDGE_CURVE('',#7926,#7976,#3484,.T.);
#10029=EDGE_CURVE('',#7944,#7940,#4217,.T.);
#10030=EDGE_CURVE('',#7960,#7958,#4218,.T.);
#10031=EDGE_CURVE('',#7939,#7942,#4219,.T.);
#10032=EDGE_CURVE('',#7957,#7977,#4220,.T.);
#10033=EDGE_CURVE('',#7977,#7960,#4221,.T.);
#10034=EDGE_CURVE('',#7977,#7978,#3485,.T.);
#10035=EDGE_CURVE('',#7959,#7978,#4222,.T.);
#10036=EDGE_CURVE('',#7978,#7979,#4223,.T.);
#10037=EDGE_CURVE('',#7961,#7979,#4224,.T.);
#10038=EDGE_CURVE('',#7979,#7980,#3486,.T.);
#10039=EDGE_CURVE('',#7962,#7980,#4225,.T.);
#10040=EDGE_CURVE('',#7980,#7981,#3487,.T.);
#10041=EDGE_CURVE('',#7963,#7981,#4226,.T.);
#10042=EDGE_CURVE('',#7981,#7982,#3488,.T.);
#10043=EDGE_CURVE('',#7964,#7982,#4227,.T.);
#10044=EDGE_CURVE('',#7982,#7983,#4228,.T.);
#10045=EDGE_CURVE('',#7965,#7983,#4229,.T.);
#10046=EDGE_CURVE('',#7983,#7984,#3489,.T.);
#10047=EDGE_CURVE('',#7966,#7984,#4230,.T.);
#10048=EDGE_CURVE('',#7984,#7985,#3490,.T.);
#10049=EDGE_CURVE('',#7967,#7985,#4231,.T.);
#10050=EDGE_CURVE('',#7985,#7986,#3491,.T.);
#10051=EDGE_CURVE('',#7968,#7986,#4232,.T.);
#10052=EDGE_CURVE('',#7986,#7987,#4233,.T.);
#10053=EDGE_CURVE('',#7969,#7987,#4234,.T.);
#10054=EDGE_CURVE('',#7987,#7988,#4235,.T.);
#10055=EDGE_CURVE('',#7970,#7988,#4236,.T.);
#10056=EDGE_CURVE('',#7988,#7989,#4237,.T.);
#10057=EDGE_CURVE('',#7971,#7989,#4238,.T.);
#10058=EDGE_CURVE('',#7989,#7990,#3492,.T.);
#10059=EDGE_CURVE('',#7972,#7990,#4239,.T.);
#10060=EDGE_CURVE('',#7990,#7991,#3493,.T.);
#10061=EDGE_CURVE('',#7973,#7991,#4240,.T.);
#10062=EDGE_CURVE('',#7991,#7992,#3494,.T.);
#10063=EDGE_CURVE('',#7974,#7992,#4241,.T.);
#10064=EDGE_CURVE('',#7992,#7993,#4242,.T.);
#10065=EDGE_CURVE('',#7975,#7993,#4243,.T.);
#10066=EDGE_CURVE('',#7993,#7994,#3495,.T.);
#10067=EDGE_CURVE('',#7976,#7994,#4244,.T.);
#10068=EDGE_CURVE('',#7994,#7923,#3496,.T.);
#10069=EDGE_CURVE('',#7995,#7996,#4245,.T.);
#10070=EDGE_CURVE('',#7997,#7995,#4246,.T.);
#10071=EDGE_CURVE('',#7998,#7997,#4247,.T.);
#10072=EDGE_CURVE('',#7999,#7998,#4248,.T.);
#10073=EDGE_CURVE('',#8000,#7999,#4249,.T.);
#10074=EDGE_CURVE('',#8001,#8000,#4250,.T.);
#10075=EDGE_CURVE('',#8002,#8001,#4251,.T.);
#10076=EDGE_CURVE('',#8003,#8002,#4252,.T.);
#10077=EDGE_CURVE('',#8004,#8003,#3497,.T.);
#10078=EDGE_CURVE('',#8005,#8004,#4253,.T.);
#10079=EDGE_CURVE('',#8006,#8005,#3498,.T.);
#10080=EDGE_CURVE('',#8007,#8006,#4254,.T.);
#10081=EDGE_CURVE('',#8008,#8007,#3499,.T.);
#10082=EDGE_CURVE('',#8009,#8008,#3500,.T.);
#10083=EDGE_CURVE('',#8010,#8009,#3501,.T.);
#10084=EDGE_CURVE('',#8011,#8010,#4255,.T.);
#10085=EDGE_CURVE('',#8012,#8011,#3502,.T.);
#10086=EDGE_CURVE('',#8013,#8012,#3503,.T.);
#10087=EDGE_CURVE('',#8014,#8013,#3504,.T.);
#10088=EDGE_CURVE('',#8015,#8014,#4256,.T.);
#10089=EDGE_CURVE('',#8016,#8015,#4257,.T.);
#10090=EDGE_CURVE('',#8017,#8016,#4258,.T.);
#10091=EDGE_CURVE('',#8018,#8017,#3505,.T.);
#10092=EDGE_CURVE('',#8019,#8018,#3506,.T.);
#10093=EDGE_CURVE('',#8020,#8019,#3507,.T.);
#10094=EDGE_CURVE('',#8021,#8020,#4259,.T.);
#10095=EDGE_CURVE('',#8022,#8021,#3508,.T.);
#10096=EDGE_CURVE('',#8023,#8022,#3509,.T.);
#10097=EDGE_CURVE('',#8024,#8023,#3510,.T.);
#10098=EDGE_CURVE('',#8025,#8024,#4260,.T.);
#10099=EDGE_CURVE('',#8026,#8025,#3511,.T.);
#10100=EDGE_CURVE('',#8027,#8026,#4261,.T.);
#10101=EDGE_CURVE('',#8028,#8027,#3512,.T.);
#10102=EDGE_CURVE('',#8029,#8028,#4262,.T.);
#10103=EDGE_CURVE('',#8030,#8029,#4263,.T.);
#10104=EDGE_CURVE('',#7996,#8030,#4264,.T.);
#10105=EDGE_CURVE('',#8014,#8031,#4265,.T.);
#10106=EDGE_CURVE('',#8032,#8031,#4266,.T.);
#10107=EDGE_CURVE('',#8015,#8032,#4267,.T.);
#10108=EDGE_CURVE('',#8013,#8033,#4268,.T.);
#10109=EDGE_CURVE('',#8031,#8033,#3513,.T.);
#10110=EDGE_CURVE('',#8012,#8034,#4269,.T.);
#10111=EDGE_CURVE('',#8033,#8034,#3514,.T.);
#10112=EDGE_CURVE('',#8011,#8035,#4270,.T.);
#10113=EDGE_CURVE('',#8034,#8035,#3515,.T.);
#10114=EDGE_CURVE('',#8010,#8036,#4271,.T.);
#10115=EDGE_CURVE('',#8035,#8036,#4272,.T.);
#10116=EDGE_CURVE('',#8009,#8037,#4273,.T.);
#10117=EDGE_CURVE('',#8036,#8037,#3516,.T.);
#10118=EDGE_CURVE('',#8008,#8038,#4274,.T.);
#10119=EDGE_CURVE('',#8037,#8038,#3517,.T.);
#10120=EDGE_CURVE('',#8007,#8039,#4275,.T.);
#10121=EDGE_CURVE('',#8038,#8039,#3518,.T.);
#10122=EDGE_CURVE('',#8006,#8040,#4276,.T.);
#10123=EDGE_CURVE('',#8039,#8040,#4277,.T.);
#10124=EDGE_CURVE('',#8005,#8041,#4278,.T.);
#10125=EDGE_CURVE('',#8040,#8041,#3519,.T.);
#10126=EDGE_CURVE('',#8004,#8042,#4279,.T.);
#10127=EDGE_CURVE('',#8041,#8042,#4280,.T.);
#10128=EDGE_CURVE('',#8003,#8043,#4281,.T.);
#10129=EDGE_CURVE('',#8042,#8043,#3520,.T.);
#10130=EDGE_CURVE('',#8002,#8044,#4282,.T.);
#10131=EDGE_CURVE('',#8043,#8044,#4283,.T.);
#10132=EDGE_CURVE('',#8001,#8045,#4284,.T.);
#10133=EDGE_CURVE('',#8044,#8045,#4285,.T.);
#10134=EDGE_CURVE('',#8000,#8046,#4286,.T.);
#10135=EDGE_CURVE('',#8045,#8046,#4287,.T.);
#10136=EDGE_CURVE('',#7999,#8047,#4288,.T.);
#10137=EDGE_CURVE('',#8046,#8047,#4289,.T.);
#10138=EDGE_CURVE('',#7996,#8048,#4290,.T.);
#10139=EDGE_CURVE('',#8049,#8048,#4291,.T.);
#10140=EDGE_CURVE('',#7995,#8049,#4292,.T.);
#10141=EDGE_CURVE('',#8030,#8050,#4293,.T.);
#10142=EDGE_CURVE('',#8048,#8050,#4294,.T.);
#10143=EDGE_CURVE('',#8029,#8051,#4295,.T.);
#10144=EDGE_CURVE('',#8050,#8051,#4296,.T.);
#10145=EDGE_CURVE('',#8028,#8052,#4297,.T.);
#10146=EDGE_CURVE('',#8051,#8052,#4298,.T.);
#10147=EDGE_CURVE('',#8027,#8053,#4299,.T.);
#10148=EDGE_CURVE('',#8052,#8053,#3521,.T.);
#10149=EDGE_CURVE('',#7998,#8054,#4300,.T.);
#10150=EDGE_CURVE('',#8047,#8054,#4301,.T.);
#10151=EDGE_CURVE('',#7997,#8055,#4302,.T.);
#10152=EDGE_CURVE('',#8054,#8055,#4303,.T.);
#10153=EDGE_CURVE('',#8055,#8049,#4304,.T.);
#10154=EDGE_CURVE('',#8056,#8026,#4305,.T.);
#10155=EDGE_CURVE('',#8053,#8056,#4306,.T.);
#10156=EDGE_CURVE('',#8057,#8032,#4307,.T.);
#10157=EDGE_CURVE('',#8016,#8057,#4308,.T.);
#10158=EDGE_CURVE('',#8058,#8057,#4309,.T.);
#10159=EDGE_CURVE('',#8017,#8058,#4310,.T.);
#10160=EDGE_CURVE('',#8059,#8058,#3522,.T.);
#10161=EDGE_CURVE('',#8018,#8059,#4311,.T.);
#10162=EDGE_CURVE('',#8060,#8059,#3523,.T.);
#10163=EDGE_CURVE('',#8019,#8060,#4312,.T.);
#10164=EDGE_CURVE('',#8061,#8060,#3524,.T.);
#10165=EDGE_CURVE('',#8020,#8061,#4313,.T.);
#10166=EDGE_CURVE('',#8062,#8061,#4314,.T.);
#10167=EDGE_CURVE('',#8021,#8062,#4315,.T.);
#10168=EDGE_CURVE('',#8063,#8062,#3525,.T.);
#10169=EDGE_CURVE('',#8022,#8063,#4316,.T.);
#10170=EDGE_CURVE('',#8064,#8063,#3526,.T.);
#10171=EDGE_CURVE('',#8023,#8064,#4317,.T.);
#10172=EDGE_CURVE('',#8065,#8064,#3527,.T.);
#10173=EDGE_CURVE('',#8024,#8065,#4318,.T.);
#10174=EDGE_CURVE('',#8066,#8065,#4319,.T.);
#10175=EDGE_CURVE('',#8025,#8066,#4320,.T.);
#10176=EDGE_CURVE('',#8056,#8066,#3528,.T.);
#10177=EDGE_CURVE('',#8067,#8068,#4321,.T.);
#10178=EDGE_CURVE('',#8069,#8067,#4322,.T.);
#10179=EDGE_CURVE('',#8069,#8070,#4323,.T.);
#10180=EDGE_CURVE('',#8070,#8068,#4324,.T.);
#10181=EDGE_CURVE('',#8068,#8071,#3529,.T.);
#10182=EDGE_CURVE('',#8070,#8072,#3530,.T.);
#10183=EDGE_CURVE('',#8072,#8071,#4325,.T.);
#10184=EDGE_CURVE('',#8071,#8073,#3531,.T.);
#10185=EDGE_CURVE('',#8072,#8074,#3532,.T.);
#10186=EDGE_CURVE('',#8074,#8073,#4326,.T.);
#10187=EDGE_CURVE('',#8073,#8075,#3533,.T.);
#10188=EDGE_CURVE('',#8074,#8076,#3534,.T.);
#10189=EDGE_CURVE('',#8076,#8075,#4327,.T.);
#10190=EDGE_CURVE('',#8075,#8077,#4328,.T.);
#10191=EDGE_CURVE('',#8076,#8078,#4329,.T.);
#10192=EDGE_CURVE('',#8078,#8077,#4330,.T.);
#10193=EDGE_CURVE('',#8077,#8079,#3535,.T.);
#10194=EDGE_CURVE('',#8078,#8080,#3536,.T.);
#10195=EDGE_CURVE('',#8080,#8079,#4331,.T.);
#10196=EDGE_CURVE('',#8079,#8081,#3537,.T.);
#10197=EDGE_CURVE('',#8080,#8082,#3538,.T.);
#10198=EDGE_CURVE('',#8082,#8081,#4332,.T.);
#10199=EDGE_CURVE('',#8083,#8084,#4333,.T.);
#10200=EDGE_CURVE('',#8084,#8085,#4334,.T.);
#10201=EDGE_CURVE('',#8085,#8086,#4335,.T.);
#10202=EDGE_CURVE('',#8086,#8087,#4336,.T.);
#10203=EDGE_CURVE('',#8087,#8088,#3539,.T.);
#10204=EDGE_CURVE('',#8088,#8089,#4337,.T.);
#10205=EDGE_CURVE('',#8090,#8089,#3540,.T.);
#10206=EDGE_CURVE('',#8091,#8090,#4338,.T.);
#10207=EDGE_CURVE('',#8092,#8091,#4339,.T.);
#10208=EDGE_CURVE('',#8093,#8092,#4340,.T.);
#10209=EDGE_CURVE('',#8094,#8093,#4341,.T.);
#10210=EDGE_CURVE('',#8094,#8095,#4342,.T.);
#10211=EDGE_CURVE('',#8095,#8096,#4343,.T.);
#10212=EDGE_CURVE('',#8096,#8097,#4344,.T.);
#10213=EDGE_CURVE('',#8097,#8098,#4345,.T.);
#10214=EDGE_CURVE('',#8098,#8099,#3541,.T.);
#10215=EDGE_CURVE('',#8099,#8100,#4346,.T.);
#10216=EDGE_CURVE('',#8100,#8101,#3542,.T.);
#10217=EDGE_CURVE('',#8101,#8102,#4347,.T.);
#10218=EDGE_CURVE('',#8102,#8103,#3543,.T.);
#10219=EDGE_CURVE('',#8103,#8104,#3544,.T.);
#10220=EDGE_CURVE('',#8104,#8105,#3545,.T.);
#10221=EDGE_CURVE('',#8105,#8106,#4348,.T.);
#10222=EDGE_CURVE('',#8106,#8107,#3546,.T.);
#10223=EDGE_CURVE('',#8107,#8108,#3547,.T.);
#10224=EDGE_CURVE('',#8108,#8109,#3548,.T.);
#10225=EDGE_CURVE('',#8109,#8110,#4349,.T.);
#10226=EDGE_CURVE('',#8110,#8067,#4350,.T.);
#10227=EDGE_CURVE('',#8081,#8111,#3549,.T.);
#10228=EDGE_CURVE('',#8111,#8112,#4351,.T.);
#10229=EDGE_CURVE('',#8112,#8113,#3550,.T.);
#10230=EDGE_CURVE('',#8113,#8114,#4352,.T.);
#10231=EDGE_CURVE('',#8114,#8115,#3551,.T.);
#10232=EDGE_CURVE('',#8115,#8116,#4353,.T.);
#10233=EDGE_CURVE('',#8116,#8117,#4354,.T.);
#10234=EDGE_CURVE('',#8117,#8118,#4355,.T.);
#10235=EDGE_CURVE('',#8118,#8083,#4356,.T.);
#10236=EDGE_CURVE('',#8119,#8084,#4357,.T.);
#10237=EDGE_CURVE('',#8120,#8083,#4358,.T.);
#10238=EDGE_CURVE('',#8119,#8120,#4359,.T.);
#10239=EDGE_CURVE('',#8121,#8085,#4360,.T.);
#10240=EDGE_CURVE('',#8121,#8119,#4361,.T.);
#10241=EDGE_CURVE('',#8122,#8086,#4362,.T.);
#10242=EDGE_CURVE('',#8122,#8121,#4363,.T.);
#10243=EDGE_CURVE('',#8123,#8087,#4364,.T.);
#10244=EDGE_CURVE('',#8123,#8122,#4365,.T.);
#10245=EDGE_CURVE('',#8124,#8124,#3552,.T.);
#10246=EDGE_CURVE('',#8125,#8125,#3553,.T.);
#10247=EDGE_CURVE('',#8126,#8088,#4366,.T.);
#10248=EDGE_CURVE('',#8126,#8123,#3554,.T.);
#10249=EDGE_CURVE('',#8126,#8127,#4367,.T.);
#10250=EDGE_CURVE('',#8127,#8089,#4368,.T.);
#10251=EDGE_CURVE('',#8128,#8120,#4369,.T.);
#10252=EDGE_CURVE('',#8129,#8128,#4370,.T.);
#10253=EDGE_CURVE('',#8130,#8129,#4371,.T.);
#10254=EDGE_CURVE('',#8131,#8130,#4372,.T.);
#10255=EDGE_CURVE('',#8132,#8131,#3555,.T.);
#10256=EDGE_CURVE('',#8133,#8132,#4373,.T.);
#10257=EDGE_CURVE('',#8134,#8133,#3556,.T.);
#10258=EDGE_CURVE('',#8135,#8134,#4374,.T.);
#10259=EDGE_CURVE('',#8082,#8135,#3557,.T.);
#10260=EDGE_CURVE('',#8136,#8069,#4375,.T.);
#10261=EDGE_CURVE('',#8137,#8136,#4376,.T.);
#10262=EDGE_CURVE('',#8138,#8137,#3558,.T.);
#10263=EDGE_CURVE('',#8139,#8138,#3559,.T.);
#10264=EDGE_CURVE('',#8140,#8139,#3560,.T.);
#10265=EDGE_CURVE('',#8141,#8140,#4377,.T.);
#10266=EDGE_CURVE('',#8142,#8141,#3561,.T.);
#10267=EDGE_CURVE('',#8143,#8142,#3562,.T.);
#10268=EDGE_CURVE('',#8144,#8143,#3563,.T.);
#10269=EDGE_CURVE('',#8145,#8144,#4378,.T.);
#10270=EDGE_CURVE('',#8146,#8145,#3564,.T.);
#10271=EDGE_CURVE('',#8147,#8146,#4379,.T.);
#10272=EDGE_CURVE('',#8148,#8147,#3565,.T.);
#10273=EDGE_CURVE('',#8149,#8148,#4380,.T.);
#10274=EDGE_CURVE('',#8150,#8149,#4381,.T.);
#10275=EDGE_CURVE('',#8151,#8150,#4382,.T.);
#10276=EDGE_CURVE('',#8152,#8151,#4383,.T.);
#10277=EDGE_CURVE('',#8153,#8152,#4384,.T.);
#10278=EDGE_CURVE('',#8154,#8153,#4385,.T.);
#10279=EDGE_CURVE('',#8155,#8154,#4386,.T.);
#10280=EDGE_CURVE('',#8156,#8155,#4387,.T.);
#10281=EDGE_CURVE('',#8127,#8156,#3566,.T.);
#10282=EDGE_CURVE('',#8153,#8093,#4388,.T.);
#10283=EDGE_CURVE('',#8094,#8152,#4389,.T.);
#10284=EDGE_CURVE('',#8154,#8092,#4390,.T.);
#10285=EDGE_CURVE('',#8155,#8091,#4391,.T.);
#10286=EDGE_CURVE('',#8156,#8090,#4392,.T.);
#10287=EDGE_CURVE('',#8157,#8157,#3567,.T.);
#10288=EDGE_CURVE('',#8158,#8158,#3568,.T.);
#10289=EDGE_CURVE('',#8125,#8159,#4393,.T.);
#10290=EDGE_CURVE('',#8159,#8159,#3569,.T.);
#10291=EDGE_CURVE('',#8158,#8160,#4394,.T.);
#10292=EDGE_CURVE('',#8160,#8160,#3570,.T.);
#10293=EDGE_CURVE('',#8124,#8161,#4395,.T.);
#10294=EDGE_CURVE('',#8161,#8161,#3571,.T.);
#10295=EDGE_CURVE('',#8157,#8162,#4396,.T.);
#10296=EDGE_CURVE('',#8162,#8162,#3572,.T.);
#10297=EDGE_CURVE('',#8128,#8118,#4397,.T.);
#10298=EDGE_CURVE('',#8129,#8117,#4398,.T.);
#10299=EDGE_CURVE('',#8130,#8116,#4399,.T.);
#10300=EDGE_CURVE('',#8131,#8115,#4400,.T.);
#10301=EDGE_CURVE('',#8132,#8114,#4401,.T.);
#10302=EDGE_CURVE('',#8133,#8113,#4402,.T.);
#10303=EDGE_CURVE('',#8134,#8112,#4403,.T.);
#10304=EDGE_CURVE('',#8135,#8111,#4404,.T.);
#10305=EDGE_CURVE('',#8151,#8095,#4405,.T.);
#10306=EDGE_CURVE('',#8150,#8096,#4406,.T.);
#10307=EDGE_CURVE('',#8149,#8097,#4407,.T.);
#10308=EDGE_CURVE('',#8148,#8098,#4408,.T.);
#10309=EDGE_CURVE('',#8147,#8099,#4409,.T.);
#10310=EDGE_CURVE('',#8100,#8146,#4410,.T.);
#10311=EDGE_CURVE('',#8145,#8101,#4411,.T.);
#10312=EDGE_CURVE('',#8144,#8102,#4412,.T.);
#10313=EDGE_CURVE('',#8143,#8103,#4413,.T.);
#10314=EDGE_CURVE('',#8142,#8104,#4414,.T.);
#10315=EDGE_CURVE('',#8141,#8105,#4415,.T.);
#10316=EDGE_CURVE('',#8140,#8106,#4416,.T.);
#10317=EDGE_CURVE('',#8139,#8107,#4417,.T.);
#10318=EDGE_CURVE('',#8138,#8108,#4418,.T.);
#10319=EDGE_CURVE('',#8137,#8109,#4419,.T.);
#10320=EDGE_CURVE('',#8136,#8110,#4420,.T.);
#10321=EDGE_CURVE('',#8163,#8164,#3573,.T.);
#10322=EDGE_CURVE('',#8165,#8163,#4421,.T.);
#10323=EDGE_CURVE('',#8166,#8165,#3574,.T.);
#10324=EDGE_CURVE('',#8166,#8164,#4422,.T.);
#10325=EDGE_CURVE('',#8164,#8167,#4423,.T.);
#10326=EDGE_CURVE('',#8168,#8166,#4424,.T.);
#10327=EDGE_CURVE('',#8168,#8167,#4425,.T.);
#10328=EDGE_CURVE('',#8167,#8169,#3575,.T.);
#10329=EDGE_CURVE('',#8170,#8168,#3576,.T.);
#10330=EDGE_CURVE('',#8170,#8169,#4426,.T.);
#10331=EDGE_CURVE('',#8169,#8171,#4427,.T.);
#10332=EDGE_CURVE('',#8172,#8170,#4428,.T.);
#10333=EDGE_CURVE('',#8172,#8171,#4429,.T.);
#10334=EDGE_CURVE('',#8171,#8173,#3577,.T.);
#10335=EDGE_CURVE('',#8174,#8172,#3578,.T.);
#10336=EDGE_CURVE('',#8174,#8173,#4430,.T.);
#10337=EDGE_CURVE('',#8173,#8175,#4431,.T.);
#10338=EDGE_CURVE('',#8176,#8174,#4432,.T.);
#10339=EDGE_CURVE('',#8176,#8175,#4433,.T.);
#10340=EDGE_CURVE('',#8175,#8177,#4434,.T.);
#10341=EDGE_CURVE('',#8178,#8176,#4435,.T.);
#10342=EDGE_CURVE('',#8178,#8177,#4436,.T.);
#10343=EDGE_CURVE('',#8177,#8179,#4437,.T.);
#10344=EDGE_CURVE('',#8180,#8178,#4438,.T.);
#10345=EDGE_CURVE('',#8180,#8179,#4439,.T.);
#10346=EDGE_CURVE('',#8181,#8182,#4440,.T.);
#10347=EDGE_CURVE('',#8183,#8182,#4441,.T.);
#10348=EDGE_CURVE('',#8184,#8183,#4442,.T.);
#10349=EDGE_CURVE('',#8184,#8181,#4443,.T.);
#10350=EDGE_CURVE('',#8185,#8181,#4444,.T.);
#10351=EDGE_CURVE('',#8186,#8184,#4445,.T.);
#10352=EDGE_CURVE('',#8186,#8185,#4446,.T.);
#10353=EDGE_CURVE('',#8187,#8185,#4447,.T.);
#10354=EDGE_CURVE('',#8188,#8186,#4448,.T.);
#10355=EDGE_CURVE('',#8188,#8187,#4449,.T.);
#10356=EDGE_CURVE('',#8187,#8189,#4450,.T.);
#10357=EDGE_CURVE('',#8190,#8188,#4451,.T.);
#10358=EDGE_CURVE('',#8190,#8189,#4452,.T.);
#10359=EDGE_CURVE('',#8189,#8191,#4453,.T.);
#10360=EDGE_CURVE('',#8192,#8190,#4454,.T.);
#10361=EDGE_CURVE('',#8192,#8191,#4455,.T.);
#10362=EDGE_CURVE('',#8191,#8193,#4456,.T.);
#10363=EDGE_CURVE('',#8194,#8192,#4457,.T.);
#10364=EDGE_CURVE('',#8194,#8193,#4458,.T.);
#10365=EDGE_CURVE('',#8193,#8195,#4459,.T.);
#10366=EDGE_CURVE('',#8196,#8194,#4460,.T.);
#10367=EDGE_CURVE('',#8196,#8195,#4461,.T.);
#10368=EDGE_CURVE('',#8195,#8197,#3579,.T.);
#10369=EDGE_CURVE('',#8198,#8196,#3580,.T.);
#10370=EDGE_CURVE('',#8198,#8197,#4462,.T.);
#10371=EDGE_CURVE('',#8199,#8200,#3581,.T.);
#10372=EDGE_CURVE('',#8200,#8198,#4463,.T.);
#10373=EDGE_CURVE('',#8183,#8180,#4464,.T.);
#10374=EDGE_CURVE('',#8165,#8201,#3582,.T.);
#10375=EDGE_CURVE('',#8201,#8202,#3583,.T.);
#10376=EDGE_CURVE('',#8202,#8203,#4465,.T.);
#10377=EDGE_CURVE('',#8203,#8204,#3584,.T.);
#10378=EDGE_CURVE('',#8204,#8205,#3585,.T.);
#10379=EDGE_CURVE('',#8205,#8206,#3586,.T.);
#10380=EDGE_CURVE('',#8206,#8207,#4466,.T.);
#10381=EDGE_CURVE('',#8207,#8208,#4467,.T.);
#10382=EDGE_CURVE('',#8208,#8209,#4468,.T.);
#10383=EDGE_CURVE('',#8209,#8210,#3587,.T.);
#10384=EDGE_CURVE('',#8210,#8211,#3588,.T.);
#10385=EDGE_CURVE('',#8211,#8212,#3589,.T.);
#10386=EDGE_CURVE('',#8212,#8213,#4469,.T.);
#10387=EDGE_CURVE('',#8213,#8214,#3590,.T.);
#10388=EDGE_CURVE('',#8214,#8215,#3591,.T.);
#10389=EDGE_CURVE('',#8215,#8216,#3592,.T.);
#10390=EDGE_CURVE('',#8216,#8199,#4470,.T.);
#10391=EDGE_CURVE('',#8179,#8182,#4471,.T.);
#10392=EDGE_CURVE('',#8197,#8217,#4472,.T.);
#10393=EDGE_CURVE('',#8217,#8200,#4473,.T.);
#10394=EDGE_CURVE('',#8217,#8218,#3593,.T.);
#10395=EDGE_CURVE('',#8199,#8218,#4474,.T.);
#10396=EDGE_CURVE('',#8218,#8219,#4475,.T.);
#10397=EDGE_CURVE('',#8216,#8219,#4476,.T.);
#10398=EDGE_CURVE('',#8219,#8220,#3594,.T.);
#10399=EDGE_CURVE('',#8215,#8220,#4477,.T.);
#10400=EDGE_CURVE('',#8220,#8221,#3595,.T.);
#10401=EDGE_CURVE('',#8214,#8221,#4478,.T.);
#10402=EDGE_CURVE('',#8221,#8222,#3596,.T.);
#10403=EDGE_CURVE('',#8213,#8222,#4479,.T.);
#10404=EDGE_CURVE('',#8222,#8223,#4480,.T.);
#10405=EDGE_CURVE('',#8212,#8223,#4481,.T.);
#10406=EDGE_CURVE('',#8223,#8224,#3597,.T.);
#10407=EDGE_CURVE('',#8211,#8224,#4482,.T.);
#10408=EDGE_CURVE('',#8224,#8225,#3598,.T.);
#10409=EDGE_CURVE('',#8210,#8225,#4483,.T.);
#10410=EDGE_CURVE('',#8225,#8226,#3599,.T.);
#10411=EDGE_CURVE('',#8209,#8226,#4484,.T.);
#10412=EDGE_CURVE('',#8226,#8227,#4485,.T.);
#10413=EDGE_CURVE('',#8208,#8227,#4486,.T.);
#10414=EDGE_CURVE('',#8227,#8228,#4487,.T.);
#10415=EDGE_CURVE('',#8207,#8228,#4488,.T.);
#10416=EDGE_CURVE('',#8228,#8229,#4489,.T.);
#10417=EDGE_CURVE('',#8206,#8229,#4490,.T.);
#10418=EDGE_CURVE('',#8229,#8230,#3600,.T.);
#10419=EDGE_CURVE('',#8205,#8230,#4491,.T.);
#10420=EDGE_CURVE('',#8230,#8231,#3601,.T.);
#10421=EDGE_CURVE('',#8204,#8231,#4492,.T.);
#10422=EDGE_CURVE('',#8231,#8232,#3602,.T.);
#10423=EDGE_CURVE('',#8203,#8232,#4493,.T.);
#10424=EDGE_CURVE('',#8232,#8233,#4494,.T.);
#10425=EDGE_CURVE('',#8202,#8233,#4495,.T.);
#10426=EDGE_CURVE('',#8233,#8234,#3603,.T.);
#10427=EDGE_CURVE('',#8201,#8234,#4496,.T.);
#10428=EDGE_CURVE('',#8234,#8163,#3604,.T.);
#10429=EDGE_CURVE('',#8235,#8235,#3605,.T.);
#10430=EDGE_CURVE('',#8235,#8236,#4497,.T.);
#10431=EDGE_CURVE('',#8236,#8236,#3606,.T.);
#10432=EDGE_CURVE('',#8237,#8237,#3607,.T.);
#10433=EDGE_CURVE('',#8237,#8235,#3608,.T.);
#10434=EDGE_CURVE('',#8238,#8238,#3609,.T.);
#10435=EDGE_CURVE('',#8238,#8239,#3610,.T.);
#10436=EDGE_CURVE('',#8239,#8239,#3611,.T.);
#10437=EDGE_CURVE('',#8240,#8240,#3612,.T.);
#10438=EDGE_CURVE('',#8240,#8238,#4498,.T.);
#10439=EDGE_CURVE('',#8241,#8242,#3613,.T.);
#10440=EDGE_CURVE('',#8242,#8243,#3614,.T.);
#10441=EDGE_CURVE('',#8243,#8244,#3615,.T.);
#10442=EDGE_CURVE('',#8244,#8245,#3616,.T.);
#10443=EDGE_CURVE('',#8245,#8246,#3617,.T.);
#10444=EDGE_CURVE('',#8246,#8247,#3618,.T.);
#10445=EDGE_CURVE('',#8247,#8248,#3619,.T.);
#10446=EDGE_CURVE('',#8248,#8249,#3620,.T.);
#10447=EDGE_CURVE('',#8249,#8250,#3621,.T.);
#10448=EDGE_CURVE('',#8250,#8240,#3622,.T.);
#10449=EDGE_CURVE('',#8250,#8251,#3623,.T.);
#10450=EDGE_CURVE('',#8251,#8252,#3624,.T.);
#10451=EDGE_CURVE('',#8252,#8253,#3625,.T.);
#10452=EDGE_CURVE('',#8253,#8254,#3626,.T.);
#10453=EDGE_CURVE('',#8254,#8255,#3627,.T.);
#10454=EDGE_CURVE('',#8255,#8256,#3628,.T.);
#10455=EDGE_CURVE('',#8256,#8257,#3629,.T.);
#10456=EDGE_CURVE('',#8257,#8241,#3630,.T.);
#10457=EDGE_CURVE('',#8258,#8258,#3631,.T.);
#10458=EDGE_CURVE('',#8258,#8259,#4499,.T.);
#10459=EDGE_CURVE('',#8259,#8259,#3632,.T.);
#10460=EDGE_CURVE('',#8260,#8260,#3633,.T.);
#10461=EDGE_CURVE('',#8260,#8258,#3634,.T.);
#10462=EDGE_CURVE('',#8259,#8261,#3635,.T.);
#10463=EDGE_CURVE('',#8261,#8262,#3636,.T.);
#10464=EDGE_CURVE('',#8263,#8262,#3637,.T.);
#10465=EDGE_CURVE('',#8264,#8263,#3638,.T.);
#10466=EDGE_CURVE('',#8265,#8264,#3639,.T.);
#10467=EDGE_CURVE('',#8265,#8266,#3640,.T.);
#10468=EDGE_CURVE('',#8267,#8266,#3641,.T.);
#10469=EDGE_CURVE('',#8268,#8267,#3642,.T.);
#10470=EDGE_CURVE('',#8269,#8268,#3643,.T.);
#10471=EDGE_CURVE('',#8269,#8270,#3644,.T.);
#10472=EDGE_CURVE('',#8271,#8270,#3645,.T.);
#10473=EDGE_CURVE('',#8272,#8271,#3646,.T.);
#10474=EDGE_CURVE('',#8273,#8272,#3647,.T.);
#10475=EDGE_CURVE('',#8273,#8274,#3648,.T.);
#10476=EDGE_CURVE('',#8275,#8274,#3649,.T.);
#10477=EDGE_CURVE('',#8276,#8275,#3650,.T.);
#10478=EDGE_CURVE('',#8277,#8276,#3651,.T.);
#10479=EDGE_CURVE('',#8277,#8278,#3652,.T.);
#10480=EDGE_CURVE('',#8279,#8278,#3653,.T.);
#10481=EDGE_CURVE('',#8280,#8279,#3654,.T.);
#10482=EDGE_CURVE('',#8281,#8280,#3655,.T.);
#10483=EDGE_CURVE('',#8281,#8282,#3656,.T.);
#10484=EDGE_CURVE('',#8283,#8282,#3657,.T.);
#10485=EDGE_CURVE('',#8284,#8283,#3658,.T.);
#10486=EDGE_CURVE('',#8285,#8284,#3659,.T.);
#10487=EDGE_CURVE('',#8285,#8286,#3660,.T.);
#10488=EDGE_CURVE('',#8287,#8286,#3661,.T.);
#10489=EDGE_CURVE('',#8288,#8287,#3662,.T.);
#10490=EDGE_CURVE('',#8289,#8288,#3663,.T.);
#10491=EDGE_CURVE('',#8289,#8290,#3664,.T.);
#10492=EDGE_CURVE('',#8291,#8290,#3665,.T.);
#10493=EDGE_CURVE('',#8292,#8291,#3666,.T.);
#10494=EDGE_CURVE('',#8293,#8292,#3667,.T.);
#10495=EDGE_CURVE('',#8293,#8261,#3668,.T.);
#10496=EDGE_CURVE('',#8294,#8291,#4500,.T.);
#10497=EDGE_CURVE('',#8295,#8294,#3669,.T.);
#10498=EDGE_CURVE('',#8292,#8295,#4501,.T.);
#10499=EDGE_CURVE('',#8296,#8297,#3670,.T.);
#10500=EDGE_CURVE('',#8264,#8296,#4502,.T.);
#10501=EDGE_CURVE('',#8297,#8263,#4503,.T.);
#10502=EDGE_CURVE('',#8298,#8287,#4504,.T.);
#10503=EDGE_CURVE('',#8299,#8298,#3671,.T.);
#10504=EDGE_CURVE('',#8288,#8299,#4505,.T.);
#10505=EDGE_CURVE('',#8300,#8283,#4506,.T.);
#10506=EDGE_CURVE('',#8301,#8300,#3672,.T.);
#10507=EDGE_CURVE('',#8284,#8301,#4507,.T.);
#10508=EDGE_CURVE('',#8302,#8279,#4508,.T.);
#10509=EDGE_CURVE('',#8303,#8302,#3673,.T.);
#10510=EDGE_CURVE('',#8280,#8303,#4509,.T.);
#10511=EDGE_CURVE('',#8304,#8275,#4510,.T.);
#10512=EDGE_CURVE('',#8305,#8304,#3674,.T.);
#10513=EDGE_CURVE('',#8276,#8305,#4511,.T.);
#10514=EDGE_CURVE('',#8306,#8271,#4512,.T.);
#10515=EDGE_CURVE('',#8307,#8306,#3675,.T.);
#10516=EDGE_CURVE('',#8272,#8307,#4513,.T.);
#10517=EDGE_CURVE('',#8308,#8309,#3676,.T.);
#10518=EDGE_CURVE('',#8268,#8308,#4514,.T.);
#10519=EDGE_CURVE('',#8309,#8267,#4515,.T.);
#10520=EDGE_CURVE('',#8310,#8294,#4516,.T.);
#10521=EDGE_CURVE('',#8311,#8310,#3677,.T.);
#10522=EDGE_CURVE('',#8295,#8311,#4517,.T.);
#10523=EDGE_CURVE('',#8312,#8313,#3678,.T.);
#10524=EDGE_CURVE('',#8296,#8312,#4518,.T.);
#10525=EDGE_CURVE('',#8313,#8297,#4519,.T.);
#10526=EDGE_CURVE('',#8314,#8298,#4520,.T.);
#10527=EDGE_CURVE('',#8315,#8314,#3679,.T.);
#10528=EDGE_CURVE('',#8299,#8315,#4521,.T.);
#10529=EDGE_CURVE('',#8316,#8300,#4522,.T.);
#10530=EDGE_CURVE('',#8317,#8316,#3680,.T.);
#10531=EDGE_CURVE('',#8301,#8317,#4523,.T.);
#10532=EDGE_CURVE('',#8318,#8302,#4524,.T.);
#10533=EDGE_CURVE('',#8319,#8318,#3681,.T.);
#10534=EDGE_CURVE('',#8303,#8319,#4525,.T.);
#10535=EDGE_CURVE('',#8320,#8304,#4526,.T.);
#10536=EDGE_CURVE('',#8321,#8320,#3682,.T.);
#10537=EDGE_CURVE('',#8305,#8321,#4527,.T.);
#10538=EDGE_CURVE('',#8322,#8306,#4528,.T.);
#10539=EDGE_CURVE('',#8323,#8322,#3683,.T.);
#10540=EDGE_CURVE('',#8307,#8323,#4529,.T.);
#10541=EDGE_CURVE('',#8324,#8325,#3684,.T.);
#10542=EDGE_CURVE('',#8308,#8324,#4530,.T.);
#10543=EDGE_CURVE('',#8325,#8309,#4531,.T.);
#10544=EDGE_CURVE('',#8252,#8310,#4532,.T.);
#10545=EDGE_CURVE('',#8311,#8251,#4533,.T.);
#10546=EDGE_CURVE('',#8312,#8248,#4534,.T.);
#10547=EDGE_CURVE('',#8249,#8313,#4535,.T.);
#10548=EDGE_CURVE('',#8254,#8314,#4536,.T.);
#10549=EDGE_CURVE('',#8315,#8253,#4537,.T.);
#10550=EDGE_CURVE('',#8256,#8316,#4538,.T.);
#10551=EDGE_CURVE('',#8317,#8255,#4539,.T.);
#10552=EDGE_CURVE('',#8241,#8318,#4540,.T.);
#10553=EDGE_CURVE('',#8319,#8257,#4541,.T.);
#10554=EDGE_CURVE('',#8243,#8320,#4542,.T.);
#10555=EDGE_CURVE('',#8321,#8242,#4543,.T.);
#10556=EDGE_CURVE('',#8245,#8322,#4544,.T.);
#10557=EDGE_CURVE('',#8323,#8244,#4545,.T.);
#10558=EDGE_CURVE('',#8324,#8246,#4546,.T.);
#10559=EDGE_CURVE('',#8247,#8325,#4547,.T.);
#10560=EDGE_CURVE('',#8246,#8269,#4548,.T.);
#10561=EDGE_CURVE('',#8270,#8245,#4549,.T.);
#10562=EDGE_CURVE('',#8248,#8265,#4550,.T.);
#10563=EDGE_CURVE('',#8266,#8247,#4551,.T.);
#10564=EDGE_CURVE('',#8244,#8273,#4552,.T.);
#10565=EDGE_CURVE('',#8274,#8243,#4553,.T.);
#10566=EDGE_CURVE('',#8242,#8277,#4554,.T.);
#10567=EDGE_CURVE('',#8278,#8241,#4555,.T.);
#10568=EDGE_CURVE('',#8257,#8281,#4556,.T.);
#10569=EDGE_CURVE('',#8282,#8256,#4557,.T.);
#10570=EDGE_CURVE('',#8255,#8285,#4558,.T.);
#10571=EDGE_CURVE('',#8286,#8254,#4559,.T.);
#10572=EDGE_CURVE('',#8253,#8289,#4560,.T.);
#10573=EDGE_CURVE('',#8290,#8252,#4561,.T.);
#10574=EDGE_CURVE('',#8251,#8293,#4562,.T.);
#10575=EDGE_CURVE('',#8262,#8249,#4563,.T.);
#10576=EDGE_CURVE('',#8326,#8327,#3685,.T.);
#10577=EDGE_CURVE('',#8328,#8328,#3686,.T.);
#10578=EDGE_CURVE('',#8328,#8329,#3687,.T.);
#10579=EDGE_CURVE('',#8329,#8329,#3688,.T.);
#10580=EDGE_CURVE('',#8330,#8330,#3689,.T.);
#10581=EDGE_CURVE('',#8330,#8331,#3690,.T.);
#10582=EDGE_CURVE('',#8331,#8332,#3691,.T.);
#10583=EDGE_CURVE('',#8332,#8331,#3692,.T.);
#10584=EDGE_CURVE('',#8333,#8334,#3693,.T.);
#10585=EDGE_CURVE('',#8334,#8332,#4564,.T.);
#10586=EDGE_CURVE('',#8334,#8333,#3694,.T.);
#10587=EDGE_CURVE('',#8333,#8335,#4565,.T.);
#10588=EDGE_CURVE('',#8335,#8335,#3695,.T.);
#10589=EDGE_CURVE('',#8335,#8336,#4566,.T.);
#10590=EDGE_CURVE('',#8336,#8336,#3696,.T.);
#10591=EDGE_CURVE('',#8336,#8337,#3697,.T.);
#10592=EDGE_CURVE('',#8337,#8337,#3698,.T.);
#10593=EDGE_CURVE('',#8338,#8338,#3699,.T.);
#10594=EDGE_CURVE('',#8338,#8339,#3700,.T.);
#10595=EDGE_CURVE('',#8339,#8339,#3701,.T.);
#10596=EDGE_CURVE('',#8340,#8340,#3702,.T.);
#10597=EDGE_CURVE('',#8340,#8341,#3703,.T.);
#10598=EDGE_CURVE('',#8341,#8341,#3704,.T.);
#10599=EDGE_CURVE('',#8329,#8340,#4567,.T.);
#10600=EDGE_CURVE('',#8339,#8328,#4568,.T.);
#10601=EDGE_CURVE('',#8342,#8342,#3705,.T.);
#10602=EDGE_CURVE('',#8342,#8343,#3706,.T.);
#10603=EDGE_CURVE('',#8343,#8343,#3707,.T.);
#10604=EDGE_CURVE('',#8344,#8344,#3708,.T.);
#10605=EDGE_CURVE('',#8344,#8345,#4569,.T.);
#10606=EDGE_CURVE('',#8345,#8345,#3709,.T.);
#10607=EDGE_CURVE('',#8345,#8346,#3710,.T.);
#10608=EDGE_CURVE('',#8346,#8346,#3711,.T.);
#10609=EDGE_CURVE('',#8346,#8347,#4570,.T.);
#10610=EDGE_CURVE('',#8347,#8347,#3712,.T.);
#10611=EDGE_CURVE('',#8348,#8349,#3713,.T.);
#10612=EDGE_CURVE('',#8349,#8350,#4571,.T.);
#10613=EDGE_CURVE('',#8350,#8350,#3714,.T.);
#10614=EDGE_CURVE('',#8349,#8348,#3715,.T.);
#10615=EDGE_CURVE('',#8348,#8344,#3716,.T.);
#10616=EDGE_CURVE('',#8351,#8351,#3717,.T.);
#10617=EDGE_CURVE('',#8351,#8342,#4572,.T.);
#10618=EDGE_CURVE('',#8343,#8352,#4573,.T.);
#10619=EDGE_CURVE('',#8352,#8352,#3718,.T.);
#10620=EDGE_CURVE('',#8353,#8354,#3719,.T.);
#10621=EDGE_CURVE('',#8355,#8356,#3720,.T.);
#10622=EDGE_CURVE('',#8357,#8358,#3721,.T.);
#10623=EDGE_CURVE('',#8359,#8360,#3722,.T.);
#10624=EDGE_CURVE('',#8361,#8362,#3723,.T.);
#10625=EDGE_CURVE('',#8363,#8364,#3724,.T.);
#10626=EDGE_CURVE('',#8365,#8366,#3725,.T.);
#10627=EDGE_CURVE('',#8367,#8368,#3726,.T.);
#10628=EDGE_CURVE('',#8368,#8367,#3727,.T.);
#10629=EDGE_CURVE('',#8368,#8369,#3728,.T.);
#10630=EDGE_CURVE('',#8370,#8369,#3729,.T.);
#10631=EDGE_CURVE('',#8369,#8370,#3730,.T.);
#10632=EDGE_CURVE('',#8371,#8371,#3731,.T.);
#10633=EDGE_CURVE('',#8371,#8372,#4574,.T.);
#10634=EDGE_CURVE('',#8372,#8372,#3732,.T.);
#10635=EDGE_CURVE('',#8373,#8373,#3733,.T.);
#10636=EDGE_CURVE('',#8373,#8371,#3734,.T.);
#10637=EDGE_CURVE('',#8374,#8374,#3735,.T.);
#10638=EDGE_CURVE('',#8374,#8375,#3736,.T.);
#10639=EDGE_CURVE('',#8375,#8375,#3737,.T.);
#10640=EDGE_CURVE('',#8376,#8376,#3738,.T.);
#10641=EDGE_CURVE('',#8376,#8374,#4575,.T.);
#10642=EDGE_CURVE('',#8377,#8378,#3739,.T.);
#10643=EDGE_CURVE('',#8379,#8377,#3740,.T.);
#10644=EDGE_CURVE('',#8380,#8379,#3741,.T.);
#10645=EDGE_CURVE('',#8381,#8380,#3742,.T.);
#10646=EDGE_CURVE('',#8382,#8381,#3743,.T.);
#10647=EDGE_CURVE('',#8383,#8382,#3744,.T.);
#10648=EDGE_CURVE('',#8384,#8383,#3745,.T.);
#10649=EDGE_CURVE('',#8385,#8384,#3746,.T.);
#10650=EDGE_CURVE('',#8386,#8385,#3747,.T.);
#10651=EDGE_CURVE('',#8386,#8376,#3748,.T.);
#10652=EDGE_CURVE('',#8387,#8386,#3749,.T.);
#10653=EDGE_CURVE('',#8388,#8387,#3750,.T.);
#10654=EDGE_CURVE('',#8389,#8388,#3751,.T.);
#10655=EDGE_CURVE('',#8390,#8389,#3752,.T.);
#10656=EDGE_CURVE('',#8391,#8390,#3753,.T.);
#10657=EDGE_CURVE('',#8392,#8391,#3754,.T.);
#10658=EDGE_CURVE('',#8393,#8392,#3755,.T.);
#10659=EDGE_CURVE('',#8378,#8393,#3756,.T.);
#10660=EDGE_CURVE('',#8394,#8394,#3757,.T.);
#10661=EDGE_CURVE('',#8394,#8395,#3758,.T.);
#10662=EDGE_CURVE('',#8395,#8395,#3759,.T.);
#10663=EDGE_CURVE('',#8395,#8370,#4576,.T.);
#10664=EDGE_CURVE('',#8367,#8396,#3760,.T.);
#10665=EDGE_CURVE('',#8397,#8396,#3761,.T.);
#10666=EDGE_CURVE('',#8397,#8398,#3762,.T.);
#10667=EDGE_CURVE('',#8398,#8399,#3763,.T.);
#10668=EDGE_CURVE('',#8399,#8400,#3764,.T.);
#10669=EDGE_CURVE('',#8401,#8400,#3765,.T.);
#10670=EDGE_CURVE('',#8401,#8402,#3766,.T.);
#10671=EDGE_CURVE('',#8402,#8403,#3767,.T.);
#10672=EDGE_CURVE('',#8403,#8404,#3768,.T.);
#10673=EDGE_CURVE('',#8405,#8404,#3769,.T.);
#10674=EDGE_CURVE('',#8405,#8406,#3770,.T.);
#10675=EDGE_CURVE('',#8406,#8407,#3771,.T.);
#10676=EDGE_CURVE('',#8407,#8408,#3772,.T.);
#10677=EDGE_CURVE('',#8409,#8408,#3773,.T.);
#10678=EDGE_CURVE('',#8409,#8410,#3774,.T.);
#10679=EDGE_CURVE('',#8410,#8411,#3775,.T.);
#10680=EDGE_CURVE('',#8411,#8412,#3776,.T.);
#10681=EDGE_CURVE('',#8413,#8412,#3777,.T.);
#10682=EDGE_CURVE('',#8413,#8414,#3778,.T.);
#10683=EDGE_CURVE('',#8414,#8415,#3779,.T.);
#10684=EDGE_CURVE('',#8415,#8416,#3780,.T.);
#10685=EDGE_CURVE('',#8417,#8416,#3781,.T.);
#10686=EDGE_CURVE('',#8417,#8418,#3782,.T.);
#10687=EDGE_CURVE('',#8418,#8419,#3783,.T.);
#10688=EDGE_CURVE('',#8419,#8420,#3784,.T.);
#10689=EDGE_CURVE('',#8421,#8420,#3785,.T.);
#10690=EDGE_CURVE('',#8421,#8422,#3786,.T.);
#10691=EDGE_CURVE('',#8422,#8423,#3787,.T.);
#10692=EDGE_CURVE('',#8423,#8424,#3788,.T.);
#10693=EDGE_CURVE('',#8425,#8424,#3789,.T.);
#10694=EDGE_CURVE('',#8425,#8426,#3790,.T.);
#10695=EDGE_CURVE('',#8426,#8427,#3791,.T.);
#10696=EDGE_CURVE('',#8427,#8428,#3792,.T.);
#10697=EDGE_CURVE('',#8396,#8428,#3793,.T.);
#10698=EDGE_CURVE('',#8398,#8429,#4577,.T.);
#10699=EDGE_CURVE('',#8429,#8430,#3794,.T.);
#10700=EDGE_CURVE('',#8430,#8399,#4578,.T.);
#10701=EDGE_CURVE('',#8431,#8432,#3795,.T.);
#10702=EDGE_CURVE('',#8432,#8427,#4579,.T.);
#10703=EDGE_CURVE('',#8426,#8431,#4580,.T.);
#10704=EDGE_CURVE('',#8402,#8433,#4581,.T.);
#10705=EDGE_CURVE('',#8433,#8434,#3796,.T.);
#10706=EDGE_CURVE('',#8434,#8403,#4582,.T.);
#10707=EDGE_CURVE('',#8406,#8435,#4583,.T.);
#10708=EDGE_CURVE('',#8435,#8436,#3797,.T.);
#10709=EDGE_CURVE('',#8436,#8407,#4584,.T.);
#10710=EDGE_CURVE('',#8410,#8437,#4585,.T.);
#10711=EDGE_CURVE('',#8437,#8438,#3798,.T.);
#10712=EDGE_CURVE('',#8438,#8411,#4586,.T.);
#10713=EDGE_CURVE('',#8414,#8439,#4587,.T.);
#10714=EDGE_CURVE('',#8439,#8440,#3799,.T.);
#10715=EDGE_CURVE('',#8440,#8415,#4588,.T.);
#10716=EDGE_CURVE('',#8418,#8441,#4589,.T.);
#10717=EDGE_CURVE('',#8441,#8442,#3800,.T.);
#10718=EDGE_CURVE('',#8442,#8419,#4590,.T.);
#10719=EDGE_CURVE('',#8443,#8444,#3801,.T.);
#10720=EDGE_CURVE('',#8444,#8423,#4591,.T.);
#10721=EDGE_CURVE('',#8422,#8443,#4592,.T.);
#10722=EDGE_CURVE('',#8429,#8445,#4593,.T.);
#10723=EDGE_CURVE('',#8445,#8446,#3802,.T.);
#10724=EDGE_CURVE('',#8446,#8430,#4594,.T.);
#10725=EDGE_CURVE('',#8447,#8448,#3803,.T.);
#10726=EDGE_CURVE('',#8448,#8432,#4595,.T.);
#10727=EDGE_CURVE('',#8431,#8447,#4596,.T.);
#10728=EDGE_CURVE('',#8433,#8449,#4597,.T.);
#10729=EDGE_CURVE('',#8449,#8450,#3804,.T.);
#10730=EDGE_CURVE('',#8450,#8434,#4598,.T.);
#10731=EDGE_CURVE('',#8435,#8451,#4599,.T.);
#10732=EDGE_CURVE('',#8451,#8452,#3805,.T.);
#10733=EDGE_CURVE('',#8452,#8436,#4600,.T.);
#10734=EDGE_CURVE('',#8437,#8453,#4601,.T.);
#10735=EDGE_CURVE('',#8453,#8454,#3806,.T.);
#10736=EDGE_CURVE('',#8454,#8438,#4602,.T.);
#10737=EDGE_CURVE('',#8439,#8455,#4603,.T.);
#10738=EDGE_CURVE('',#8455,#8456,#3807,.T.);
#10739=EDGE_CURVE('',#8456,#8440,#4604,.T.);
#10740=EDGE_CURVE('',#8441,#8457,#4605,.T.);
#10741=EDGE_CURVE('',#8457,#8458,#3808,.T.);
#10742=EDGE_CURVE('',#8458,#8442,#4606,.T.);
#10743=EDGE_CURVE('',#8459,#8460,#3809,.T.);
#10744=EDGE_CURVE('',#8460,#8444,#4607,.T.);
#10745=EDGE_CURVE('',#8443,#8459,#4608,.T.);
#10746=EDGE_CURVE('',#8445,#8385,#4609,.T.);
#10747=EDGE_CURVE('',#8384,#8446,#4610,.T.);
#10748=EDGE_CURVE('',#8387,#8448,#4611,.T.);
#10749=EDGE_CURVE('',#8447,#8388,#4612,.T.);
#10750=EDGE_CURVE('',#8449,#8383,#4613,.T.);
#10751=EDGE_CURVE('',#8382,#8450,#4614,.T.);
#10752=EDGE_CURVE('',#8451,#8381,#4615,.T.);
#10753=EDGE_CURVE('',#8380,#8452,#4616,.T.);
#10754=EDGE_CURVE('',#8453,#8379,#4617,.T.);
#10755=EDGE_CURVE('',#8377,#8454,#4618,.T.);
#10756=EDGE_CURVE('',#8455,#8378,#4619,.T.);
#10757=EDGE_CURVE('',#8393,#8456,#4620,.T.);
#10758=EDGE_CURVE('',#8457,#8392,#4621,.T.);
#10759=EDGE_CURVE('',#8391,#8458,#4622,.T.);
#10760=EDGE_CURVE('',#8389,#8460,#4623,.T.);
#10761=EDGE_CURVE('',#8459,#8390,#4624,.T.);
#10762=EDGE_CURVE('',#8390,#8421,#4625,.T.);
#10763=EDGE_CURVE('',#8420,#8391,#4626,.T.);
#10764=EDGE_CURVE('',#8388,#8425,#4627,.T.);
#10765=EDGE_CURVE('',#8424,#8389,#4628,.T.);
#10766=EDGE_CURVE('',#8392,#8417,#4629,.T.);
#10767=EDGE_CURVE('',#8416,#8393,#4630,.T.);
#10768=EDGE_CURVE('',#8378,#8413,#4631,.T.);
#10769=EDGE_CURVE('',#8412,#8377,#4632,.T.);
#10770=EDGE_CURVE('',#8379,#8409,#4633,.T.);
#10771=EDGE_CURVE('',#8408,#8380,#4634,.T.);
#10772=EDGE_CURVE('',#8381,#8405,#4635,.T.);
#10773=EDGE_CURVE('',#8404,#8382,#4636,.T.);
#10774=EDGE_CURVE('',#8383,#8401,#4637,.T.);
#10775=EDGE_CURVE('',#8400,#8384,#4638,.T.);
#10776=EDGE_CURVE('',#8385,#8397,#4639,.T.);
#10777=EDGE_CURVE('',#8428,#8387,#4640,.T.);
#10778=EDGE_CURVE('',#8461,#8462,#4641,.T.);
#10779=EDGE_CURVE('',#8462,#8463,#4642,.T.);
#10780=EDGE_CURVE('',#8464,#8463,#4643,.T.);
#10781=EDGE_CURVE('',#8461,#8464,#4644,.T.);
#10782=EDGE_CURVE('',#8462,#8465,#4645,.T.);
#10783=EDGE_CURVE('',#8465,#8466,#4646,.T.);
#10784=EDGE_CURVE('',#8463,#8466,#4647,.T.);
#10785=EDGE_CURVE('',#8465,#8467,#4648,.T.);
#10786=EDGE_CURVE('',#8467,#8468,#4649,.T.);
#10787=EDGE_CURVE('',#8466,#8468,#4650,.T.);
#10788=EDGE_CURVE('',#8469,#8470,#4651,.T.);
#10789=EDGE_CURVE('',#8470,#8471,#4652,.T.);
#10790=EDGE_CURVE('',#8472,#8471,#4653,.T.);
#10791=EDGE_CURVE('',#8469,#8472,#4654,.T.);
#10792=EDGE_CURVE('',#8473,#8469,#4655,.T.);
#10793=EDGE_CURVE('',#8474,#8472,#4656,.T.);
#10794=EDGE_CURVE('',#8473,#8474,#4657,.T.);
#10795=EDGE_CURVE('',#8475,#8473,#4658,.T.);
#10796=EDGE_CURVE('',#8476,#8474,#4659,.T.);
#10797=EDGE_CURVE('',#8475,#8476,#4660,.T.);
#10798=EDGE_CURVE('',#8477,#8475,#4661,.T.);
#10799=EDGE_CURVE('',#8478,#8476,#4662,.T.);
#10800=EDGE_CURVE('',#8477,#8478,#4663,.T.);
#10801=EDGE_CURVE('',#8479,#8477,#4664,.T.);
#10802=EDGE_CURVE('',#8480,#8478,#4665,.T.);
#10803=EDGE_CURVE('',#8479,#8480,#4666,.T.);
#10804=EDGE_CURVE('',#8481,#8479,#4667,.T.);
#10805=EDGE_CURVE('',#8482,#8480,#4668,.T.);
#10806=EDGE_CURVE('',#8481,#8482,#4669,.T.);
#10807=EDGE_CURVE('',#8483,#8484,#4670,.T.);
#10808=EDGE_CURVE('',#8483,#8485,#4671,.T.);
#10809=EDGE_CURVE('',#8485,#8486,#4672,.T.);
#10810=EDGE_CURVE('',#8484,#8486,#4673,.T.);
#10811=EDGE_CURVE('',#8484,#8487,#4674,.T.);
#10812=EDGE_CURVE('',#8486,#8488,#4675,.T.);
#10813=EDGE_CURVE('',#8487,#8488,#4676,.T.);
#10814=EDGE_CURVE('',#8487,#8489,#4677,.T.);
#10815=EDGE_CURVE('',#8488,#8490,#4678,.T.);
#10816=EDGE_CURVE('',#8489,#8490,#4679,.T.);
#10817=EDGE_CURVE('',#8481,#8491,#4680,.T.);
#10818=EDGE_CURVE('',#8492,#8482,#4681,.T.);
#10819=EDGE_CURVE('',#8491,#8492,#4682,.T.);
#10820=EDGE_CURVE('',#8493,#8494,#4683,.T.);
#10821=EDGE_CURVE('',#8493,#8495,#4684,.T.);
#10822=EDGE_CURVE('',#8495,#8496,#4685,.T.);
#10823=EDGE_CURVE('',#8494,#8496,#4686,.T.);
#10824=EDGE_CURVE('',#8497,#8493,#4687,.T.);
#10825=EDGE_CURVE('',#8497,#8498,#4688,.T.);
#10826=EDGE_CURVE('',#8498,#8495,#4689,.T.);
#10827=EDGE_CURVE('',#8499,#8497,#4690,.T.);
#10828=EDGE_CURVE('',#8499,#8500,#4691,.T.);
#10829=EDGE_CURVE('',#8500,#8498,#4692,.T.);
#10830=EDGE_CURVE('',#8501,#8499,#4693,.T.);
#10831=EDGE_CURVE('',#8501,#8502,#4694,.T.);
#10832=EDGE_CURVE('',#8502,#8500,#4695,.T.);
#10833=EDGE_CURVE('',#8503,#8501,#4696,.T.);
#10834=EDGE_CURVE('',#8503,#8504,#4697,.T.);
#10835=EDGE_CURVE('',#8504,#8502,#4698,.T.);
#10836=EDGE_CURVE('',#8491,#8503,#4699,.T.);
#10837=EDGE_CURVE('',#8492,#8504,#4700,.T.);
#10838=EDGE_CURVE('',#8505,#8506,#4701,.T.);
#10839=EDGE_CURVE('',#8505,#8507,#4702,.T.);
#10840=EDGE_CURVE('',#8507,#8508,#4703,.T.);
#10841=EDGE_CURVE('',#8506,#8508,#4704,.T.);
#10842=EDGE_CURVE('',#8506,#8509,#4705,.T.);
#10843=EDGE_CURVE('',#8508,#8510,#4706,.T.);
#10844=EDGE_CURVE('',#8509,#8510,#4707,.T.);
#10845=EDGE_CURVE('',#8509,#8511,#4708,.T.);
#10846=EDGE_CURVE('',#8510,#8512,#4709,.T.);
#10847=EDGE_CURVE('',#8511,#8512,#4710,.T.);
#10848=EDGE_CURVE('',#8467,#8511,#4711,.T.);
#10849=EDGE_CURVE('',#8512,#8468,#4712,.T.);
#10850=EDGE_CURVE('',#8513,#8514,#4713,.T.);
#10851=EDGE_CURVE('',#8513,#8515,#4714,.T.);
#10852=EDGE_CURVE('',#8515,#8516,#4715,.T.);
#10853=EDGE_CURVE('',#8514,#8516,#4716,.T.);
#10854=EDGE_CURVE('',#8517,#8513,#4717,.T.);
#10855=EDGE_CURVE('',#8517,#8518,#4718,.T.);
#10856=EDGE_CURVE('',#8518,#8515,#4719,.T.);
#10857=EDGE_CURVE('',#8519,#8517,#4720,.T.);
#10858=EDGE_CURVE('',#8519,#8520,#4721,.T.);
#10859=EDGE_CURVE('',#8520,#8518,#4722,.T.);
#10860=EDGE_CURVE('',#8521,#8519,#4723,.T.);
#10861=EDGE_CURVE('',#8521,#8522,#4724,.T.);
#10862=EDGE_CURVE('',#8522,#8520,#4725,.T.);
#10863=EDGE_CURVE('',#8523,#8521,#4726,.T.);
#10864=EDGE_CURVE('',#8523,#8524,#4727,.T.);
#10865=EDGE_CURVE('',#8524,#8522,#4728,.T.);
#10866=EDGE_CURVE('',#8525,#8523,#4729,.T.);
#10867=EDGE_CURVE('',#8525,#8526,#4730,.T.);
#10868=EDGE_CURVE('',#8526,#8524,#4731,.T.);
#10869=EDGE_CURVE('',#8527,#8528,#4732,.T.);
#10870=EDGE_CURVE('',#8528,#8529,#4733,.T.);
#10871=EDGE_CURVE('',#8530,#8529,#4734,.T.);
#10872=EDGE_CURVE('',#8527,#8530,#4735,.T.);
#10873=EDGE_CURVE('',#8528,#8531,#4736,.T.);
#10874=EDGE_CURVE('',#8531,#8532,#4737,.T.);
#10875=EDGE_CURVE('',#8529,#8532,#4738,.T.);
#10876=EDGE_CURVE('',#8531,#8533,#4739,.T.);
#10877=EDGE_CURVE('',#8533,#8534,#4740,.T.);
#10878=EDGE_CURVE('',#8532,#8534,#4741,.T.);
#10879=EDGE_CURVE('',#8489,#8533,#4742,.T.);
#10880=EDGE_CURVE('',#8534,#8490,#4743,.T.);
#10881=EDGE_CURVE('',#8535,#8535,#3810,.T.);
#10882=EDGE_CURVE('',#8535,#8536,#4744,.T.);
#10883=EDGE_CURVE('',#8536,#8536,#3811,.T.);
#10884=EDGE_CURVE('',#8525,#8537,#4745,.T.);
#10885=EDGE_CURVE('',#8537,#8538,#4746,.T.);
#10886=EDGE_CURVE('',#8538,#8526,#4747,.T.);
#10887=EDGE_CURVE('',#8539,#8540,#4748,.T.);
#10888=EDGE_CURVE('',#8540,#8541,#4749,.T.);
#10889=EDGE_CURVE('',#8542,#8541,#4750,.T.);
#10890=EDGE_CURVE('',#8539,#8542,#4751,.T.);
#10891=EDGE_CURVE('',#8543,#8539,#4752,.T.);
#10892=EDGE_CURVE('',#8544,#8542,#4753,.T.);
#10893=EDGE_CURVE('',#8543,#8544,#4754,.T.);
#10894=EDGE_CURVE('',#8545,#8543,#4755,.T.);
#10895=EDGE_CURVE('',#8546,#8544,#4756,.T.);
#10896=EDGE_CURVE('',#8545,#8546,#4757,.T.);
#10897=EDGE_CURVE('',#8547,#8545,#4758,.T.);
#10898=EDGE_CURVE('',#8548,#8546,#4759,.T.);
#10899=EDGE_CURVE('',#8547,#8548,#4760,.T.);
#10900=EDGE_CURVE('',#8549,#8547,#4761,.T.);
#10901=EDGE_CURVE('',#8550,#8548,#4762,.T.);
#10902=EDGE_CURVE('',#8549,#8550,#4763,.T.);
#10903=EDGE_CURVE('',#8537,#8549,#4764,.T.);
#10904=EDGE_CURVE('',#8538,#8550,#4765,.T.);
#10905=EDGE_CURVE('',#8551,#8552,#4766,.T.);
#10906=EDGE_CURVE('',#8551,#8553,#4767,.T.);
#10907=EDGE_CURVE('',#8553,#8554,#4768,.T.);
#10908=EDGE_CURVE('',#8552,#8554,#4769,.T.);
#10909=EDGE_CURVE('',#8552,#8555,#3812,.T.);
#10910=EDGE_CURVE('',#8554,#8556,#3813,.T.);
#10911=EDGE_CURVE('',#8555,#8556,#4770,.T.);
#10912=EDGE_CURVE('',#8555,#8557,#4771,.T.);
#10913=EDGE_CURVE('',#8556,#8558,#4772,.T.);
#10914=EDGE_CURVE('',#8557,#8558,#4773,.T.);
#10915=EDGE_CURVE('',#8557,#8559,#3814,.T.);
#10916=EDGE_CURVE('',#8558,#8560,#3815,.T.);
#10917=EDGE_CURVE('',#8559,#8560,#4774,.T.);
#10918=EDGE_CURVE('',#8561,#8562,#4775,.T.);
#10919=EDGE_CURVE('',#8561,#8563,#4776,.T.);
#10920=EDGE_CURVE('',#8563,#8564,#4777,.T.);
#10921=EDGE_CURVE('',#8562,#8564,#4778,.T.);
#10922=EDGE_CURVE('',#8562,#8565,#4779,.T.);
#10923=EDGE_CURVE('',#8564,#8566,#4780,.T.);
#10924=EDGE_CURVE('',#8565,#8566,#4781,.T.);
#10925=EDGE_CURVE('',#8565,#8567,#4782,.T.);
#10926=EDGE_CURVE('',#8566,#8568,#4783,.T.);
#10927=EDGE_CURVE('',#8567,#8568,#4784,.T.);
#10928=EDGE_CURVE('',#8567,#8569,#4785,.T.);
#10929=EDGE_CURVE('',#8568,#8570,#4786,.T.);
#10930=EDGE_CURVE('',#8569,#8570,#4787,.T.);
#10931=EDGE_CURVE('',#8569,#8571,#4788,.T.);
#10932=EDGE_CURVE('',#8570,#8572,#4789,.T.);
#10933=EDGE_CURVE('',#8571,#8572,#4790,.T.);
#10934=EDGE_CURVE('',#8571,#8573,#4791,.T.);
#10935=EDGE_CURVE('',#8572,#8574,#4792,.T.);
#10936=EDGE_CURVE('',#8573,#8574,#4793,.T.);
#10937=EDGE_CURVE('',#8540,#8573,#4794,.T.);
#10938=EDGE_CURVE('',#8574,#8541,#4795,.T.);
#10939=EDGE_CURVE('',#8527,#8575,#4796,.T.);
#10940=EDGE_CURVE('',#8576,#8530,#4797,.T.);
#10941=EDGE_CURVE('',#8575,#8576,#4798,.T.);
#10942=EDGE_CURVE('',#8575,#8577,#4799,.T.);
#10943=EDGE_CURVE('',#8576,#8578,#4800,.T.);
#10944=EDGE_CURVE('',#8577,#8578,#4801,.T.);
#10945=EDGE_CURVE('',#8577,#8579,#4802,.T.);
#10946=EDGE_CURVE('',#8578,#8580,#4803,.T.);
#10947=EDGE_CURVE('',#8579,#8580,#4804,.T.);
#10948=EDGE_CURVE('',#8579,#8581,#4805,.T.);
#10949=EDGE_CURVE('',#8580,#8582,#4806,.T.);
#10950=EDGE_CURVE('',#8581,#8582,#4807,.T.);
#10951=EDGE_CURVE('',#8583,#8551,#3816,.T.);
#10952=EDGE_CURVE('',#8583,#8584,#4808,.T.);
#10953=EDGE_CURVE('',#8584,#8553,#3817,.T.);
#10954=EDGE_CURVE('',#8585,#8583,#4809,.T.);
#10955=EDGE_CURVE('',#8585,#8586,#4810,.T.);
#10956=EDGE_CURVE('',#8586,#8584,#4811,.T.);
#10957=EDGE_CURVE('',#8587,#8585,#3818,.T.);
#10958=EDGE_CURVE('',#8587,#8588,#4812,.T.);
#10959=EDGE_CURVE('',#8588,#8586,#3819,.T.);
#10960=EDGE_CURVE('',#8559,#8587,#4813,.T.);
#10961=EDGE_CURVE('',#8560,#8588,#4814,.T.);
#10962=EDGE_CURVE('',#8589,#8561,#4815,.T.);
#10963=EDGE_CURVE('',#8589,#8590,#4816,.T.);
#10964=EDGE_CURVE('',#8590,#8563,#4817,.T.);
#10965=EDGE_CURVE('',#8591,#8589,#4818,.T.);
#10966=EDGE_CURVE('',#8591,#8592,#4819,.T.);
#10967=EDGE_CURVE('',#8592,#8590,#4820,.T.);
#10968=EDGE_CURVE('',#8593,#8591,#4821,.T.);
#10969=EDGE_CURVE('',#8593,#8594,#4822,.T.);
#10970=EDGE_CURVE('',#8594,#8592,#4823,.T.);
#10971=EDGE_CURVE('',#8595,#8593,#4824,.T.);
#10972=EDGE_CURVE('',#8595,#8596,#4825,.T.);
#10973=EDGE_CURVE('',#8596,#8594,#4826,.T.);
#10974=EDGE_CURVE('',#8597,#8595,#4827,.T.);
#10975=EDGE_CURVE('',#8597,#8598,#4828,.T.);
#10976=EDGE_CURVE('',#8598,#8596,#4829,.T.);
#10977=EDGE_CURVE('',#8599,#8597,#4830,.T.);
#10978=EDGE_CURVE('',#8599,#8600,#4831,.T.);
#10979=EDGE_CURVE('',#8600,#8598,#4832,.T.);
#10980=EDGE_CURVE('',#8601,#8599,#4833,.T.);
#10981=EDGE_CURVE('',#8601,#8602,#4834,.T.);
#10982=EDGE_CURVE('',#8602,#8600,#4835,.T.);
#10983=EDGE_CURVE('',#8603,#8601,#4836,.T.);
#10984=EDGE_CURVE('',#8603,#8604,#4837,.T.);
#10985=EDGE_CURVE('',#8604,#8602,#4838,.T.);
#10986=EDGE_CURVE('',#8605,#8603,#3820,.T.);
#10987=EDGE_CURVE('',#8605,#8606,#4839,.T.);
#10988=EDGE_CURVE('',#8606,#8604,#3821,.T.);
#10989=EDGE_CURVE('',#8607,#8605,#4840,.T.);
#10990=EDGE_CURVE('',#8607,#8608,#4841,.T.);
#10991=EDGE_CURVE('',#8608,#8606,#4842,.T.);
#10992=EDGE_CURVE('',#8609,#8607,#4843,.T.);
#10993=EDGE_CURVE('',#8609,#8610,#4844,.T.);
#10994=EDGE_CURVE('',#8610,#8608,#4845,.T.);
#10995=EDGE_CURVE('',#8611,#8609,#4846,.T.);
#10996=EDGE_CURVE('',#8611,#8612,#4847,.T.);
#10997=EDGE_CURVE('',#8612,#8610,#4848,.T.);
#10998=EDGE_CURVE('',#8613,#8611,#4849,.T.);
#10999=EDGE_CURVE('',#8613,#8614,#4850,.T.);
#11000=EDGE_CURVE('',#8614,#8612,#4851,.T.);
#11001=EDGE_CURVE('',#8615,#8613,#4852,.T.);
#11002=EDGE_CURVE('',#8615,#8616,#4853,.T.);
#11003=EDGE_CURVE('',#8616,#8614,#4854,.T.);
#11004=EDGE_CURVE('',#8617,#8615,#4855,.T.);
#11005=EDGE_CURVE('',#8617,#8618,#4856,.T.);
#11006=EDGE_CURVE('',#8618,#8616,#4857,.T.);
#11007=EDGE_CURVE('',#8619,#8617,#4858,.T.);
#11008=EDGE_CURVE('',#8619,#8620,#4859,.T.);
#11009=EDGE_CURVE('',#8620,#8618,#4860,.T.);
#11010=EDGE_CURVE('',#8621,#8622,#4861,.T.);
#11011=EDGE_CURVE('',#8622,#8623,#4862,.T.);
#11012=EDGE_CURVE('',#8624,#8623,#4863,.T.);
#11013=EDGE_CURVE('',#8621,#8624,#4864,.T.);
#11014=EDGE_CURVE('',#8622,#8625,#3822,.T.);
#11015=EDGE_CURVE('',#8625,#8626,#4865,.T.);
#11016=EDGE_CURVE('',#8623,#8626,#3823,.T.);
#11017=EDGE_CURVE('',#8625,#8627,#4866,.T.);
#11018=EDGE_CURVE('',#8627,#8628,#4867,.T.);
#11019=EDGE_CURVE('',#8626,#8628,#4868,.T.);
#11020=EDGE_CURVE('',#8627,#8629,#3824,.T.);
#11021=EDGE_CURVE('',#8629,#8630,#4869,.T.);
#11022=EDGE_CURVE('',#8628,#8630,#3825,.T.);
#11023=EDGE_CURVE('',#8631,#8632,#4870,.T.);
#11024=EDGE_CURVE('',#8632,#8633,#4871,.T.);
#11025=EDGE_CURVE('',#8634,#8633,#4872,.T.);
#11026=EDGE_CURVE('',#8631,#8634,#4873,.T.);
#11027=EDGE_CURVE('',#8632,#8635,#4874,.T.);
#11028=EDGE_CURVE('',#8635,#8636,#4875,.T.);
#11029=EDGE_CURVE('',#8633,#8636,#4876,.T.);
#11030=EDGE_CURVE('',#8635,#8637,#4877,.T.);
#11031=EDGE_CURVE('',#8637,#8638,#4878,.T.);
#11032=EDGE_CURVE('',#8636,#8638,#4879,.T.);
#11033=EDGE_CURVE('',#8637,#8639,#4880,.T.);
#11034=EDGE_CURVE('',#8639,#8640,#4881,.T.);
#11035=EDGE_CURVE('',#8638,#8640,#4882,.T.);
#11036=EDGE_CURVE('',#8639,#8641,#4883,.T.);
#11037=EDGE_CURVE('',#8641,#8642,#4884,.T.);
#11038=EDGE_CURVE('',#8640,#8642,#4885,.T.);
#11039=EDGE_CURVE('',#8641,#8643,#4886,.T.);
#11040=EDGE_CURVE('',#8643,#8644,#4887,.T.);
#11041=EDGE_CURVE('',#8642,#8644,#4888,.T.);
#11042=EDGE_CURVE('',#8494,#8643,#4889,.T.);
#11043=EDGE_CURVE('',#8644,#8496,#4890,.T.);
#11044=EDGE_CURVE('',#8483,#8645,#4891,.T.);
#11045=EDGE_CURVE('',#8645,#8646,#4892,.T.);
#11046=EDGE_CURVE('',#8646,#8485,#4893,.T.);
#11047=EDGE_CURVE('',#8645,#8647,#4894,.T.);
#11048=EDGE_CURVE('',#8647,#8648,#4895,.T.);
#11049=EDGE_CURVE('',#8646,#8648,#4896,.T.);
#11050=EDGE_CURVE('',#8647,#8649,#4897,.T.);
#11051=EDGE_CURVE('',#8649,#8650,#4898,.T.);
#11052=EDGE_CURVE('',#8648,#8650,#4899,.T.);
#11053=EDGE_CURVE('',#8649,#8651,#4900,.T.);
#11054=EDGE_CURVE('',#8651,#8652,#4901,.T.);
#11055=EDGE_CURVE('',#8650,#8652,#4902,.T.);
#11056=EDGE_CURVE('',#8581,#8651,#4903,.T.);
#11057=EDGE_CURVE('',#8652,#8582,#4904,.T.);
#11058=EDGE_CURVE('',#8653,#8653,#3826,.T.);
#11059=EDGE_CURVE('',#8653,#8654,#4905,.T.);
#11060=EDGE_CURVE('',#8654,#8654,#3827,.T.);
#11061=EDGE_CURVE('',#8619,#8655,#4906,.T.);
#11062=EDGE_CURVE('',#8655,#8656,#4907,.T.);
#11063=EDGE_CURVE('',#8656,#8620,#4908,.T.);
#11064=EDGE_CURVE('',#8657,#8621,#3828,.T.);
#11065=EDGE_CURVE('',#8658,#8624,#3829,.T.);
#11066=EDGE_CURVE('',#8657,#8658,#4909,.T.);
#11067=EDGE_CURVE('',#8659,#8657,#4910,.T.);
#11068=EDGE_CURVE('',#8660,#8658,#4911,.T.);
#11069=EDGE_CURVE('',#8659,#8660,#4912,.T.);
#11070=EDGE_CURVE('',#8661,#8659,#3830,.T.);
#11071=EDGE_CURVE('',#8662,#8660,#3831,.T.);
#11072=EDGE_CURVE('',#8661,#8662,#4913,.T.);
#11073=EDGE_CURVE('',#8629,#8661,#4914,.T.);
#11074=EDGE_CURVE('',#8630,#8662,#4915,.T.);
#11075=EDGE_CURVE('',#8663,#8631,#4916,.T.);
#11076=EDGE_CURVE('',#8664,#8634,#4917,.T.);
#11077=EDGE_CURVE('',#8663,#8664,#4918,.T.);
#11078=EDGE_CURVE('',#8665,#8663,#4919,.T.);
#11079=EDGE_CURVE('',#8666,#8664,#4920,.T.);
#11080=EDGE_CURVE('',#8665,#8666,#4921,.T.);
#11081=EDGE_CURVE('',#8667,#8665,#4922,.T.);
#11082=EDGE_CURVE('',#8668,#8666,#4923,.T.);
#11083=EDGE_CURVE('',#8667,#8668,#4924,.T.);
#11084=EDGE_CURVE('',#8669,#8667,#4925,.T.);
#11085=EDGE_CURVE('',#8670,#8668,#4926,.T.);
#11086=EDGE_CURVE('',#8669,#8670,#4927,.T.);
#11087=EDGE_CURVE('',#8671,#8669,#4928,.T.);
#11088=EDGE_CURVE('',#8672,#8670,#4929,.T.);
#11089=EDGE_CURVE('',#8671,#8672,#4930,.T.);
#11090=EDGE_CURVE('',#8673,#8671,#4931,.T.);
#11091=EDGE_CURVE('',#8674,#8672,#4932,.T.);
#11092=EDGE_CURVE('',#8673,#8674,#4933,.T.);
#11093=EDGE_CURVE('',#8675,#8673,#4934,.T.);
#11094=EDGE_CURVE('',#8676,#8674,#4935,.T.);
#11095=EDGE_CURVE('',#8675,#8676,#4936,.T.);
#11096=EDGE_CURVE('',#8677,#8675,#4937,.T.);
#11097=EDGE_CURVE('',#8678,#8676,#4938,.T.);
#11098=EDGE_CURVE('',#8677,#8678,#4939,.T.);
#11099=EDGE_CURVE('',#8679,#8677,#3832,.T.);
#11100=EDGE_CURVE('',#8680,#8678,#3833,.T.);
#11101=EDGE_CURVE('',#8679,#8680,#4940,.T.);
#11102=EDGE_CURVE('',#8681,#8679,#4941,.T.);
#11103=EDGE_CURVE('',#8682,#8680,#4942,.T.);
#11104=EDGE_CURVE('',#8681,#8682,#4943,.T.);
#11105=EDGE_CURVE('',#8683,#8681,#4944,.T.);
#11106=EDGE_CURVE('',#8684,#8682,#4945,.T.);
#11107=EDGE_CURVE('',#8683,#8684,#4946,.T.);
#11108=EDGE_CURVE('',#8685,#8683,#4947,.T.);
#11109=EDGE_CURVE('',#8686,#8684,#4948,.T.);
#11110=EDGE_CURVE('',#8685,#8686,#4949,.T.);
#11111=EDGE_CURVE('',#8687,#8685,#4950,.T.);
#11112=EDGE_CURVE('',#8688,#8686,#4951,.T.);
#11113=EDGE_CURVE('',#8687,#8688,#4952,.T.);
#11114=EDGE_CURVE('',#8689,#8687,#4953,.T.);
#11115=EDGE_CURVE('',#8690,#8688,#4954,.T.);
#11116=EDGE_CURVE('',#8689,#8690,#4955,.T.);
#11117=EDGE_CURVE('',#8691,#8689,#4956,.T.);
#11118=EDGE_CURVE('',#8692,#8690,#4957,.T.);
#11119=EDGE_CURVE('',#8691,#8692,#4958,.T.);
#11120=EDGE_CURVE('',#8655,#8691,#4959,.T.);
#11121=EDGE_CURVE('',#8656,#8692,#4960,.T.);
#11122=EDGE_CURVE('',#8693,#8694,#4961,.T.);
#11123=EDGE_CURVE('',#8694,#8695,#4962,.T.);
#11124=EDGE_CURVE('',#8696,#8695,#4963,.T.);
#11125=EDGE_CURVE('',#8693,#8696,#4964,.T.);
#11126=EDGE_CURVE('',#8694,#8697,#4965,.T.);
#11127=EDGE_CURVE('',#8697,#8698,#4966,.T.);
#11128=EDGE_CURVE('',#8695,#8698,#4967,.T.);
#11129=EDGE_CURVE('',#8697,#8699,#4968,.T.);
#11130=EDGE_CURVE('',#8699,#8700,#4969,.T.);
#11131=EDGE_CURVE('',#8698,#8700,#4970,.T.);
#11132=EDGE_CURVE('',#8701,#8702,#4971,.T.);
#11133=EDGE_CURVE('',#8702,#8703,#4972,.T.);
#11134=EDGE_CURVE('',#8704,#8703,#4973,.T.);
#11135=EDGE_CURVE('',#8701,#8704,#4974,.T.);
#11136=EDGE_CURVE('',#8705,#8701,#4975,.T.);
#11137=EDGE_CURVE('',#8706,#8704,#4976,.T.);
#11138=EDGE_CURVE('',#8705,#8706,#4977,.T.);
#11139=EDGE_CURVE('',#8707,#8705,#4978,.T.);
#11140=EDGE_CURVE('',#8708,#8706,#4979,.T.);
#11141=EDGE_CURVE('',#8707,#8708,#4980,.T.);
#11142=EDGE_CURVE('',#8709,#8707,#4981,.T.);
#11143=EDGE_CURVE('',#8710,#8708,#4982,.T.);
#11144=EDGE_CURVE('',#8709,#8710,#4983,.T.);
#11145=EDGE_CURVE('',#8711,#8709,#4984,.T.);
#11146=EDGE_CURVE('',#8712,#8710,#4985,.T.);
#11147=EDGE_CURVE('',#8711,#8712,#4986,.T.);
#11148=EDGE_CURVE('',#8713,#8711,#4987,.T.);
#11149=EDGE_CURVE('',#8714,#8712,#4988,.T.);
#11150=EDGE_CURVE('',#8713,#8714,#4989,.T.);
#11151=EDGE_CURVE('',#8461,#8715,#4990,.T.);
#11152=EDGE_CURVE('',#8464,#8716,#4991,.T.);
#11153=EDGE_CURVE('',#8715,#8716,#4992,.T.);
#11154=EDGE_CURVE('',#8715,#8717,#4993,.T.);
#11155=EDGE_CURVE('',#8716,#8718,#4994,.T.);
#11156=EDGE_CURVE('',#8717,#8718,#4995,.T.);
#11157=EDGE_CURVE('',#8717,#8719,#4996,.T.);
#11158=EDGE_CURVE('',#8718,#8720,#4997,.T.);
#11159=EDGE_CURVE('',#8719,#8720,#4998,.T.);
#11160=EDGE_CURVE('',#8719,#8721,#4999,.T.);
#11161=EDGE_CURVE('',#8720,#8722,#5000,.T.);
#11162=EDGE_CURVE('',#8721,#8722,#5001,.T.);
#11163=EDGE_CURVE('',#8713,#8723,#5002,.T.);
#11164=EDGE_CURVE('',#8724,#8714,#5003,.T.);
#11165=EDGE_CURVE('',#8723,#8724,#5004,.T.);
#11166=EDGE_CURVE('',#8470,#8725,#5005,.T.);
#11167=EDGE_CURVE('',#8725,#8726,#5006,.T.);
#11168=EDGE_CURVE('',#8726,#8471,#5007,.T.);
#11169=EDGE_CURVE('',#8727,#8725,#5008,.T.);
#11170=EDGE_CURVE('',#8727,#8728,#5009,.T.);
#11171=EDGE_CURVE('',#8728,#8726,#5010,.T.);
#11172=EDGE_CURVE('',#8729,#8727,#5011,.T.);
#11173=EDGE_CURVE('',#8729,#8730,#5012,.T.);
#11174=EDGE_CURVE('',#8730,#8728,#5013,.T.);
#11175=EDGE_CURVE('',#8731,#8729,#5014,.T.);
#11176=EDGE_CURVE('',#8731,#8732,#5015,.T.);
#11177=EDGE_CURVE('',#8732,#8730,#5016,.T.);
#11178=EDGE_CURVE('',#8733,#8731,#5017,.T.);
#11179=EDGE_CURVE('',#8733,#8734,#5018,.T.);
#11180=EDGE_CURVE('',#8734,#8732,#5019,.T.);
#11181=EDGE_CURVE('',#8735,#8733,#5020,.T.);
#11182=EDGE_CURVE('',#8735,#8736,#5021,.T.);
#11183=EDGE_CURVE('',#8736,#8734,#5022,.T.);
#11184=EDGE_CURVE('',#8723,#8735,#5023,.T.);
#11185=EDGE_CURVE('',#8724,#8736,#5024,.T.);
#11186=EDGE_CURVE('',#8737,#8738,#5025,.T.);
#11187=EDGE_CURVE('',#8737,#8739,#5026,.T.);
#11188=EDGE_CURVE('',#8739,#8740,#5027,.T.);
#11189=EDGE_CURVE('',#8738,#8740,#5028,.T.);
#11190=EDGE_CURVE('',#8738,#8741,#5029,.T.);
#11191=EDGE_CURVE('',#8740,#8742,#5030,.T.);
#11192=EDGE_CURVE('',#8741,#8742,#5031,.T.);
#11193=EDGE_CURVE('',#8741,#8743,#5032,.T.);
#11194=EDGE_CURVE('',#8742,#8744,#5033,.T.);
#11195=EDGE_CURVE('',#8743,#8744,#5034,.T.);
#11196=EDGE_CURVE('',#8699,#8743,#5035,.T.);
#11197=EDGE_CURVE('',#8744,#8700,#5036,.T.);
#11198=EDGE_CURVE('',#8745,#8746,#5037,.T.);
#11199=EDGE_CURVE('',#8745,#8747,#5038,.T.);
#11200=EDGE_CURVE('',#8747,#8748,#5039,.T.);
#11201=EDGE_CURVE('',#8746,#8748,#5040,.T.);
#11202=EDGE_CURVE('',#8749,#8745,#5041,.T.);
#11203=EDGE_CURVE('',#8749,#8750,#5042,.T.);
#11204=EDGE_CURVE('',#8750,#8747,#5043,.T.);
#11205=EDGE_CURVE('',#8751,#8749,#5044,.T.);
#11206=EDGE_CURVE('',#8751,#8752,#5045,.T.);
#11207=EDGE_CURVE('',#8752,#8750,#5046,.T.);
#11208=EDGE_CURVE('',#8753,#8751,#5047,.T.);
#11209=EDGE_CURVE('',#8753,#8754,#5048,.T.);
#11210=EDGE_CURVE('',#8754,#8752,#5049,.T.);
#11211=EDGE_CURVE('',#8755,#8753,#5050,.T.);
#11212=EDGE_CURVE('',#8755,#8756,#5051,.T.);
#11213=EDGE_CURVE('',#8756,#8754,#5052,.T.);
#11214=EDGE_CURVE('',#8757,#8755,#5053,.T.);
#11215=EDGE_CURVE('',#8757,#8758,#5054,.T.);
#11216=EDGE_CURVE('',#8758,#8756,#5055,.T.);
#11217=EDGE_CURVE('',#8505,#8759,#5056,.T.);
#11218=EDGE_CURVE('',#8759,#8760,#5057,.T.);
#11219=EDGE_CURVE('',#8760,#8507,#5058,.T.);
#11220=EDGE_CURVE('',#8759,#8761,#5059,.T.);
#11221=EDGE_CURVE('',#8761,#8762,#5060,.T.);
#11222=EDGE_CURVE('',#8760,#8762,#5061,.T.);
#11223=EDGE_CURVE('',#8761,#8763,#5062,.T.);
#11224=EDGE_CURVE('',#8763,#8764,#5063,.T.);
#11225=EDGE_CURVE('',#8762,#8764,#5064,.T.);
#11226=EDGE_CURVE('',#8763,#8765,#5065,.T.);
#11227=EDGE_CURVE('',#8765,#8766,#5066,.T.);
#11228=EDGE_CURVE('',#8764,#8766,#5067,.T.);
#11229=EDGE_CURVE('',#8721,#8765,#5068,.T.);
#11230=EDGE_CURVE('',#8766,#8722,#5069,.T.);
#11231=EDGE_CURVE('',#8767,#8767,#3834,.T.);
#11232=EDGE_CURVE('',#8767,#8768,#5070,.T.);
#11233=EDGE_CURVE('',#8768,#8768,#3835,.T.);
#11234=EDGE_CURVE('',#8757,#8769,#5071,.T.);
#11235=EDGE_CURVE('',#8769,#8770,#5072,.T.);
#11236=EDGE_CURVE('',#8770,#8758,#5073,.T.);
#11237=EDGE_CURVE('',#8514,#8771,#5074,.T.);
#11238=EDGE_CURVE('',#8772,#8516,#5075,.T.);
#11239=EDGE_CURVE('',#8771,#8772,#5076,.T.);
#11240=EDGE_CURVE('',#8773,#8771,#5077,.T.);
#11241=EDGE_CURVE('',#8774,#8772,#5078,.T.);
#11242=EDGE_CURVE('',#8773,#8774,#5079,.T.);
#11243=EDGE_CURVE('',#8775,#8773,#5080,.T.);
#11244=EDGE_CURVE('',#8776,#8774,#5081,.T.);
#11245=EDGE_CURVE('',#8775,#8776,#5082,.T.);
#11246=EDGE_CURVE('',#8777,#8775,#5083,.T.);
#11247=EDGE_CURVE('',#8778,#8776,#5084,.T.);
#11248=EDGE_CURVE('',#8777,#8778,#5085,.T.);
#11249=EDGE_CURVE('',#8779,#8777,#5086,.T.);
#11250=EDGE_CURVE('',#8780,#8778,#5087,.T.);
#11251=EDGE_CURVE('',#8779,#8780,#5088,.T.);
#11252=EDGE_CURVE('',#8781,#8779,#5089,.T.);
#11253=EDGE_CURVE('',#8782,#8780,#5090,.T.);
#11254=EDGE_CURVE('',#8781,#8782,#5091,.T.);
#11255=EDGE_CURVE('',#8769,#8781,#5092,.T.);
#11256=EDGE_CURVE('',#8770,#8782,#5093,.T.);
#11257=EDGE_CURVE('',#8783,#8784,#5094,.T.);
#11258=EDGE_CURVE('',#8784,#8785,#5095,.T.);
#11259=EDGE_CURVE('',#8786,#8785,#5096,.T.);
#11260=EDGE_CURVE('',#8783,#8786,#5097,.T.);
#11261=EDGE_CURVE('',#8784,#8787,#5098,.T.);
#11262=EDGE_CURVE('',#8787,#8788,#5099,.T.);
#11263=EDGE_CURVE('',#8785,#8788,#5100,.T.);
#11264=EDGE_CURVE('',#8787,#8789,#5101,.T.);
#11265=EDGE_CURVE('',#8789,#8790,#5102,.T.);
#11266=EDGE_CURVE('',#8788,#8790,#5103,.T.);
#11267=EDGE_CURVE('',#8791,#8792,#5104,.T.);
#11268=EDGE_CURVE('',#8792,#8793,#5105,.T.);
#11269=EDGE_CURVE('',#8794,#8793,#5106,.T.);
#11270=EDGE_CURVE('',#8791,#8794,#5107,.T.);
#11271=EDGE_CURVE('',#8795,#8791,#5108,.T.);
#11272=EDGE_CURVE('',#8796,#8794,#5109,.T.);
#11273=EDGE_CURVE('',#8795,#8796,#5110,.T.);
#11274=EDGE_CURVE('',#8797,#8795,#5111,.T.);
#11275=EDGE_CURVE('',#8798,#8796,#5112,.T.);
#11276=EDGE_CURVE('',#8797,#8798,#5113,.T.);
#11277=EDGE_CURVE('',#8799,#8797,#5114,.T.);
#11278=EDGE_CURVE('',#8800,#8798,#5115,.T.);
#11279=EDGE_CURVE('',#8799,#8800,#5116,.T.);
#11280=EDGE_CURVE('',#8801,#8799,#5117,.T.);
#11281=EDGE_CURVE('',#8802,#8800,#5118,.T.);
#11282=EDGE_CURVE('',#8801,#8802,#5119,.T.);
#11283=EDGE_CURVE('',#8803,#8801,#5120,.T.);
#11284=EDGE_CURVE('',#8804,#8802,#5121,.T.);
#11285=EDGE_CURVE('',#8803,#8804,#5122,.T.);
#11286=EDGE_CURVE('',#8693,#8805,#5123,.T.);
#11287=EDGE_CURVE('',#8696,#8806,#5124,.T.);
#11288=EDGE_CURVE('',#8805,#8806,#5125,.T.);
#11289=EDGE_CURVE('',#8805,#8807,#5126,.T.);
#11290=EDGE_CURVE('',#8806,#8808,#5127,.T.);
#11291=EDGE_CURVE('',#8807,#8808,#5128,.T.);
#11292=EDGE_CURVE('',#8807,#8809,#5129,.T.);
#11293=EDGE_CURVE('',#8808,#8810,#5130,.T.);
#11294=EDGE_CURVE('',#8809,#8810,#5131,.T.);
#11295=EDGE_CURVE('',#8809,#8811,#5132,.T.);
#11296=EDGE_CURVE('',#8810,#8812,#5133,.T.);
#11297=EDGE_CURVE('',#8811,#8812,#5134,.T.);
#11298=EDGE_CURVE('',#8803,#8813,#5135,.T.);
#11299=EDGE_CURVE('',#8814,#8804,#5136,.T.);
#11300=EDGE_CURVE('',#8813,#8814,#5137,.T.);
#11301=EDGE_CURVE('',#8702,#8815,#5138,.T.);
#11302=EDGE_CURVE('',#8815,#8816,#5139,.T.);
#11303=EDGE_CURVE('',#8816,#8703,#5140,.T.);
#11304=EDGE_CURVE('',#8817,#8815,#5141,.T.);
#11305=EDGE_CURVE('',#8817,#8818,#5142,.T.);
#11306=EDGE_CURVE('',#8818,#8816,#5143,.T.);
#11307=EDGE_CURVE('',#8819,#8817,#5144,.T.);
#11308=EDGE_CURVE('',#8819,#8820,#5145,.T.);
#11309=EDGE_CURVE('',#8820,#8818,#5146,.T.);
#11310=EDGE_CURVE('',#8821,#8819,#5147,.T.);
#11311=EDGE_CURVE('',#8821,#8822,#5148,.T.);
#11312=EDGE_CURVE('',#8822,#8820,#5149,.T.);
#11313=EDGE_CURVE('',#8823,#8821,#5150,.T.);
#11314=EDGE_CURVE('',#8823,#8824,#5151,.T.);
#11315=EDGE_CURVE('',#8824,#8822,#5152,.T.);
#11316=EDGE_CURVE('',#8825,#8823,#5153,.T.);
#11317=EDGE_CURVE('',#8825,#8826,#5154,.T.);
#11318=EDGE_CURVE('',#8826,#8824,#5155,.T.);
#11319=EDGE_CURVE('',#8813,#8825,#5156,.T.);
#11320=EDGE_CURVE('',#8814,#8826,#5157,.T.);
#11321=EDGE_CURVE('',#8827,#8828,#5158,.T.);
#11322=EDGE_CURVE('',#8827,#8829,#5159,.T.);
#11323=EDGE_CURVE('',#8829,#8830,#5160,.T.);
#11324=EDGE_CURVE('',#8828,#8830,#5161,.T.);
#11325=EDGE_CURVE('',#8828,#8831,#5162,.T.);
#11326=EDGE_CURVE('',#8830,#8832,#5163,.T.);
#11327=EDGE_CURVE('',#8831,#8832,#5164,.T.);
#11328=EDGE_CURVE('',#8831,#8833,#5165,.T.);
#11329=EDGE_CURVE('',#8832,#8834,#5166,.T.);
#11330=EDGE_CURVE('',#8833,#8834,#5167,.T.);
#11331=EDGE_CURVE('',#8789,#8833,#5168,.T.);
#11332=EDGE_CURVE('',#8834,#8790,#5169,.T.);
#11333=EDGE_CURVE('',#8835,#8836,#5170,.T.);
#11334=EDGE_CURVE('',#8835,#8837,#5171,.T.);
#11335=EDGE_CURVE('',#8837,#8838,#5172,.T.);
#11336=EDGE_CURVE('',#8836,#8838,#5173,.T.);
#11337=EDGE_CURVE('',#8839,#8835,#5174,.T.);
#11338=EDGE_CURVE('',#8839,#8840,#5175,.T.);
#11339=EDGE_CURVE('',#8840,#8837,#5176,.T.);
#11340=EDGE_CURVE('',#8841,#8839,#5177,.T.);
#11341=EDGE_CURVE('',#8841,#8842,#5178,.T.);
#11342=EDGE_CURVE('',#8842,#8840,#5179,.T.);
#11343=EDGE_CURVE('',#8843,#8841,#5180,.T.);
#11344=EDGE_CURVE('',#8843,#8844,#5181,.T.);
#11345=EDGE_CURVE('',#8844,#8842,#5182,.T.);
#11346=EDGE_CURVE('',#8845,#8843,#5183,.T.);
#11347=EDGE_CURVE('',#8845,#8846,#5184,.T.);
#11348=EDGE_CURVE('',#8846,#8844,#5185,.T.);
#11349=EDGE_CURVE('',#8847,#8845,#5186,.T.);
#11350=EDGE_CURVE('',#8847,#8848,#5187,.T.);
#11351=EDGE_CURVE('',#8848,#8846,#5188,.T.);
#11352=EDGE_CURVE('',#8737,#8849,#5189,.T.);
#11353=EDGE_CURVE('',#8849,#8850,#5190,.T.);
#11354=EDGE_CURVE('',#8850,#8739,#5191,.T.);
#11355=EDGE_CURVE('',#8849,#8851,#5192,.T.);
#11356=EDGE_CURVE('',#8851,#8852,#5193,.T.);
#11357=EDGE_CURVE('',#8850,#8852,#5194,.T.);
#11358=EDGE_CURVE('',#8851,#8853,#5195,.T.);
#11359=EDGE_CURVE('',#8853,#8854,#5196,.T.);
#11360=EDGE_CURVE('',#8852,#8854,#5197,.T.);
#11361=EDGE_CURVE('',#8853,#8855,#5198,.T.);
#11362=EDGE_CURVE('',#8855,#8856,#5199,.T.);
#11363=EDGE_CURVE('',#8854,#8856,#5200,.T.);
#11364=EDGE_CURVE('',#8811,#8855,#5201,.T.);
#11365=EDGE_CURVE('',#8856,#8812,#5202,.T.);
#11366=EDGE_CURVE('',#8857,#8857,#3836,.T.);
#11367=EDGE_CURVE('',#8857,#8858,#5203,.T.);
#11368=EDGE_CURVE('',#8858,#8858,#3837,.T.);
#11369=EDGE_CURVE('',#8847,#8859,#5204,.T.);
#11370=EDGE_CURVE('',#8859,#8860,#5205,.T.);
#11371=EDGE_CURVE('',#8860,#8848,#5206,.T.);
#11372=EDGE_CURVE('',#8746,#8861,#5207,.T.);
#11373=EDGE_CURVE('',#8862,#8748,#5208,.T.);
#11374=EDGE_CURVE('',#8861,#8862,#5209,.T.);
#11375=EDGE_CURVE('',#8863,#8861,#5210,.T.);
#11376=EDGE_CURVE('',#8864,#8862,#5211,.T.);
#11377=EDGE_CURVE('',#8863,#8864,#5212,.T.);
#11378=EDGE_CURVE('',#8865,#8863,#5213,.T.);
#11379=EDGE_CURVE('',#8866,#8864,#5214,.T.);
#11380=EDGE_CURVE('',#8865,#8866,#5215,.T.);
#11381=EDGE_CURVE('',#8867,#8865,#5216,.T.);
#11382=EDGE_CURVE('',#8868,#8866,#5217,.T.);
#11383=EDGE_CURVE('',#8867,#8868,#5218,.T.);
#11384=EDGE_CURVE('',#8869,#8867,#5219,.T.);
#11385=EDGE_CURVE('',#8870,#8868,#5220,.T.);
#11386=EDGE_CURVE('',#8869,#8870,#5221,.T.);
#11387=EDGE_CURVE('',#8871,#8869,#5222,.T.);
#11388=EDGE_CURVE('',#8872,#8870,#5223,.T.);
#11389=EDGE_CURVE('',#8871,#8872,#5224,.T.);
#11390=EDGE_CURVE('',#8859,#8871,#5225,.T.);
#11391=EDGE_CURVE('',#8860,#8872,#5226,.T.);
#11392=EDGE_CURVE('',#8873,#8874,#5227,.T.);
#11393=EDGE_CURVE('',#8873,#8875,#5228,.T.);
#11394=EDGE_CURVE('',#8875,#8876,#5229,.T.);
#11395=EDGE_CURVE('',#8874,#8876,#5230,.T.);
#11396=EDGE_CURVE('',#8874,#8877,#3838,.T.);
#11397=EDGE_CURVE('',#8876,#8878,#3839,.T.);
#11398=EDGE_CURVE('',#8877,#8878,#5231,.T.);
#11399=EDGE_CURVE('',#8877,#8879,#5232,.T.);
#11400=EDGE_CURVE('',#8878,#8880,#5233,.T.);
#11401=EDGE_CURVE('',#8879,#8880,#5234,.T.);
#11402=EDGE_CURVE('',#8879,#8881,#3840,.T.);
#11403=EDGE_CURVE('',#8880,#8882,#3841,.T.);
#11404=EDGE_CURVE('',#8881,#8882,#5235,.T.);
#11405=EDGE_CURVE('',#8883,#8884,#5236,.T.);
#11406=EDGE_CURVE('',#8883,#8885,#5237,.T.);
#11407=EDGE_CURVE('',#8885,#8886,#5238,.T.);
#11408=EDGE_CURVE('',#8884,#8886,#5239,.T.);
#11409=EDGE_CURVE('',#8884,#8887,#5240,.T.);
#11410=EDGE_CURVE('',#8886,#8888,#5241,.T.);
#11411=EDGE_CURVE('',#8887,#8888,#5242,.T.);
#11412=EDGE_CURVE('',#8887,#8889,#5243,.T.);
#11413=EDGE_CURVE('',#8888,#8890,#5244,.T.);
#11414=EDGE_CURVE('',#8889,#8890,#5245,.T.);
#11415=EDGE_CURVE('',#8889,#8891,#5246,.T.);
#11416=EDGE_CURVE('',#8890,#8892,#5247,.T.);
#11417=EDGE_CURVE('',#8891,#8892,#5248,.T.);
#11418=EDGE_CURVE('',#8891,#8893,#5249,.T.);
#11419=EDGE_CURVE('',#8892,#8894,#5250,.T.);
#11420=EDGE_CURVE('',#8893,#8894,#5251,.T.);
#11421=EDGE_CURVE('',#8893,#8895,#5252,.T.);
#11422=EDGE_CURVE('',#8894,#8896,#5253,.T.);
#11423=EDGE_CURVE('',#8895,#8896,#5254,.T.);
#11424=EDGE_CURVE('',#8792,#8895,#5255,.T.);
#11425=EDGE_CURVE('',#8896,#8793,#5256,.T.);
#11426=EDGE_CURVE('',#8783,#8897,#5257,.T.);
#11427=EDGE_CURVE('',#8898,#8786,#5258,.T.);
#11428=EDGE_CURVE('',#8897,#8898,#5259,.T.);
#11429=EDGE_CURVE('',#8897,#8899,#5260,.T.);
#11430=EDGE_CURVE('',#8898,#8900,#5261,.T.);
#11431=EDGE_CURVE('',#8899,#8900,#5262,.T.);
#11432=EDGE_CURVE('',#8899,#8901,#5263,.T.);
#11433=EDGE_CURVE('',#8900,#8902,#5264,.T.);
#11434=EDGE_CURVE('',#8901,#8902,#5265,.T.);
#11435=EDGE_CURVE('',#8901,#8903,#5266,.T.);
#11436=EDGE_CURVE('',#8902,#8904,#5267,.T.);
#11437=EDGE_CURVE('',#8903,#8904,#5268,.T.);
#11438=EDGE_CURVE('',#8905,#8873,#3842,.T.);
#11439=EDGE_CURVE('',#8905,#8906,#5269,.T.);
#11440=EDGE_CURVE('',#8906,#8875,#3843,.T.);
#11441=EDGE_CURVE('',#8907,#8905,#5270,.T.);
#11442=EDGE_CURVE('',#8907,#8908,#5271,.T.);
#11443=EDGE_CURVE('',#8908,#8906,#5272,.T.);
#11444=EDGE_CURVE('',#8909,#8907,#3844,.T.);
#11445=EDGE_CURVE('',#8909,#8910,#5273,.T.);
#11446=EDGE_CURVE('',#8910,#8908,#3845,.T.);
#11447=EDGE_CURVE('',#8881,#8909,#5274,.T.);
#11448=EDGE_CURVE('',#8882,#8910,#5275,.T.);
#11449=EDGE_CURVE('',#8911,#8883,#5276,.T.);
#11450=EDGE_CURVE('',#8911,#8912,#5277,.T.);
#11451=EDGE_CURVE('',#8912,#8885,#5278,.T.);
#11452=EDGE_CURVE('',#8913,#8911,#5279,.T.);
#11453=EDGE_CURVE('',#8913,#8914,#5280,.T.);
#11454=EDGE_CURVE('',#8914,#8912,#5281,.T.);
#11455=EDGE_CURVE('',#8915,#8913,#5282,.T.);
#11456=EDGE_CURVE('',#8915,#8916,#5283,.T.);
#11457=EDGE_CURVE('',#8916,#8914,#5284,.T.);
#11458=EDGE_CURVE('',#8917,#8915,#5285,.T.);
#11459=EDGE_CURVE('',#8917,#8918,#5286,.T.);
#11460=EDGE_CURVE('',#8918,#8916,#5287,.T.);
#11461=EDGE_CURVE('',#8919,#8917,#5288,.T.);
#11462=EDGE_CURVE('',#8919,#8920,#5289,.T.);
#11463=EDGE_CURVE('',#8920,#8918,#5290,.T.);
#11464=EDGE_CURVE('',#8921,#8919,#5291,.T.);
#11465=EDGE_CURVE('',#8921,#8922,#5292,.T.);
#11466=EDGE_CURVE('',#8922,#8920,#5293,.T.);
#11467=EDGE_CURVE('',#8923,#8921,#5294,.T.);
#11468=EDGE_CURVE('',#8923,#8924,#5295,.T.);
#11469=EDGE_CURVE('',#8924,#8922,#5296,.T.);
#11470=EDGE_CURVE('',#8925,#8923,#5297,.T.);
#11471=EDGE_CURVE('',#8925,#8926,#5298,.T.);
#11472=EDGE_CURVE('',#8926,#8924,#5299,.T.);
#11473=EDGE_CURVE('',#8927,#8925,#3846,.T.);
#11474=EDGE_CURVE('',#8927,#8928,#5300,.T.);
#11475=EDGE_CURVE('',#8928,#8926,#3847,.T.);
#11476=EDGE_CURVE('',#8929,#8927,#5301,.T.);
#11477=EDGE_CURVE('',#8929,#8930,#5302,.T.);
#11478=EDGE_CURVE('',#8930,#8928,#5303,.T.);
#11479=EDGE_CURVE('',#8931,#8929,#5304,.T.);
#11480=EDGE_CURVE('',#8931,#8932,#5305,.T.);
#11481=EDGE_CURVE('',#8932,#8930,#5306,.T.);
#11482=EDGE_CURVE('',#8933,#8931,#5307,.T.);
#11483=EDGE_CURVE('',#8933,#8934,#5308,.T.);
#11484=EDGE_CURVE('',#8934,#8932,#5309,.T.);
#11485=EDGE_CURVE('',#8935,#8933,#5310,.T.);
#11486=EDGE_CURVE('',#8935,#8936,#5311,.T.);
#11487=EDGE_CURVE('',#8936,#8934,#5312,.T.);
#11488=EDGE_CURVE('',#8937,#8935,#5313,.T.);
#11489=EDGE_CURVE('',#8937,#8938,#5314,.T.);
#11490=EDGE_CURVE('',#8938,#8936,#5315,.T.);
#11491=EDGE_CURVE('',#8939,#8937,#5316,.T.);
#11492=EDGE_CURVE('',#8939,#8940,#5317,.T.);
#11493=EDGE_CURVE('',#8940,#8938,#5318,.T.);
#11494=EDGE_CURVE('',#8941,#8939,#5319,.T.);
#11495=EDGE_CURVE('',#8941,#8942,#5320,.T.);
#11496=EDGE_CURVE('',#8942,#8940,#5321,.T.);
#11497=EDGE_CURVE('',#8836,#8943,#5322,.T.);
#11498=EDGE_CURVE('',#8944,#8943,#5323,.T.);
#11499=EDGE_CURVE('',#8945,#8944,#5324,.T.);
#11500=EDGE_CURVE('',#8946,#8945,#5325,.T.);
#11501=EDGE_CURVE('',#8947,#8946,#5326,.T.);
#11502=EDGE_CURVE('',#8948,#8947,#5327,.T.);
#11503=EDGE_CURVE('',#8949,#8948,#5328,.T.);
#11504=EDGE_CURVE('',#8950,#8949,#5329,.T.);
#11505=EDGE_CURVE('',#8951,#8950,#5330,.T.);
#11506=EDGE_CURVE('',#8952,#8951,#5331,.T.);
#11507=EDGE_CURVE('',#8953,#8952,#5332,.T.);
#11508=EDGE_CURVE('',#8954,#8953,#5333,.T.);
#11509=EDGE_CURVE('',#8955,#8954,#5334,.T.);
#11510=EDGE_CURVE('',#8956,#8955,#5335,.T.);
#11511=EDGE_CURVE('',#8957,#8956,#5336,.T.);
#11512=EDGE_CURVE('',#8958,#8957,#3848,.T.);
#11513=EDGE_CURVE('',#8959,#8958,#5337,.T.);
#11514=EDGE_CURVE('',#8960,#8959,#5338,.T.);
#11515=EDGE_CURVE('',#8961,#8960,#5339,.T.);
#11516=EDGE_CURVE('',#8962,#8961,#5340,.T.);
#11517=EDGE_CURVE('',#8963,#8962,#5341,.T.);
#11518=EDGE_CURVE('',#8964,#8963,#5342,.T.);
#11519=EDGE_CURVE('',#8965,#8964,#5343,.T.);
#11520=EDGE_CURVE('',#8941,#8965,#5344,.T.);
#11521=EDGE_CURVE('',#8903,#8966,#5345,.T.);
#11522=EDGE_CURVE('',#8967,#8966,#5346,.T.);
#11523=EDGE_CURVE('',#8968,#8967,#5347,.T.);
#11524=EDGE_CURVE('',#8969,#8968,#5348,.T.);
#11525=EDGE_CURVE('',#8827,#8969,#5349,.T.);
#11526=EDGE_CURVE('',#8970,#8971,#3849,.T.);
#11527=EDGE_CURVE('',#8972,#8970,#5350,.T.);
#11528=EDGE_CURVE('',#8973,#8972,#3850,.T.);
#11529=EDGE_CURVE('',#8974,#8973,#5351,.T.);
#11530=EDGE_CURVE('',#8975,#8974,#3851,.T.);
#11531=EDGE_CURVE('',#8976,#8975,#5352,.T.);
#11532=EDGE_CURVE('',#8977,#8976,#3852,.T.);
#11533=EDGE_CURVE('',#8971,#8977,#5353,.T.);
#11534=EDGE_CURVE('',#8978,#8978,#3853,.T.);
#11535=EDGE_CURVE('',#8973,#8979,#5354,.T.);
#11536=EDGE_CURVE('',#8980,#8979,#5355,.T.);
#11537=EDGE_CURVE('',#8974,#8980,#5356,.T.);
#11538=EDGE_CURVE('',#8972,#8981,#5357,.T.);
#11539=EDGE_CURVE('',#8979,#8981,#3854,.T.);
#11540=EDGE_CURVE('',#8970,#8982,#5358,.T.);
#11541=EDGE_CURVE('',#8981,#8982,#5359,.T.);
#11542=EDGE_CURVE('',#8971,#8983,#5360,.T.);
#11543=EDGE_CURVE('',#8982,#8983,#3855,.T.);
#11544=EDGE_CURVE('',#8948,#8984,#5361,.T.);
#11545=EDGE_CURVE('',#8985,#8984,#5362,.T.);
#11546=EDGE_CURVE('',#8949,#8985,#5363,.T.);
#11547=EDGE_CURVE('',#8947,#8986,#5364,.T.);
#11548=EDGE_CURVE('',#8984,#8986,#5365,.T.);
#11549=EDGE_CURVE('',#8946,#8987,#5366,.T.);
#11550=EDGE_CURVE('',#8986,#8987,#5367,.T.);
#11551=EDGE_CURVE('',#8945,#8988,#5368,.T.);
#11552=EDGE_CURVE('',#8987,#8988,#5369,.T.);
#11553=EDGE_CURVE('',#8944,#8989,#5370,.T.);
#11554=EDGE_CURVE('',#8988,#8989,#5371,.T.);
#11555=EDGE_CURVE('',#8943,#8990,#5372,.T.);
#11556=EDGE_CURVE('',#8989,#8990,#5373,.T.);
#11557=EDGE_CURVE('',#8990,#8838,#5374,.T.);
#11558=EDGE_CURVE('',#8969,#8991,#5375,.T.);
#11559=EDGE_CURVE('',#8991,#8829,#5376,.T.);
#11560=EDGE_CURVE('',#8968,#8992,#5377,.T.);
#11561=EDGE_CURVE('',#8991,#8992,#5378,.T.);
#11562=EDGE_CURVE('',#8967,#8993,#5379,.T.);
#11563=EDGE_CURVE('',#8992,#8993,#5380,.T.);
#11564=EDGE_CURVE('',#8966,#8994,#5381,.T.);
#11565=EDGE_CURVE('',#8993,#8994,#5382,.T.);
#11566=EDGE_CURVE('',#8994,#8904,#5383,.T.);
#11567=EDGE_CURVE('',#8995,#8995,#3856,.T.);
#11568=EDGE_CURVE('',#8995,#8978,#5384,.T.);
#11569=EDGE_CURVE('',#8965,#8996,#5385,.T.);
#11570=EDGE_CURVE('',#8996,#8942,#5386,.T.);
#11571=EDGE_CURVE('',#8997,#8980,#3857,.T.);
#11572=EDGE_CURVE('',#8975,#8997,#5387,.T.);
#11573=EDGE_CURVE('',#8998,#8997,#5388,.T.);
#11574=EDGE_CURVE('',#8976,#8998,#5389,.T.);
#11575=EDGE_CURVE('',#8999,#8998,#3858,.T.);
#11576=EDGE_CURVE('',#8977,#8999,#5390,.T.);
#11577=EDGE_CURVE('',#8983,#8999,#5391,.T.);
#11578=EDGE_CURVE('',#9000,#8985,#5392,.T.);
#11579=EDGE_CURVE('',#8950,#9000,#5393,.T.);
#11580=EDGE_CURVE('',#9001,#9000,#5394,.T.);
#11581=EDGE_CURVE('',#8951,#9001,#5395,.T.);
#11582=EDGE_CURVE('',#9002,#9001,#5396,.T.);
#11583=EDGE_CURVE('',#8952,#9002,#5397,.T.);
#11584=EDGE_CURVE('',#9003,#9002,#5398,.T.);
#11585=EDGE_CURVE('',#8953,#9003,#5399,.T.);
#11586=EDGE_CURVE('',#9004,#9003,#5400,.T.);
#11587=EDGE_CURVE('',#8954,#9004,#5401,.T.);
#11588=EDGE_CURVE('',#9005,#9004,#5402,.T.);
#11589=EDGE_CURVE('',#8955,#9005,#5403,.T.);
#11590=EDGE_CURVE('',#9006,#9005,#5404,.T.);
#11591=EDGE_CURVE('',#8956,#9006,#5405,.T.);
#11592=EDGE_CURVE('',#9007,#9006,#5406,.T.);
#11593=EDGE_CURVE('',#8957,#9007,#5407,.T.);
#11594=EDGE_CURVE('',#9008,#9007,#3859,.T.);
#11595=EDGE_CURVE('',#8958,#9008,#5408,.T.);
#11596=EDGE_CURVE('',#9009,#9008,#5409,.T.);
#11597=EDGE_CURVE('',#8959,#9009,#5410,.T.);
#11598=EDGE_CURVE('',#9010,#9009,#5411,.T.);
#11599=EDGE_CURVE('',#8960,#9010,#5412,.T.);
#11600=EDGE_CURVE('',#9011,#9010,#5413,.T.);
#11601=EDGE_CURVE('',#8961,#9011,#5414,.T.);
#11602=EDGE_CURVE('',#9012,#9011,#5415,.T.);
#11603=EDGE_CURVE('',#8962,#9012,#5416,.T.);
#11604=EDGE_CURVE('',#9013,#9012,#5417,.T.);
#11605=EDGE_CURVE('',#8963,#9013,#5418,.T.);
#11606=EDGE_CURVE('',#9014,#9013,#5419,.T.);
#11607=EDGE_CURVE('',#8964,#9014,#5420,.T.);
#11608=EDGE_CURVE('',#8996,#9014,#5421,.T.);
#11609=EDGE_CURVE('',#9015,#9016,#5422,.T.);
#11610=EDGE_CURVE('',#9015,#9017,#71,.T.);
#11611=EDGE_CURVE('',#9018,#9017,#3860,.T.);
#11612=EDGE_CURVE('',#9018,#9016,#72,.T.);
#11613=EDGE_CURVE('',#9019,#9020,#5423,.T.);
#11614=EDGE_CURVE('',#9019,#9015,#73,.T.);
#11615=EDGE_CURVE('',#9016,#9020,#74,.T.);
#11616=EDGE_CURVE('',#9021,#9022,#5424,.T.);
#11617=EDGE_CURVE('',#9021,#9019,#75,.T.);
#11618=EDGE_CURVE('',#9020,#9022,#76,.T.);
#11619=EDGE_CURVE('',#9023,#9024,#5425,.T.);
#11620=EDGE_CURVE('',#9023,#9021,#77,.T.);
#11621=EDGE_CURVE('',#9022,#9024,#78,.T.);
#11622=EDGE_CURVE('',#9025,#9026,#5426,.T.);
#11623=EDGE_CURVE('',#9025,#9023,#79,.T.);
#11624=EDGE_CURVE('',#9024,#9026,#80,.T.);
#11625=EDGE_CURVE('',#9027,#9028,#5427,.T.);
#11626=EDGE_CURVE('',#9027,#9025,#81,.T.);
#11627=EDGE_CURVE('',#9026,#9028,#82,.T.);
#11628=EDGE_CURVE('',#9029,#9030,#5428,.T.);
#11629=EDGE_CURVE('',#9029,#9027,#83,.T.);
#11630=EDGE_CURVE('',#9028,#9030,#84,.T.);
#11631=EDGE_CURVE('',#9031,#9032,#5429,.T.);
#11632=EDGE_CURVE('',#9031,#9029,#85,.T.);
#11633=EDGE_CURVE('',#9030,#9032,#86,.T.);
#11634=EDGE_CURVE('',#9033,#9034,#5430,.T.);
#11635=EDGE_CURVE('',#9033,#9031,#87,.T.);
#11636=EDGE_CURVE('',#9032,#9034,#88,.T.);
#11637=EDGE_CURVE('',#9035,#9036,#5431,.T.);
#11638=EDGE_CURVE('',#9035,#9033,#89,.T.);
#11639=EDGE_CURVE('',#9034,#9036,#90,.T.);
#11640=EDGE_CURVE('',#9037,#9038,#5432,.T.);
#11641=EDGE_CURVE('',#9037,#9035,#91,.T.);
#11642=EDGE_CURVE('',#9036,#9038,#92,.T.);
#11643=EDGE_CURVE('',#9039,#9040,#5433,.T.);
#11644=EDGE_CURVE('',#9039,#9037,#93,.T.);
#11645=EDGE_CURVE('',#9038,#9040,#94,.T.);
#11646=EDGE_CURVE('',#9041,#9042,#5434,.T.);
#11647=EDGE_CURVE('',#9041,#9039,#95,.T.);
#11648=EDGE_CURVE('',#9040,#9042,#96,.T.);
#11649=EDGE_CURVE('',#9043,#9044,#5435,.T.);
#11650=EDGE_CURVE('',#9043,#9041,#97,.T.);
#11651=EDGE_CURVE('',#9042,#9044,#98,.T.);
#11652=EDGE_CURVE('',#9045,#9046,#5436,.T.);
#11653=EDGE_CURVE('',#9045,#9043,#99,.T.);
#11654=EDGE_CURVE('',#9044,#9046,#100,.T.);
#11655=EDGE_CURVE('',#9047,#9048,#5437,.T.);
#11656=EDGE_CURVE('',#9047,#9045,#101,.T.);
#11657=EDGE_CURVE('',#9046,#9048,#102,.T.);
#11658=EDGE_CURVE('',#9049,#9050,#5438,.T.);
#11659=EDGE_CURVE('',#9049,#9047,#103,.T.);
#11660=EDGE_CURVE('',#9048,#9050,#104,.T.);
#11661=EDGE_CURVE('',#9051,#9052,#5439,.T.);
#11662=EDGE_CURVE('',#9051,#9049,#105,.T.);
#11663=EDGE_CURVE('',#9050,#9052,#106,.T.);
#11664=EDGE_CURVE('',#9053,#9054,#5440,.T.);
#11665=EDGE_CURVE('',#9053,#9051,#107,.T.);
#11666=EDGE_CURVE('',#9052,#9054,#108,.T.);
#11667=EDGE_CURVE('',#9055,#9056,#5441,.T.);
#11668=EDGE_CURVE('',#9055,#9053,#109,.T.);
#11669=EDGE_CURVE('',#9054,#9056,#110,.T.);
#11670=EDGE_CURVE('',#9057,#9058,#5442,.T.);
#11671=EDGE_CURVE('',#9057,#9055,#111,.T.);
#11672=EDGE_CURVE('',#9056,#9058,#112,.T.);
#11673=EDGE_CURVE('',#9059,#9060,#5443,.T.);
#11674=EDGE_CURVE('',#9059,#9057,#113,.T.);
#11675=EDGE_CURVE('',#9058,#9060,#114,.T.);
#11676=EDGE_CURVE('',#9061,#9062,#5444,.T.);
#11677=EDGE_CURVE('',#9061,#9059,#115,.T.);
#11678=EDGE_CURVE('',#9060,#9062,#116,.T.);
#11679=EDGE_CURVE('',#9063,#9064,#5445,.T.);
#11680=EDGE_CURVE('',#9063,#9061,#117,.T.);
#11681=EDGE_CURVE('',#9062,#9064,#118,.T.);
#11682=EDGE_CURVE('',#9065,#9066,#5446,.T.);
#11683=EDGE_CURVE('',#9065,#9063,#119,.T.);
#11684=EDGE_CURVE('',#9064,#9066,#120,.T.);
#11685=EDGE_CURVE('',#9067,#9068,#5447,.T.);
#11686=EDGE_CURVE('',#9067,#9065,#121,.T.);
#11687=EDGE_CURVE('',#9066,#9068,#122,.T.);
#11688=EDGE_CURVE('',#9069,#9070,#5448,.T.);
#11689=EDGE_CURVE('',#9069,#9067,#123,.T.);
#11690=EDGE_CURVE('',#9068,#9070,#124,.T.);
#11691=EDGE_CURVE('',#9071,#9072,#5449,.T.);
#11692=EDGE_CURVE('',#9071,#9069,#125,.T.);
#11693=EDGE_CURVE('',#9070,#9072,#126,.T.);
#11694=EDGE_CURVE('',#9073,#9074,#5450,.T.);
#11695=EDGE_CURVE('',#9073,#9071,#127,.T.);
#11696=EDGE_CURVE('',#9072,#9074,#128,.T.);
#11697=EDGE_CURVE('',#9075,#9076,#5451,.T.);
#11698=EDGE_CURVE('',#9075,#9073,#129,.T.);
#11699=EDGE_CURVE('',#9074,#9076,#130,.T.);
#11700=EDGE_CURVE('',#9077,#9078,#5452,.T.);
#11701=EDGE_CURVE('',#9077,#9075,#131,.T.);
#11702=EDGE_CURVE('',#9076,#9078,#132,.T.);
#11703=EDGE_CURVE('',#9079,#9080,#5453,.T.);
#11704=EDGE_CURVE('',#9079,#9077,#133,.T.);
#11705=EDGE_CURVE('',#9078,#9080,#134,.T.);
#11706=EDGE_CURVE('',#9081,#9082,#5454,.T.);
#11707=EDGE_CURVE('',#9081,#9079,#135,.T.);
#11708=EDGE_CURVE('',#9080,#9082,#136,.T.);
#11709=EDGE_CURVE('',#9083,#9084,#5455,.T.);
#11710=EDGE_CURVE('',#9083,#9081,#137,.T.);
#11711=EDGE_CURVE('',#9082,#9084,#138,.T.);
#11712=EDGE_CURVE('',#9085,#9086,#5456,.T.);
#11713=EDGE_CURVE('',#9085,#9083,#139,.T.);
#11714=EDGE_CURVE('',#9084,#9086,#140,.T.);
#11715=EDGE_CURVE('',#9087,#9088,#5457,.T.);
#11716=EDGE_CURVE('',#9087,#9085,#141,.T.);
#11717=EDGE_CURVE('',#9086,#9088,#142,.T.);
#11718=EDGE_CURVE('',#9089,#9090,#5458,.T.);
#11719=EDGE_CURVE('',#9089,#9087,#143,.T.);
#11720=EDGE_CURVE('',#9088,#9090,#144,.T.);
#11721=EDGE_CURVE('',#9091,#9092,#5459,.T.);
#11722=EDGE_CURVE('',#9091,#9089,#145,.T.);
#11723=EDGE_CURVE('',#9090,#9092,#146,.T.);
#11724=EDGE_CURVE('',#9093,#9094,#5460,.T.);
#11725=EDGE_CURVE('',#9093,#9091,#147,.T.);
#11726=EDGE_CURVE('',#9092,#9094,#148,.T.);
#11727=EDGE_CURVE('',#9095,#9096,#5461,.T.);
#11728=EDGE_CURVE('',#9095,#9093,#149,.T.);
#11729=EDGE_CURVE('',#9094,#9096,#150,.T.);
#11730=EDGE_CURVE('',#9097,#9098,#5462,.T.);
#11731=EDGE_CURVE('',#9097,#9095,#151,.T.);
#11732=EDGE_CURVE('',#9096,#9098,#152,.T.);
#11733=EDGE_CURVE('',#9099,#9100,#5463,.T.);
#11734=EDGE_CURVE('',#9099,#9097,#153,.T.);
#11735=EDGE_CURVE('',#9098,#9100,#154,.T.);
#11736=EDGE_CURVE('',#9101,#9102,#5464,.T.);
#11737=EDGE_CURVE('',#9101,#9099,#155,.T.);
#11738=EDGE_CURVE('',#9100,#9102,#156,.T.);
#11739=EDGE_CURVE('',#9103,#9104,#5465,.T.);
#11740=EDGE_CURVE('',#9103,#9101,#157,.T.);
#11741=EDGE_CURVE('',#9102,#9104,#158,.T.);
#11742=EDGE_CURVE('',#9105,#9106,#5466,.T.);
#11743=EDGE_CURVE('',#9105,#9103,#159,.T.);
#11744=EDGE_CURVE('',#9104,#9106,#160,.T.);
#11745=EDGE_CURVE('',#9107,#9108,#5467,.T.);
#11746=EDGE_CURVE('',#9107,#9105,#161,.T.);
#11747=EDGE_CURVE('',#9106,#9108,#162,.T.);
#11748=EDGE_CURVE('',#9109,#9110,#5468,.T.);
#11749=EDGE_CURVE('',#9109,#9107,#163,.T.);
#11750=EDGE_CURVE('',#9108,#9110,#164,.T.);
#11751=EDGE_CURVE('',#9111,#9112,#5469,.T.);
#11752=EDGE_CURVE('',#9111,#9109,#165,.T.);
#11753=EDGE_CURVE('',#9110,#9112,#166,.T.);
#11754=EDGE_CURVE('',#9113,#9114,#5470,.T.);
#11755=EDGE_CURVE('',#9113,#9111,#167,.T.);
#11756=EDGE_CURVE('',#9112,#9114,#168,.T.);
#11757=EDGE_CURVE('',#9115,#9116,#5471,.T.);
#11758=EDGE_CURVE('',#9115,#9113,#169,.T.);
#11759=EDGE_CURVE('',#9114,#9116,#170,.T.);
#11760=EDGE_CURVE('',#9117,#9118,#5472,.T.);
#11761=EDGE_CURVE('',#9117,#9115,#171,.T.);
#11762=EDGE_CURVE('',#9116,#9118,#172,.T.);
#11763=EDGE_CURVE('',#9119,#9120,#5473,.T.);
#11764=EDGE_CURVE('',#9119,#9117,#173,.T.);
#11765=EDGE_CURVE('',#9118,#9120,#174,.T.);
#11766=EDGE_CURVE('',#9121,#9122,#5474,.T.);
#11767=EDGE_CURVE('',#9121,#9119,#175,.T.);
#11768=EDGE_CURVE('',#9120,#9122,#176,.T.);
#11769=EDGE_CURVE('',#9123,#9124,#5475,.T.);
#11770=EDGE_CURVE('',#9123,#9121,#177,.T.);
#11771=EDGE_CURVE('',#9122,#9124,#178,.T.);
#11772=EDGE_CURVE('',#9125,#9126,#5476,.T.);
#11773=EDGE_CURVE('',#9125,#9123,#179,.T.);
#11774=EDGE_CURVE('',#9124,#9126,#180,.T.);
#11775=EDGE_CURVE('',#9127,#9128,#5477,.T.);
#11776=EDGE_CURVE('',#9127,#9125,#181,.T.);
#11777=EDGE_CURVE('',#9126,#9128,#182,.T.);
#11778=EDGE_CURVE('',#9129,#9130,#5478,.T.);
#11779=EDGE_CURVE('',#9129,#9127,#183,.T.);
#11780=EDGE_CURVE('',#9128,#9130,#184,.T.);
#11781=EDGE_CURVE('',#9131,#9132,#5479,.T.);
#11782=EDGE_CURVE('',#9131,#9129,#185,.T.);
#11783=EDGE_CURVE('',#9130,#9132,#186,.T.);
#11784=EDGE_CURVE('',#9133,#9134,#5480,.T.);
#11785=EDGE_CURVE('',#9133,#9131,#187,.T.);
#11786=EDGE_CURVE('',#9132,#9134,#188,.T.);
#11787=EDGE_CURVE('',#9135,#9136,#5481,.T.);
#11788=EDGE_CURVE('',#9135,#9133,#189,.T.);
#11789=EDGE_CURVE('',#9134,#9136,#190,.T.);
#11790=EDGE_CURVE('',#9137,#9138,#5482,.T.);
#11791=EDGE_CURVE('',#9137,#9135,#191,.T.);
#11792=EDGE_CURVE('',#9136,#9138,#192,.T.);
#11793=EDGE_CURVE('',#9139,#9140,#5483,.T.);
#11794=EDGE_CURVE('',#9139,#9137,#193,.T.);
#11795=EDGE_CURVE('',#9138,#9140,#194,.T.);
#11796=EDGE_CURVE('',#9141,#9142,#5484,.T.);
#11797=EDGE_CURVE('',#9141,#9139,#195,.T.);
#11798=EDGE_CURVE('',#9140,#9142,#196,.T.);
#11799=EDGE_CURVE('',#9143,#9144,#5485,.T.);
#11800=EDGE_CURVE('',#9143,#9141,#197,.T.);
#11801=EDGE_CURVE('',#9142,#9144,#198,.T.);
#11802=EDGE_CURVE('',#9145,#9146,#5486,.T.);
#11803=EDGE_CURVE('',#9145,#9143,#199,.T.);
#11804=EDGE_CURVE('',#9144,#9146,#200,.T.);
#11805=EDGE_CURVE('',#9147,#9148,#5487,.T.);
#11806=EDGE_CURVE('',#9147,#9145,#201,.T.);
#11807=EDGE_CURVE('',#9146,#9148,#202,.T.);
#11808=EDGE_CURVE('',#9149,#9150,#5488,.T.);
#11809=EDGE_CURVE('',#9149,#9147,#203,.T.);
#11810=EDGE_CURVE('',#9148,#9150,#204,.T.);
#11811=EDGE_CURVE('',#9151,#9152,#5489,.T.);
#11812=EDGE_CURVE('',#9151,#9149,#205,.T.);
#11813=EDGE_CURVE('',#9150,#9152,#206,.T.);
#11814=EDGE_CURVE('',#9153,#9154,#5490,.T.);
#11815=EDGE_CURVE('',#9153,#9151,#207,.T.);
#11816=EDGE_CURVE('',#9152,#9154,#208,.T.);
#11817=EDGE_CURVE('',#9155,#9156,#5491,.T.);
#11818=EDGE_CURVE('',#9155,#9153,#209,.T.);
#11819=EDGE_CURVE('',#9154,#9156,#210,.T.);
#11820=EDGE_CURVE('',#9157,#9158,#5492,.T.);
#11821=EDGE_CURVE('',#9157,#9155,#211,.T.);
#11822=EDGE_CURVE('',#9156,#9158,#212,.T.);
#11823=EDGE_CURVE('',#9159,#9160,#5493,.T.);
#11824=EDGE_CURVE('',#9159,#9157,#213,.T.);
#11825=EDGE_CURVE('',#9158,#9160,#214,.T.);
#11826=EDGE_CURVE('',#9161,#9162,#5494,.T.);
#11827=EDGE_CURVE('',#9161,#9159,#215,.T.);
#11828=EDGE_CURVE('',#9160,#9162,#216,.T.);
#11829=EDGE_CURVE('',#9163,#9164,#5495,.T.);
#11830=EDGE_CURVE('',#9163,#9161,#217,.T.);
#11831=EDGE_CURVE('',#9162,#9164,#218,.T.);
#11832=EDGE_CURVE('',#9165,#9166,#5496,.T.);
#11833=EDGE_CURVE('',#9165,#9163,#219,.T.);
#11834=EDGE_CURVE('',#9164,#9166,#220,.T.);
#11835=EDGE_CURVE('',#9167,#9168,#5497,.T.);
#11836=EDGE_CURVE('',#9167,#9165,#221,.T.);
#11837=EDGE_CURVE('',#9166,#9168,#222,.T.);
#11838=EDGE_CURVE('',#9169,#9170,#5498,.T.);
#11839=EDGE_CURVE('',#9169,#9167,#223,.T.);
#11840=EDGE_CURVE('',#9168,#9170,#224,.T.);
#11841=EDGE_CURVE('',#9171,#9172,#5499,.T.);
#11842=EDGE_CURVE('',#9171,#9169,#225,.T.);
#11843=EDGE_CURVE('',#9170,#9172,#226,.T.);
#11844=EDGE_CURVE('',#9173,#9174,#5500,.T.);
#11845=EDGE_CURVE('',#9173,#9171,#227,.T.);
#11846=EDGE_CURVE('',#9172,#9174,#228,.T.);
#11847=EDGE_CURVE('',#9175,#9176,#5501,.T.);
#11848=EDGE_CURVE('',#9175,#9173,#229,.T.);
#11849=EDGE_CURVE('',#9174,#9176,#230,.T.);
#11850=EDGE_CURVE('',#9177,#9178,#5502,.T.);
#11851=EDGE_CURVE('',#9177,#9175,#231,.T.);
#11852=EDGE_CURVE('',#9176,#9178,#232,.T.);
#11853=EDGE_CURVE('',#9179,#9180,#5503,.T.);
#11854=EDGE_CURVE('',#9179,#9177,#233,.T.);
#11855=EDGE_CURVE('',#9178,#9180,#234,.T.);
#11856=EDGE_CURVE('',#9181,#9182,#5504,.T.);
#11857=EDGE_CURVE('',#9181,#9179,#235,.T.);
#11858=EDGE_CURVE('',#9180,#9182,#236,.T.);
#11859=EDGE_CURVE('',#9183,#9184,#5505,.T.);
#11860=EDGE_CURVE('',#9183,#9181,#237,.T.);
#11861=EDGE_CURVE('',#9182,#9184,#238,.T.);
#11862=EDGE_CURVE('',#9185,#9186,#5506,.T.);
#11863=EDGE_CURVE('',#9185,#9183,#239,.T.);
#11864=EDGE_CURVE('',#9184,#9186,#240,.T.);
#11865=EDGE_CURVE('',#9187,#9188,#5507,.T.);
#11866=EDGE_CURVE('',#9187,#9185,#241,.T.);
#11867=EDGE_CURVE('',#9186,#9188,#242,.T.);
#11868=EDGE_CURVE('',#9189,#9190,#5508,.T.);
#11869=EDGE_CURVE('',#9189,#9187,#243,.T.);
#11870=EDGE_CURVE('',#9188,#9190,#244,.T.);
#11871=EDGE_CURVE('',#9191,#9192,#5509,.T.);
#11872=EDGE_CURVE('',#9191,#9189,#245,.T.);
#11873=EDGE_CURVE('',#9190,#9192,#246,.T.);
#11874=EDGE_CURVE('',#9193,#9194,#5510,.T.);
#11875=EDGE_CURVE('',#9193,#9191,#247,.T.);
#11876=EDGE_CURVE('',#9192,#9194,#248,.T.);
#11877=EDGE_CURVE('',#9195,#9196,#5511,.T.);
#11878=EDGE_CURVE('',#9195,#9193,#249,.T.);
#11879=EDGE_CURVE('',#9194,#9196,#250,.T.);
#11880=EDGE_CURVE('',#9197,#9198,#5512,.T.);
#11881=EDGE_CURVE('',#9197,#9195,#251,.T.);
#11882=EDGE_CURVE('',#9196,#9198,#252,.T.);
#11883=EDGE_CURVE('',#9199,#9200,#5513,.T.);
#11884=EDGE_CURVE('',#9199,#9197,#253,.T.);
#11885=EDGE_CURVE('',#9198,#9200,#254,.T.);
#11886=EDGE_CURVE('',#9201,#9202,#5514,.T.);
#11887=EDGE_CURVE('',#9201,#9199,#255,.T.);
#11888=EDGE_CURVE('',#9200,#9202,#256,.T.);
#11889=EDGE_CURVE('',#9203,#9204,#5515,.T.);
#11890=EDGE_CURVE('',#9203,#9201,#257,.T.);
#11891=EDGE_CURVE('',#9202,#9204,#258,.T.);
#11892=EDGE_CURVE('',#9205,#9206,#5516,.T.);
#11893=EDGE_CURVE('',#9205,#9203,#259,.T.);
#11894=EDGE_CURVE('',#9204,#9206,#260,.T.);
#11895=EDGE_CURVE('',#9207,#9208,#5517,.T.);
#11896=EDGE_CURVE('',#9207,#9205,#261,.T.);
#11897=EDGE_CURVE('',#9206,#9208,#262,.T.);
#11898=EDGE_CURVE('',#9209,#9210,#5518,.T.);
#11899=EDGE_CURVE('',#9209,#9207,#263,.T.);
#11900=EDGE_CURVE('',#9208,#9210,#264,.T.);
#11901=EDGE_CURVE('',#9211,#9212,#5519,.T.);
#11902=EDGE_CURVE('',#9211,#9209,#265,.T.);
#11903=EDGE_CURVE('',#9210,#9212,#266,.T.);
#11904=EDGE_CURVE('',#9213,#9214,#5520,.T.);
#11905=EDGE_CURVE('',#9213,#9211,#267,.T.);
#11906=EDGE_CURVE('',#9212,#9214,#268,.T.);
#11907=EDGE_CURVE('',#9215,#9216,#5521,.T.);
#11908=EDGE_CURVE('',#9215,#9213,#269,.T.);
#11909=EDGE_CURVE('',#9214,#9216,#270,.T.);
#11910=EDGE_CURVE('',#9217,#9218,#5522,.T.);
#11911=EDGE_CURVE('',#9217,#9219,#3861,.T.);
#11912=EDGE_CURVE('',#9219,#9215,#271,.T.);
#11913=EDGE_CURVE('',#9216,#9218,#272,.T.);
#11914=EDGE_CURVE('',#9220,#9221,#5523,.T.);
#11915=EDGE_CURVE('',#9220,#9222,#273,.F.);
#11916=EDGE_CURVE('',#9222,#9223,#5524,.T.);
#11917=EDGE_CURVE('',#9223,#9223,#3862,.F.);
#11918=EDGE_CURVE('',#9222,#9224,#274,.F.);
#11919=EDGE_CURVE('',#9224,#9225,#3863,.T.);
#11920=EDGE_CURVE('',#9225,#9221,#275,.F.);
#11921=EDGE_CURVE('',#9226,#9227,#5525,.T.);
#11922=EDGE_CURVE('',#9226,#9220,#276,.F.);
#11923=EDGE_CURVE('',#9221,#9227,#277,.F.);
#11924=EDGE_CURVE('',#9228,#9229,#5526,.T.);
#11925=EDGE_CURVE('',#9228,#9226,#278,.F.);
#11926=EDGE_CURVE('',#9227,#9229,#279,.F.);
#11927=EDGE_CURVE('',#9230,#9231,#5527,.T.);
#11928=EDGE_CURVE('',#9230,#9228,#280,.F.);
#11929=EDGE_CURVE('',#9229,#9231,#281,.F.);
#11930=EDGE_CURVE('',#9232,#9233,#5528,.T.);
#11931=EDGE_CURVE('',#9232,#9230,#282,.F.);
#11932=EDGE_CURVE('',#9231,#9233,#283,.F.);
#11933=EDGE_CURVE('',#9234,#9235,#5529,.T.);
#11934=EDGE_CURVE('',#9234,#9232,#284,.F.);
#11935=EDGE_CURVE('',#9233,#9235,#285,.F.);
#11936=EDGE_CURVE('',#9236,#9237,#5530,.T.);
#11937=EDGE_CURVE('',#9236,#9234,#286,.F.);
#11938=EDGE_CURVE('',#9235,#9237,#287,.F.);
#11939=EDGE_CURVE('',#9238,#9239,#5531,.T.);
#11940=EDGE_CURVE('',#9238,#9236,#288,.F.);
#11941=EDGE_CURVE('',#9237,#9239,#289,.F.);
#11942=EDGE_CURVE('',#9240,#9241,#5532,.T.);
#11943=EDGE_CURVE('',#9240,#9238,#290,.F.);
#11944=EDGE_CURVE('',#9239,#9241,#291,.F.);
#11945=EDGE_CURVE('',#9242,#9243,#5533,.T.);
#11946=EDGE_CURVE('',#9244,#9242,#3864,.F.);
#11947=EDGE_CURVE('',#9244,#9240,#292,.F.);
#11948=EDGE_CURVE('',#9241,#9243,#293,.F.);
#11949=EDGE_CURVE('',#9245,#9246,#5534,.T.);
#11950=EDGE_CURVE('',#9245,#9247,#294,.T.);
#11951=EDGE_CURVE('',#9248,#9247,#3865,.T.);
#11952=EDGE_CURVE('',#9246,#9248,#295,.T.);
#11953=EDGE_CURVE('',#9249,#9250,#5535,.T.);
#11954=EDGE_CURVE('',#9249,#9245,#296,.T.);
#11955=EDGE_CURVE('',#9250,#9246,#297,.T.);
#11956=EDGE_CURVE('',#9251,#9252,#5536,.T.);
#11957=EDGE_CURVE('',#9251,#9249,#298,.T.);
#11958=EDGE_CURVE('',#9252,#9250,#299,.T.);
#11959=EDGE_CURVE('',#9253,#9254,#5537,.T.);
#11960=EDGE_CURVE('',#9253,#9251,#300,.T.);
#11961=EDGE_CURVE('',#9254,#9252,#301,.T.);
#11962=EDGE_CURVE('',#9255,#9256,#5538,.T.);
#11963=EDGE_CURVE('',#9255,#9253,#302,.T.);
#11964=EDGE_CURVE('',#9256,#9254,#303,.T.);
#11965=EDGE_CURVE('',#9257,#9258,#5539,.T.);
#11966=EDGE_CURVE('',#9257,#9255,#304,.T.);
#11967=EDGE_CURVE('',#9258,#9256,#305,.T.);
#11968=EDGE_CURVE('',#9259,#9260,#5540,.T.);
#11969=EDGE_CURVE('',#9259,#9257,#306,.T.);
#11970=EDGE_CURVE('',#9260,#9258,#307,.T.);
#11971=EDGE_CURVE('',#9261,#9262,#5541,.T.);
#11972=EDGE_CURVE('',#9261,#9259,#308,.T.);
#11973=EDGE_CURVE('',#9262,#9260,#309,.T.);
#11974=EDGE_CURVE('',#9263,#9264,#5542,.T.);
#11975=EDGE_CURVE('',#9263,#9261,#310,.T.);
#11976=EDGE_CURVE('',#9264,#9262,#311,.T.);
#11977=EDGE_CURVE('',#9265,#9266,#5543,.T.);
#11978=EDGE_CURVE('',#9265,#9263,#312,.T.);
#11979=EDGE_CURVE('',#9266,#9264,#313,.T.);
#11980=EDGE_CURVE('',#9267,#9268,#5544,.T.);
#11981=EDGE_CURVE('',#9267,#9269,#314,.T.);
#11982=EDGE_CURVE('',#9269,#9270,#3866,.T.);
#11983=EDGE_CURVE('',#9268,#9270,#315,.T.);
#11984=EDGE_CURVE('',#9271,#9272,#5545,.T.);
#11985=EDGE_CURVE('',#9271,#9267,#316,.T.);
#11986=EDGE_CURVE('',#9272,#9268,#317,.T.);
#11987=EDGE_CURVE('',#9273,#9274,#5546,.T.);
#11988=EDGE_CURVE('',#9273,#9271,#318,.T.);
#11989=EDGE_CURVE('',#9274,#9272,#319,.T.);
#11990=EDGE_CURVE('',#9275,#9276,#5547,.T.);
#11991=EDGE_CURVE('',#9275,#9273,#320,.T.);
#11992=EDGE_CURVE('',#9276,#9274,#321,.T.);
#11993=EDGE_CURVE('',#9277,#9278,#5548,.T.);
#11994=EDGE_CURVE('',#9277,#9275,#322,.T.);
#11995=EDGE_CURVE('',#9278,#9276,#323,.T.);
#11996=EDGE_CURVE('',#9279,#9280,#5549,.T.);
#11997=EDGE_CURVE('',#9279,#9277,#324,.T.);
#11998=EDGE_CURVE('',#9280,#9278,#325,.T.);
#11999=EDGE_CURVE('',#9281,#9282,#5550,.T.);
#12000=EDGE_CURVE('',#9281,#9279,#326,.T.);
#12001=EDGE_CURVE('',#9282,#9280,#327,.T.);
#12002=EDGE_CURVE('',#9283,#9284,#5551,.T.);
#12003=EDGE_CURVE('',#9283,#9281,#328,.T.);
#12004=EDGE_CURVE('',#9284,#9282,#329,.T.);
#12005=EDGE_CURVE('',#9285,#9286,#5552,.T.);
#12006=EDGE_CURVE('',#9285,#9283,#330,.T.);
#12007=EDGE_CURVE('',#9286,#9284,#331,.T.);
#12008=EDGE_CURVE('',#9287,#9288,#5553,.T.);
#12009=EDGE_CURVE('',#9287,#9285,#332,.T.);
#12010=EDGE_CURVE('',#9288,#9286,#333,.T.);
#12011=EDGE_CURVE('',#9289,#9290,#5554,.T.);
#12012=EDGE_CURVE('',#9289,#9287,#334,.T.);
#12013=EDGE_CURVE('',#9290,#9288,#335,.T.);
#12014=EDGE_CURVE('',#9291,#9292,#5555,.T.);
#12015=EDGE_CURVE('',#9291,#9289,#336,.T.);
#12016=EDGE_CURVE('',#9292,#9290,#337,.T.);
#12017=EDGE_CURVE('',#9293,#9294,#5556,.T.);
#12018=EDGE_CURVE('',#9293,#9291,#338,.T.);
#12019=EDGE_CURVE('',#9294,#9292,#339,.T.);
#12020=EDGE_CURVE('',#9295,#9296,#5557,.T.);
#12021=EDGE_CURVE('',#9295,#9293,#340,.T.);
#12022=EDGE_CURVE('',#9296,#9294,#341,.T.);
#12023=EDGE_CURVE('',#9297,#9298,#5558,.T.);
#12024=EDGE_CURVE('',#9297,#9295,#342,.T.);
#12025=EDGE_CURVE('',#9298,#9296,#343,.T.);
#12026=EDGE_CURVE('',#9299,#9300,#5559,.T.);
#12027=EDGE_CURVE('',#9299,#9297,#344,.T.);
#12028=EDGE_CURVE('',#9300,#9298,#345,.T.);
#12029=EDGE_CURVE('',#9301,#9302,#5560,.T.);
#12030=EDGE_CURVE('',#9301,#9299,#346,.T.);
#12031=EDGE_CURVE('',#9302,#9300,#347,.T.);
#12032=EDGE_CURVE('',#9303,#9304,#5561,.T.);
#12033=EDGE_CURVE('',#9303,#9301,#348,.T.);
#12034=EDGE_CURVE('',#9304,#9302,#349,.T.);
#12035=EDGE_CURVE('',#9305,#9306,#5562,.T.);
#12036=EDGE_CURVE('',#9305,#9303,#350,.T.);
#12037=EDGE_CURVE('',#9306,#9304,#351,.T.);
#12038=EDGE_CURVE('',#9307,#9308,#5563,.T.);
#12039=EDGE_CURVE('',#9307,#9305,#352,.T.);
#12040=EDGE_CURVE('',#9308,#9306,#353,.T.);
#12041=EDGE_CURVE('',#9309,#9310,#5564,.T.);
#12042=EDGE_CURVE('',#9309,#9307,#354,.T.);
#12043=EDGE_CURVE('',#9310,#9308,#355,.T.);
#12044=EDGE_CURVE('',#9311,#9312,#5565,.T.);
#12045=EDGE_CURVE('',#9311,#9309,#356,.T.);
#12046=EDGE_CURVE('',#9312,#9310,#357,.T.);
#12047=EDGE_CURVE('',#9313,#9314,#5566,.T.);
#12048=EDGE_CURVE('',#9313,#9311,#358,.T.);
#12049=EDGE_CURVE('',#9314,#9312,#359,.T.);
#12050=EDGE_CURVE('',#9315,#9316,#5567,.T.);
#12051=EDGE_CURVE('',#9315,#9313,#360,.T.);
#12052=EDGE_CURVE('',#9316,#9314,#361,.T.);
#12053=EDGE_CURVE('',#9317,#9318,#5568,.T.);
#12054=EDGE_CURVE('',#9317,#9315,#362,.T.);
#12055=EDGE_CURVE('',#9318,#9316,#363,.T.);
#12056=EDGE_CURVE('',#9319,#9320,#5569,.T.);
#12057=EDGE_CURVE('',#9319,#9317,#364,.T.);
#12058=EDGE_CURVE('',#9320,#9318,#365,.T.);
#12059=EDGE_CURVE('',#9321,#9322,#5570,.T.);
#12060=EDGE_CURVE('',#9321,#9319,#366,.T.);
#12061=EDGE_CURVE('',#9322,#9320,#367,.T.);
#12062=EDGE_CURVE('',#9323,#9324,#5571,.T.);
#12063=EDGE_CURVE('',#9323,#9321,#368,.T.);
#12064=EDGE_CURVE('',#9324,#9322,#369,.T.);
#12065=EDGE_CURVE('',#9325,#9326,#5572,.T.);
#12066=EDGE_CURVE('',#9325,#9323,#370,.T.);
#12067=EDGE_CURVE('',#9326,#9324,#371,.T.);
#12068=EDGE_CURVE('',#9327,#9328,#5573,.T.);
#12069=EDGE_CURVE('',#9327,#9325,#372,.T.);
#12070=EDGE_CURVE('',#9328,#9326,#373,.T.);
#12071=EDGE_CURVE('',#9329,#9330,#5574,.T.);
#12072=EDGE_CURVE('',#9329,#9327,#374,.T.);
#12073=EDGE_CURVE('',#9330,#9328,#375,.T.);
#12074=EDGE_CURVE('',#9331,#9332,#5575,.T.);
#12075=EDGE_CURVE('',#9331,#9329,#376,.T.);
#12076=EDGE_CURVE('',#9332,#9330,#377,.T.);
#12077=EDGE_CURVE('',#9333,#9334,#5576,.T.);
#12078=EDGE_CURVE('',#9333,#9331,#378,.T.);
#12079=EDGE_CURVE('',#9334,#9332,#379,.T.);
#12080=EDGE_CURVE('',#9335,#9336,#5577,.T.);
#12081=EDGE_CURVE('',#9335,#9333,#380,.T.);
#12082=EDGE_CURVE('',#9336,#9334,#381,.T.);
#12083=EDGE_CURVE('',#9337,#9338,#5578,.T.);
#12084=EDGE_CURVE('',#9337,#9335,#382,.T.);
#12085=EDGE_CURVE('',#9338,#9336,#383,.T.);
#12086=EDGE_CURVE('',#9339,#9340,#5579,.T.);
#12087=EDGE_CURVE('',#9339,#9337,#384,.T.);
#12088=EDGE_CURVE('',#9340,#9338,#385,.T.);
#12089=EDGE_CURVE('',#9341,#9342,#5580,.T.);
#12090=EDGE_CURVE('',#9341,#9339,#386,.T.);
#12091=EDGE_CURVE('',#9342,#9340,#387,.T.);
#12092=EDGE_CURVE('',#9343,#9344,#5581,.T.);
#12093=EDGE_CURVE('',#9343,#9341,#388,.T.);
#12094=EDGE_CURVE('',#9344,#9342,#389,.T.);
#12095=EDGE_CURVE('',#9345,#9346,#5582,.T.);
#12096=EDGE_CURVE('',#9345,#9343,#390,.T.);
#12097=EDGE_CURVE('',#9346,#9344,#391,.T.);
#12098=EDGE_CURVE('',#9347,#9348,#5583,.T.);
#12099=EDGE_CURVE('',#9347,#9345,#392,.T.);
#12100=EDGE_CURVE('',#9348,#9346,#393,.T.);
#12101=EDGE_CURVE('',#9349,#9350,#5584,.T.);
#12102=EDGE_CURVE('',#9349,#9347,#394,.T.);
#12103=EDGE_CURVE('',#9350,#9348,#395,.T.);
#12104=EDGE_CURVE('',#9351,#9352,#5585,.T.);
#12105=EDGE_CURVE('',#9351,#9349,#396,.T.);
#12106=EDGE_CURVE('',#9352,#9350,#397,.T.);
#12107=EDGE_CURVE('',#9353,#9354,#5586,.T.);
#12108=EDGE_CURVE('',#9353,#9351,#398,.T.);
#12109=EDGE_CURVE('',#9354,#9352,#399,.T.);
#12110=EDGE_CURVE('',#9355,#9356,#5587,.T.);
#12111=EDGE_CURVE('',#9355,#9353,#400,.T.);
#12112=EDGE_CURVE('',#9356,#9354,#401,.T.);
#12113=EDGE_CURVE('',#9357,#9358,#5588,.T.);
#12114=EDGE_CURVE('',#9357,#9355,#402,.T.);
#12115=EDGE_CURVE('',#9358,#9356,#403,.T.);
#12116=EDGE_CURVE('',#9359,#9360,#5589,.T.);
#12117=EDGE_CURVE('',#9359,#9357,#404,.T.);
#12118=EDGE_CURVE('',#9360,#9358,#405,.T.);
#12119=EDGE_CURVE('',#9361,#9362,#5590,.T.);
#12120=EDGE_CURVE('',#9361,#9359,#406,.T.);
#12121=EDGE_CURVE('',#9362,#9360,#407,.T.);
#12122=EDGE_CURVE('',#9363,#9364,#5591,.T.);
#12123=EDGE_CURVE('',#9363,#9361,#408,.T.);
#12124=EDGE_CURVE('',#9364,#9362,#409,.T.);
#12125=EDGE_CURVE('',#9365,#9366,#5592,.T.);
#12126=EDGE_CURVE('',#9365,#9363,#410,.T.);
#12127=EDGE_CURVE('',#9366,#9364,#411,.T.);
#12128=EDGE_CURVE('',#9367,#9368,#5593,.T.);
#12129=EDGE_CURVE('',#9367,#9365,#412,.T.);
#12130=EDGE_CURVE('',#9368,#9366,#413,.T.);
#12131=EDGE_CURVE('',#9369,#9370,#5594,.T.);
#12132=EDGE_CURVE('',#9369,#9367,#414,.T.);
#12133=EDGE_CURVE('',#9370,#9368,#415,.T.);
#12134=EDGE_CURVE('',#9371,#9372,#5595,.T.);
#12135=EDGE_CURVE('',#9371,#9369,#416,.T.);
#12136=EDGE_CURVE('',#9372,#9370,#417,.T.);
#12137=EDGE_CURVE('',#9373,#9374,#5596,.T.);
#12138=EDGE_CURVE('',#9373,#9371,#418,.T.);
#12139=EDGE_CURVE('',#9374,#9372,#419,.T.);
#12140=EDGE_CURVE('',#9375,#9376,#5597,.T.);
#12141=EDGE_CURVE('',#9375,#9373,#420,.T.);
#12142=EDGE_CURVE('',#9376,#9374,#421,.T.);
#12143=EDGE_CURVE('',#9377,#9378,#5598,.T.);
#12144=EDGE_CURVE('',#9377,#9375,#422,.T.);
#12145=EDGE_CURVE('',#9378,#9376,#423,.T.);
#12146=EDGE_CURVE('',#9379,#9380,#5599,.T.);
#12147=EDGE_CURVE('',#9379,#9377,#424,.T.);
#12148=EDGE_CURVE('',#9380,#9378,#425,.T.);
#12149=EDGE_CURVE('',#9381,#9382,#5600,.T.);
#12150=EDGE_CURVE('',#9381,#9379,#426,.T.);
#12151=EDGE_CURVE('',#9382,#9380,#427,.T.);
#12152=EDGE_CURVE('',#9383,#9384,#5601,.T.);
#12153=EDGE_CURVE('',#9383,#9381,#428,.T.);
#12154=EDGE_CURVE('',#9384,#9382,#429,.T.);
#12155=EDGE_CURVE('',#9385,#9386,#5602,.T.);
#12156=EDGE_CURVE('',#9385,#9383,#430,.T.);
#12157=EDGE_CURVE('',#9386,#9384,#431,.T.);
#12158=EDGE_CURVE('',#9387,#9388,#5603,.T.);
#12159=EDGE_CURVE('',#9387,#9385,#432,.T.);
#12160=EDGE_CURVE('',#9388,#9386,#433,.T.);
#12161=EDGE_CURVE('',#9389,#9390,#5604,.T.);
#12162=EDGE_CURVE('',#9389,#9387,#434,.T.);
#12163=EDGE_CURVE('',#9390,#9388,#435,.T.);
#12164=EDGE_CURVE('',#9391,#9392,#5605,.T.);
#12165=EDGE_CURVE('',#9391,#9389,#436,.T.);
#12166=EDGE_CURVE('',#9392,#9390,#437,.T.);
#12167=EDGE_CURVE('',#9393,#9394,#5606,.T.);
#12168=EDGE_CURVE('',#9393,#9391,#438,.T.);
#12169=EDGE_CURVE('',#9394,#9392,#439,.T.);
#12170=EDGE_CURVE('',#9395,#9396,#5607,.T.);
#12171=EDGE_CURVE('',#9395,#9393,#440,.T.);
#12172=EDGE_CURVE('',#9396,#9394,#441,.T.);
#12173=EDGE_CURVE('',#9397,#9398,#5608,.T.);
#12174=EDGE_CURVE('',#9397,#9395,#442,.T.);
#12175=EDGE_CURVE('',#9398,#9396,#443,.T.);
#12176=EDGE_CURVE('',#9399,#9400,#5609,.T.);
#12177=EDGE_CURVE('',#9399,#9397,#444,.T.);
#12178=EDGE_CURVE('',#9400,#9398,#445,.T.);
#12179=EDGE_CURVE('',#9401,#9402,#5610,.T.);
#12180=EDGE_CURVE('',#9401,#9399,#446,.T.);
#12181=EDGE_CURVE('',#9402,#9400,#447,.T.);
#12182=EDGE_CURVE('',#9403,#9404,#5611,.T.);
#12183=EDGE_CURVE('',#9403,#9401,#448,.T.);
#12184=EDGE_CURVE('',#9404,#9402,#449,.T.);
#12185=EDGE_CURVE('',#9405,#9406,#5612,.T.);
#12186=EDGE_CURVE('',#9405,#9403,#450,.T.);
#12187=EDGE_CURVE('',#9406,#9404,#451,.T.);
#12188=EDGE_CURVE('',#9407,#9408,#5613,.T.);
#12189=EDGE_CURVE('',#9407,#9405,#452,.T.);
#12190=EDGE_CURVE('',#9408,#9406,#453,.T.);
#12191=EDGE_CURVE('',#9409,#9410,#5614,.T.);
#12192=EDGE_CURVE('',#9409,#9407,#454,.T.);
#12193=EDGE_CURVE('',#9410,#9408,#455,.T.);
#12194=EDGE_CURVE('',#9411,#9412,#5615,.T.);
#12195=EDGE_CURVE('',#9411,#9409,#456,.T.);
#12196=EDGE_CURVE('',#9412,#9410,#457,.T.);
#12197=EDGE_CURVE('',#9413,#9414,#5616,.T.);
#12198=EDGE_CURVE('',#9413,#9411,#458,.T.);
#12199=EDGE_CURVE('',#9414,#9412,#459,.T.);
#12200=EDGE_CURVE('',#9415,#9416,#5617,.T.);
#12201=EDGE_CURVE('',#9415,#9413,#460,.T.);
#12202=EDGE_CURVE('',#9416,#9414,#461,.T.);
#12203=EDGE_CURVE('',#9417,#9418,#5618,.T.);
#12204=EDGE_CURVE('',#9417,#9415,#462,.T.);
#12205=EDGE_CURVE('',#9418,#9416,#463,.T.);
#12206=EDGE_CURVE('',#9419,#9420,#5619,.T.);
#12207=EDGE_CURVE('',#9419,#9417,#464,.T.);
#12208=EDGE_CURVE('',#9420,#9418,#465,.T.);
#12209=EDGE_CURVE('',#9421,#9422,#5620,.T.);
#12210=EDGE_CURVE('',#9421,#9419,#466,.T.);
#12211=EDGE_CURVE('',#9422,#9420,#467,.T.);
#12212=EDGE_CURVE('',#9423,#9424,#5621,.T.);
#12213=EDGE_CURVE('',#9423,#9421,#468,.T.);
#12214=EDGE_CURVE('',#9424,#9422,#469,.T.);
#12215=EDGE_CURVE('',#9425,#9426,#5622,.T.);
#12216=EDGE_CURVE('',#9425,#9423,#470,.T.);
#12217=EDGE_CURVE('',#9426,#9424,#471,.T.);
#12218=EDGE_CURVE('',#9427,#9428,#5623,.T.);
#12219=EDGE_CURVE('',#9427,#9425,#472,.T.);
#12220=EDGE_CURVE('',#9428,#9426,#473,.T.);
#12221=EDGE_CURVE('',#9429,#9430,#5624,.T.);
#12222=EDGE_CURVE('',#9429,#9427,#474,.T.);
#12223=EDGE_CURVE('',#9430,#9428,#475,.T.);
#12224=EDGE_CURVE('',#9431,#9432,#5625,.T.);
#12225=EDGE_CURVE('',#9431,#9429,#476,.T.);
#12226=EDGE_CURVE('',#9432,#9430,#477,.T.);
#12227=EDGE_CURVE('',#9433,#9434,#5626,.T.);
#12228=EDGE_CURVE('',#9433,#9431,#478,.T.);
#12229=EDGE_CURVE('',#9434,#9432,#479,.T.);
#12230=EDGE_CURVE('',#9435,#9436,#5627,.T.);
#12231=EDGE_CURVE('',#9435,#9433,#480,.T.);
#12232=EDGE_CURVE('',#9436,#9434,#481,.T.);
#12233=EDGE_CURVE('',#9437,#9438,#5628,.T.);
#12234=EDGE_CURVE('',#9437,#9435,#482,.T.);
#12235=EDGE_CURVE('',#9438,#9436,#483,.T.);
#12236=EDGE_CURVE('',#9439,#9440,#5629,.T.);
#12237=EDGE_CURVE('',#9439,#9437,#484,.T.);
#12238=EDGE_CURVE('',#9440,#9438,#485,.T.);
#12239=EDGE_CURVE('',#9441,#9442,#5630,.T.);
#12240=EDGE_CURVE('',#9441,#9439,#486,.T.);
#12241=EDGE_CURVE('',#9442,#9440,#487,.T.);
#12242=EDGE_CURVE('',#9443,#9444,#5631,.T.);
#12243=EDGE_CURVE('',#9443,#9441,#488,.T.);
#12244=EDGE_CURVE('',#9444,#9442,#489,.T.);
#12245=EDGE_CURVE('',#9445,#9446,#5632,.T.);
#12246=EDGE_CURVE('',#9445,#9443,#490,.T.);
#12247=EDGE_CURVE('',#9446,#9444,#491,.T.);
#12248=EDGE_CURVE('',#9447,#9448,#5633,.T.);
#12249=EDGE_CURVE('',#9447,#9445,#492,.T.);
#12250=EDGE_CURVE('',#9448,#9446,#493,.T.);
#12251=EDGE_CURVE('',#9449,#9450,#5634,.T.);
#12252=EDGE_CURVE('',#9449,#9447,#494,.T.);
#12253=EDGE_CURVE('',#9450,#9448,#495,.T.);
#12254=EDGE_CURVE('',#9451,#9452,#5635,.T.);
#12255=EDGE_CURVE('',#9451,#9449,#496,.T.);
#12256=EDGE_CURVE('',#9452,#9450,#497,.T.);
#12257=EDGE_CURVE('',#9453,#9454,#5636,.T.);
#12258=EDGE_CURVE('',#9453,#9451,#498,.T.);
#12259=EDGE_CURVE('',#9454,#9452,#499,.T.);
#12260=EDGE_CURVE('',#9455,#9456,#5637,.T.);
#12261=EDGE_CURVE('',#9455,#9453,#500,.T.);
#12262=EDGE_CURVE('',#9456,#9454,#501,.T.);
#12263=EDGE_CURVE('',#9457,#9458,#5638,.T.);
#12264=EDGE_CURVE('',#9457,#9455,#502,.T.);
#12265=EDGE_CURVE('',#9458,#9456,#503,.T.);
#12266=EDGE_CURVE('',#9459,#9460,#5639,.T.);
#12267=EDGE_CURVE('',#9459,#9457,#504,.T.);
#12268=EDGE_CURVE('',#9460,#9458,#505,.T.);
#12269=EDGE_CURVE('',#9461,#9462,#5640,.T.);
#12270=EDGE_CURVE('',#9461,#9459,#506,.T.);
#12271=EDGE_CURVE('',#9462,#9460,#507,.T.);
#12272=EDGE_CURVE('',#9463,#9464,#5641,.T.);
#12273=EDGE_CURVE('',#9463,#9461,#508,.T.);
#12274=EDGE_CURVE('',#9464,#9462,#509,.T.);
#12275=EDGE_CURVE('',#9465,#9466,#5642,.T.);
#12276=EDGE_CURVE('',#9465,#9463,#510,.T.);
#12277=EDGE_CURVE('',#9466,#9464,#511,.T.);
#12278=EDGE_CURVE('',#9467,#9468,#5643,.T.);
#12279=EDGE_CURVE('',#9467,#9465,#512,.T.);
#12280=EDGE_CURVE('',#9468,#9466,#513,.T.);
#12281=EDGE_CURVE('',#9469,#9469,#3867,.T.);
#12282=EDGE_CURVE('',#9469,#9470,#5644,.T.);
#12283=EDGE_CURVE('',#9470,#9470,#3868,.T.);
#12284=EDGE_CURVE('',#9469,#9471,#5645,.T.);
#12285=EDGE_CURVE('',#9471,#9471,#3869,.T.);
#12286=EDGE_CURVE('',#9472,#9472,#3870,.T.);
#12287=EDGE_CURVE('',#9472,#9473,#5646,.T.);
#12288=EDGE_CURVE('',#9473,#9473,#3871,.T.);
#12289=EDGE_CURVE('',#9473,#9474,#5647,.T.);
#12290=EDGE_CURVE('',#9474,#9474,#3872,.T.);
#12291=EDGE_CURVE('',#9270,#9475,#514,.T.);
#12292=EDGE_CURVE('',#9219,#9269,#515,.T.);
#12293=EDGE_CURVE('',#9475,#9217,#3873,.T.);
#12294=EDGE_CURVE('',#9476,#9467,#516,.T.);
#12295=EDGE_CURVE('',#9017,#9476,#517,.T.);
#12296=EDGE_CURVE('',#9477,#9468,#518,.T.);
#12297=EDGE_CURVE('',#9476,#9477,#3874,.T.);
#12298=EDGE_CURVE('',#9247,#9244,#519,.F.);
#12299=EDGE_CURVE('',#9242,#9478,#3875,.F.);
#12300=EDGE_CURVE('',#9478,#9248,#520,.F.);
#12301=EDGE_CURVE('',#9479,#9266,#521,.T.);
#12302=EDGE_CURVE('',#9243,#9478,#522,.F.);
#12303=EDGE_CURVE('',#9479,#9225,#523,.F.);
#12304=EDGE_CURVE('',#9224,#9480,#524,.F.);
#12305=EDGE_CURVE('',#9480,#9479,#3876,.T.);
#12306=EDGE_CURVE('',#9480,#9265,#525,.T.);
#12307=EDGE_CURVE('',#9477,#9018,#526,.T.);
#12308=EDGE_CURVE('',#9218,#9475,#527,.T.);
#12309=EDGE_CURVE('',#9481,#9482,#3877,.T.);
#12310=EDGE_CURVE('',#9483,#9481,#5648,.T.);
#12311=EDGE_CURVE('',#9484,#9483,#3878,.T.);
#12312=EDGE_CURVE('',#9485,#9484,#5649,.T.);
#12313=EDGE_CURVE('',#9486,#9485,#5650,.T.);
#12314=EDGE_CURVE('',#9486,#9482,#5651,.T.);
#12315=EDGE_CURVE('',#9487,#9487,#3879,.T.);
#12316=EDGE_CURVE('',#9488,#9488,#3880,.T.);
#12317=EDGE_CURVE('',#9488,#9489,#5652,.T.);
#12318=EDGE_CURVE('',#9489,#9489,#3881,.T.);
#12319=EDGE_CURVE('',#9490,#9490,#3882,.T.);
#12320=EDGE_CURVE('',#9490,#9491,#5653,.T.);
#12321=EDGE_CURVE('',#9491,#9491,#3883,.T.);
#12322=EDGE_CURVE('',#9492,#9492,#3884,.T.);
#12323=EDGE_CURVE('',#9492,#9493,#5654,.T.);
#12324=EDGE_CURVE('',#9493,#9493,#3885,.T.);
#12325=EDGE_CURVE('',#9494,#9494,#3886,.T.);
#12326=EDGE_CURVE('',#9494,#9495,#5655,.T.);
#12327=EDGE_CURVE('',#9495,#9495,#3887,.T.);
#12328=EDGE_CURVE('',#9496,#9496,#3888,.T.);
#12329=EDGE_CURVE('',#9496,#9497,#5656,.T.);
#12330=EDGE_CURVE('',#9497,#9497,#3889,.T.);
#12331=EDGE_CURVE('',#9498,#9498,#3890,.T.);
#12332=EDGE_CURVE('',#9498,#9499,#5657,.T.);
#12333=EDGE_CURVE('',#9499,#9499,#3891,.T.);
#12334=EDGE_CURVE('',#9500,#9500,#3892,.T.);
#12335=EDGE_CURVE('',#9500,#9501,#5658,.T.);
#12336=EDGE_CURVE('',#9501,#9501,#3893,.T.);
#12337=EDGE_CURVE('',#9502,#9502,#3894,.T.);
#12338=EDGE_CURVE('',#9502,#9503,#5659,.T.);
#12339=EDGE_CURVE('',#9503,#9503,#3895,.T.);
#12340=EDGE_CURVE('',#9504,#9504,#3896,.T.);
#12341=EDGE_CURVE('',#9504,#9505,#5660,.T.);
#12342=EDGE_CURVE('',#9505,#9505,#3897,.T.);
#12343=EDGE_CURVE('',#9506,#9506,#3898,.T.);
#12344=EDGE_CURVE('',#9506,#9507,#5661,.T.);
#12345=EDGE_CURVE('',#9507,#9507,#3899,.T.);
#12346=EDGE_CURVE('',#9508,#9508,#3900,.T.);
#12347=EDGE_CURVE('',#9508,#9509,#5662,.T.);
#12348=EDGE_CURVE('',#9509,#9509,#3901,.T.);
#12349=EDGE_CURVE('',#9510,#9510,#3902,.T.);
#12350=EDGE_CURVE('',#9510,#9511,#5663,.T.);
#12351=EDGE_CURVE('',#9511,#9511,#3903,.T.);
#12352=EDGE_CURVE('',#9512,#9512,#3904,.T.);
#12353=EDGE_CURVE('',#9512,#9513,#5664,.T.);
#12354=EDGE_CURVE('',#9513,#9513,#3905,.T.);
#12355=EDGE_CURVE('',#9514,#9514,#3906,.T.);
#12356=EDGE_CURVE('',#9514,#9515,#5665,.T.);
#12357=EDGE_CURVE('',#9515,#9515,#3907,.T.);
#12358=EDGE_CURVE('',#9516,#9516,#3908,.T.);
#12359=EDGE_CURVE('',#9516,#9517,#5666,.T.);
#12360=EDGE_CURVE('',#9517,#9517,#3909,.T.);
#12361=EDGE_CURVE('',#9518,#9518,#3910,.T.);
#12362=EDGE_CURVE('',#9518,#9519,#5667,.T.);
#12363=EDGE_CURVE('',#9519,#9519,#3911,.T.);
#12364=EDGE_CURVE('',#9520,#9520,#3912,.T.);
#12365=EDGE_CURVE('',#9520,#9487,#5668,.T.);
#12366=EDGE_CURVE('',#9521,#9522,#3913,.T.);
#12367=EDGE_CURVE('',#9522,#9481,#5669,.T.);
#12368=EDGE_CURVE('',#9482,#9521,#5670,.T.);
#12369=EDGE_CURVE('',#9522,#9523,#5671,.T.);
#12370=EDGE_CURVE('',#9483,#9523,#5672,.T.);
#12371=EDGE_CURVE('',#9523,#9524,#3914,.T.);
#12372=EDGE_CURVE('',#9524,#9484,#5673,.T.);
#12373=EDGE_CURVE('',#9525,#9524,#5674,.T.);
#12374=EDGE_CURVE('',#9485,#9525,#5675,.T.);
#12375=EDGE_CURVE('',#9526,#9521,#5676,.T.);
#12376=EDGE_CURVE('',#9525,#9526,#5677,.T.);
#12377=EDGE_CURVE('',#9526,#9486,#5678,.T.);
#12378=EDGE_CURVE('',#9527,#9528,#5679,.T.);
#12379=EDGE_CURVE('',#9527,#9529,#5680,.T.);
#12380=EDGE_CURVE('',#9530,#9529,#5681,.T.);
#12381=EDGE_CURVE('',#9528,#9530,#5682,.T.);
#12382=EDGE_CURVE('',#9531,#9527,#5683,.T.);
#12383=EDGE_CURVE('',#9531,#9532,#5684,.T.);
#12384=EDGE_CURVE('',#9529,#9532,#5685,.T.);
#12385=EDGE_CURVE('',#9533,#9531,#5686,.T.);
#12386=EDGE_CURVE('',#9534,#9533,#5687,.T.);
#12387=EDGE_CURVE('',#9532,#9534,#5688,.T.);
#12388=EDGE_CURVE('',#9535,#9530,#5689,.T.);
#12389=EDGE_CURVE('',#9536,#9535,#5690,.T.);
#12390=EDGE_CURVE('',#9528,#9536,#5691,.T.);
#12391=EDGE_CURVE('',#9537,#9533,#5692,.T.);
#12392=EDGE_CURVE('',#9538,#9537,#5693,.T.);
#12393=EDGE_CURVE('',#9534,#9538,#5694,.T.);
#12394=EDGE_CURVE('',#9536,#9539,#5695,.T.);
#12395=EDGE_CURVE('',#9540,#9539,#5696,.T.);
#12396=EDGE_CURVE('',#9537,#9540,#5697,.T.);
#12397=EDGE_CURVE('',#9538,#9541,#5698,.T.);
#12398=EDGE_CURVE('',#9542,#9541,#5699,.T.);
#12399=EDGE_CURVE('',#9535,#9542,#5700,.T.);
#12400=EDGE_CURVE('',#9539,#9542,#5701,.T.);
#12401=EDGE_CURVE('',#9541,#9540,#5702,.T.);
#12402=EDGE_CURVE('',#9543,#9544,#5703,.T.);
#12403=EDGE_CURVE('',#9545,#9543,#5704,.T.);
#12404=EDGE_CURVE('',#9546,#9545,#5705,.T.);
#12405=EDGE_CURVE('',#9544,#9546,#5706,.T.);
#12406=EDGE_CURVE('',#9547,#9545,#3915,.T.);
#12407=EDGE_CURVE('',#9548,#9547,#5707,.T.);
#12408=EDGE_CURVE('',#9546,#9548,#3916,.T.);
#12409=EDGE_CURVE('',#9549,#9547,#3917,.T.);
#12410=EDGE_CURVE('',#9550,#9549,#5708,.T.);
#12411=EDGE_CURVE('',#9548,#9550,#3918,.T.);
#12412=EDGE_CURVE('',#9551,#9549,#3919,.T.);
#12413=EDGE_CURVE('',#9552,#9551,#5709,.T.);
#12414=EDGE_CURVE('',#9550,#9552,#3920,.T.);
#12415=EDGE_CURVE('',#9553,#9551,#5710,.T.);
#12416=EDGE_CURVE('',#9554,#9553,#5711,.T.);
#12417=EDGE_CURVE('',#9552,#9554,#5712,.T.);
#12418=EDGE_CURVE('',#9555,#9553,#3921,.T.);
#12419=EDGE_CURVE('',#9556,#9555,#5713,.T.);
#12420=EDGE_CURVE('',#9554,#9556,#3922,.T.);
#12421=EDGE_CURVE('',#9557,#9555,#3923,.T.);
#12422=EDGE_CURVE('',#9558,#9557,#5714,.T.);
#12423=EDGE_CURVE('',#9556,#9558,#3924,.T.);
#12424=EDGE_CURVE('',#9559,#9557,#3925,.T.);
#12425=EDGE_CURVE('',#9560,#9559,#5715,.T.);
#12426=EDGE_CURVE('',#9558,#9560,#3926,.T.);
#12427=EDGE_CURVE('',#9561,#9559,#5716,.T.);
#12428=EDGE_CURVE('',#9562,#9561,#5717,.T.);
#12429=EDGE_CURVE('',#9560,#9562,#5718,.T.);
#12430=EDGE_CURVE('',#9563,#9561,#3927,.T.);
#12431=EDGE_CURVE('',#9564,#9563,#5719,.T.);
#12432=EDGE_CURVE('',#9562,#9564,#3928,.T.);
#12433=EDGE_CURVE('',#9565,#9563,#5720,.T.);
#12434=EDGE_CURVE('',#9566,#9565,#5721,.T.);
#12435=EDGE_CURVE('',#9564,#9566,#5722,.T.);
#12436=EDGE_CURVE('',#9567,#9565,#3929,.T.);
#12437=EDGE_CURVE('',#9568,#9567,#5723,.T.);
#12438=EDGE_CURVE('',#9566,#9568,#3930,.T.);
#12439=EDGE_CURVE('',#9569,#9567,#5724,.T.);
#12440=EDGE_CURVE('',#9570,#9569,#5725,.T.);
#12441=EDGE_CURVE('',#9568,#9570,#5726,.T.);
#12442=EDGE_CURVE('',#9571,#9569,#3931,.T.);
#12443=EDGE_CURVE('',#9572,#9571,#5727,.T.);
#12444=EDGE_CURVE('',#9570,#9572,#3932,.T.);
#12445=EDGE_CURVE('',#9573,#9571,#5728,.T.);
#12446=EDGE_CURVE('',#9574,#9573,#5729,.T.);
#12447=EDGE_CURVE('',#9572,#9574,#5730,.T.);
#12448=EDGE_CURVE('',#9575,#9573,#5731,.T.);
#12449=EDGE_CURVE('',#9576,#9575,#5732,.T.);
#12450=EDGE_CURVE('',#9574,#9576,#5733,.T.);
#12451=EDGE_CURVE('',#9577,#9544,#5734,.T.);
#12452=EDGE_CURVE('',#9578,#9576,#5735,.T.);
#12453=EDGE_CURVE('',#9579,#9578,#5736,.T.);
#12454=EDGE_CURVE('',#9580,#9579,#5737,.T.);
#12455=EDGE_CURVE('',#9581,#9580,#3933,.T.);
#12456=EDGE_CURVE('',#9582,#9581,#5738,.T.);
#12457=EDGE_CURVE('',#9583,#9582,#3934,.T.);
#12458=EDGE_CURVE('',#9584,#9583,#5739,.T.);
#12459=EDGE_CURVE('',#9585,#9584,#3935,.T.);
#12460=EDGE_CURVE('',#9586,#9585,#5740,.T.);
#12461=EDGE_CURVE('',#9587,#9586,#3936,.T.);
#12462=EDGE_CURVE('',#9588,#9587,#3937,.T.);
#12463=EDGE_CURVE('',#9589,#9588,#3938,.T.);
#12464=EDGE_CURVE('',#9590,#9589,#5741,.T.);
#12465=EDGE_CURVE('',#9591,#9590,#3939,.T.);
#12466=EDGE_CURVE('',#9592,#9591,#3940,.T.);
#12467=EDGE_CURVE('',#9593,#9592,#3941,.T.);
#12468=EDGE_CURVE('',#9577,#9593,#5742,.T.);
#12469=EDGE_CURVE('',#9594,#9577,#5743,.T.);
#12470=EDGE_CURVE('',#9593,#9595,#5744,.T.);
#12471=EDGE_CURVE('',#9595,#9594,#5745,.T.);
#12472=EDGE_CURVE('',#9592,#9596,#5746,.T.);
#12473=EDGE_CURVE('',#9596,#9595,#3942,.T.);
#12474=EDGE_CURVE('',#9591,#9597,#5747,.T.);
#12475=EDGE_CURVE('',#9597,#9596,#3943,.T.);
#12476=EDGE_CURVE('',#9590,#9598,#5748,.T.);
#12477=EDGE_CURVE('',#9598,#9597,#3944,.T.);
#12478=EDGE_CURVE('',#9589,#9599,#5749,.T.);
#12479=EDGE_CURVE('',#9599,#9598,#5750,.T.);
#12480=EDGE_CURVE('',#9588,#9600,#5751,.T.);
#12481=EDGE_CURVE('',#9600,#9599,#3945,.T.);
#12482=EDGE_CURVE('',#9587,#9601,#5752,.T.);
#12483=EDGE_CURVE('',#9601,#9600,#3946,.T.);
#12484=EDGE_CURVE('',#9586,#9602,#5753,.T.);
#12485=EDGE_CURVE('',#9602,#9601,#3947,.T.);
#12486=EDGE_CURVE('',#9585,#9603,#5754,.T.);
#12487=EDGE_CURVE('',#9603,#9602,#5755,.T.);
#12488=EDGE_CURVE('',#9584,#9604,#5756,.T.);
#12489=EDGE_CURVE('',#9604,#9603,#3948,.T.);
#12490=EDGE_CURVE('',#9583,#9605,#5757,.T.);
#12491=EDGE_CURVE('',#9605,#9604,#5758,.T.);
#12492=EDGE_CURVE('',#9582,#9606,#5759,.T.);
#12493=EDGE_CURVE('',#9606,#9605,#3949,.T.);
#12494=EDGE_CURVE('',#9581,#9607,#5760,.T.);
#12495=EDGE_CURVE('',#9607,#9606,#5761,.T.);
#12496=EDGE_CURVE('',#9580,#9608,#5762,.T.);
#12497=EDGE_CURVE('',#9608,#9607,#3950,.T.);
#12498=EDGE_CURVE('',#9579,#9609,#5763,.T.);
#12499=EDGE_CURVE('',#9609,#9608,#5764,.T.);
#12500=EDGE_CURVE('',#9578,#9610,#5765,.T.);
#12501=EDGE_CURVE('',#9610,#9609,#5766,.T.);
#12502=EDGE_CURVE('',#9610,#9575,#5767,.T.);
#12503=EDGE_CURVE('',#9594,#9543,#5768,.T.);
#12504=EDGE_CURVE('',#9611,#9611,#3951,.T.);
#12505=EDGE_CURVE('',#9611,#9612,#5769,.T.);
#12506=EDGE_CURVE('',#9612,#9612,#3952,.T.);
#12507=EDGE_CURVE('',#9613,#9614,#5770,.T.);
#12508=EDGE_CURVE('',#9613,#9615,#5771,.T.);
#12509=EDGE_CURVE('',#9616,#9615,#5772,.T.);
#12510=EDGE_CURVE('',#9614,#9616,#5773,.T.);
#12511=EDGE_CURVE('',#9614,#9617,#5774,.T.);
#12512=EDGE_CURVE('',#9618,#9616,#5775,.T.);
#12513=EDGE_CURVE('',#9617,#9618,#5776,.T.);
#12514=EDGE_CURVE('',#9617,#9619,#5777,.T.);
#12515=EDGE_CURVE('',#9620,#9618,#5778,.T.);
#12516=EDGE_CURVE('',#9619,#9620,#5779,.T.);
#12517=EDGE_CURVE('',#9619,#9613,#5780,.T.);
#12518=EDGE_CURVE('',#9615,#9620,#5781,.T.);
#12519=EDGE_CURVE('',#9621,#9621,#3953,.T.);
#12520=EDGE_CURVE('',#9621,#9622,#5782,.T.);
#12521=EDGE_CURVE('',#9622,#9622,#3954,.F.);
#12522=EDGE_CURVE('',#9623,#9624,#5783,.T.);
#12523=EDGE_CURVE('',#9623,#9625,#5784,.F.);
#12524=EDGE_CURVE('',#9626,#9625,#5785,.T.);
#12525=EDGE_CURVE('',#9624,#9626,#5786,.T.);
#12526=EDGE_CURVE('',#9624,#9627,#5787,.T.);
#12527=EDGE_CURVE('',#9628,#9626,#5788,.T.);
#12528=EDGE_CURVE('',#9627,#9628,#5789,.T.);
#12529=EDGE_CURVE('',#9627,#9629,#5790,.T.);
#12530=EDGE_CURVE('',#9630,#9628,#5791,.T.);
#12531=EDGE_CURVE('',#9629,#9630,#5792,.T.);
#12532=EDGE_CURVE('',#9629,#9623,#5793,.T.);
#12533=EDGE_CURVE('',#9625,#9630,#5794,.F.);
#12534=EDGE_CURVE('',#9631,#9631,#3955,.T.);
#12535=EDGE_CURVE('',#9631,#9632,#5795,.T.);
#12536=EDGE_CURVE('',#9632,#9632,#3956,.T.);
#12537=EDGE_CURVE('',#9633,#9634,#5796,.T.);
#12538=EDGE_CURVE('',#9634,#9635,#5797,.T.);
#12539=EDGE_CURVE('',#9636,#9635,#5798,.T.);
#12540=EDGE_CURVE('',#9633,#9636,#5799,.T.);
#12541=EDGE_CURVE('',#9637,#9633,#5800,.T.);
#12542=EDGE_CURVE('',#9638,#9636,#5801,.T.);
#12543=EDGE_CURVE('',#9637,#9638,#5802,.T.);
#12544=EDGE_CURVE('',#9639,#9637,#5803,.T.);
#12545=EDGE_CURVE('',#9640,#9638,#5804,.T.);
#12546=EDGE_CURVE('',#9639,#9640,#5805,.T.);
#12547=EDGE_CURVE('',#9634,#9639,#5806,.T.);
#12548=EDGE_CURVE('',#9635,#9640,#5807,.T.);
#12549=EDGE_CURVE('',#9641,#9642,#5808,.T.);
#12550=EDGE_CURVE('',#9642,#9643,#5809,.T.);
#12551=EDGE_CURVE('',#9643,#9644,#5810,.T.);
#12552=EDGE_CURVE('',#9644,#9641,#5811,.T.);
#12553=EDGE_CURVE('',#9643,#9645,#3957,.T.);
#12554=EDGE_CURVE('',#9645,#9646,#5812,.T.);
#12555=EDGE_CURVE('',#9646,#9644,#3958,.T.);
#12556=EDGE_CURVE('',#9645,#9647,#3959,.T.);
#12557=EDGE_CURVE('',#9647,#9648,#5813,.T.);
#12558=EDGE_CURVE('',#9648,#9646,#3960,.T.);
#12559=EDGE_CURVE('',#9647,#9649,#3961,.T.);
#12560=EDGE_CURVE('',#9649,#9650,#5814,.T.);
#12561=EDGE_CURVE('',#9650,#9648,#3962,.T.);
#12562=EDGE_CURVE('',#9649,#9651,#5815,.T.);
#12563=EDGE_CURVE('',#9651,#9652,#5816,.T.);
#12564=EDGE_CURVE('',#9652,#9650,#5817,.T.);
#12565=EDGE_CURVE('',#9651,#9653,#3963,.T.);
#12566=EDGE_CURVE('',#9653,#9654,#5818,.T.);
#12567=EDGE_CURVE('',#9654,#9652,#3964,.T.);
#12568=EDGE_CURVE('',#9653,#9655,#3965,.T.);
#12569=EDGE_CURVE('',#9655,#9656,#5819,.T.);
#12570=EDGE_CURVE('',#9656,#9654,#3966,.T.);
#12571=EDGE_CURVE('',#9655,#9657,#3967,.T.);
#12572=EDGE_CURVE('',#9657,#9658,#5820,.T.);
#12573=EDGE_CURVE('',#9658,#9656,#3968,.T.);
#12574=EDGE_CURVE('',#9657,#9659,#5821,.T.);
#12575=EDGE_CURVE('',#9659,#9660,#5822,.T.);
#12576=EDGE_CURVE('',#9660,#9658,#5823,.T.);
#12577=EDGE_CURVE('',#9659,#9661,#3969,.T.);
#12578=EDGE_CURVE('',#9661,#9662,#5824,.T.);
#12579=EDGE_CURVE('',#9662,#9660,#3970,.T.);
#12580=EDGE_CURVE('',#9661,#9663,#5825,.T.);
#12581=EDGE_CURVE('',#9663,#9664,#5826,.T.);
#12582=EDGE_CURVE('',#9664,#9662,#5827,.T.);
#12583=EDGE_CURVE('',#9663,#9665,#3971,.T.);
#12584=EDGE_CURVE('',#9665,#9666,#5828,.T.);
#12585=EDGE_CURVE('',#9666,#9664,#3972,.T.);
#12586=EDGE_CURVE('',#9665,#9667,#5829,.T.);
#12587=EDGE_CURVE('',#9667,#9668,#5830,.T.);
#12588=EDGE_CURVE('',#9668,#9666,#5831,.T.);
#12589=EDGE_CURVE('',#9667,#9669,#3973,.T.);
#12590=EDGE_CURVE('',#9669,#9670,#5832,.T.);
#12591=EDGE_CURVE('',#9670,#9668,#3974,.T.);
#12592=EDGE_CURVE('',#9669,#9671,#5833,.T.);
#12593=EDGE_CURVE('',#9671,#9672,#5834,.T.);
#12594=EDGE_CURVE('',#9672,#9670,#5835,.T.);
#12595=EDGE_CURVE('',#9671,#9673,#5836,.T.);
#12596=EDGE_CURVE('',#9673,#9674,#5837,.T.);
#12597=EDGE_CURVE('',#9674,#9672,#5838,.T.);
#12598=EDGE_CURVE('',#9675,#9642,#5839,.T.);
#12599=EDGE_CURVE('',#9675,#9676,#5840,.T.);
#12600=EDGE_CURVE('',#9676,#9677,#3975,.T.);
#12601=EDGE_CURVE('',#9677,#9678,#3976,.T.);
#12602=EDGE_CURVE('',#9678,#9679,#3977,.T.);
#12603=EDGE_CURVE('',#9679,#9680,#5841,.T.);
#12604=EDGE_CURVE('',#9680,#9681,#3978,.T.);
#12605=EDGE_CURVE('',#9681,#9682,#3979,.T.);
#12606=EDGE_CURVE('',#9682,#9683,#3980,.T.);
#12607=EDGE_CURVE('',#9683,#9684,#5842,.T.);
#12608=EDGE_CURVE('',#9684,#9685,#3981,.T.);
#12609=EDGE_CURVE('',#9685,#9686,#5843,.T.);
#12610=EDGE_CURVE('',#9686,#9687,#3982,.T.);
#12611=EDGE_CURVE('',#9687,#9688,#5844,.T.);
#12612=EDGE_CURVE('',#9688,#9689,#3983,.T.);
#12613=EDGE_CURVE('',#9689,#9690,#5845,.T.);
#12614=EDGE_CURVE('',#9690,#9691,#5846,.T.);
#12615=EDGE_CURVE('',#9691,#9673,#5847,.T.);
#12616=EDGE_CURVE('',#9692,#9675,#5848,.T.);
#12617=EDGE_CURVE('',#9693,#9692,#5849,.T.);
#12618=EDGE_CURVE('',#9676,#9693,#5850,.T.);
#12619=EDGE_CURVE('',#9694,#9693,#3984,.T.);
#12620=EDGE_CURVE('',#9677,#9694,#5851,.T.);
#12621=EDGE_CURVE('',#9695,#9694,#3985,.T.);
#12622=EDGE_CURVE('',#9678,#9695,#5852,.T.);
#12623=EDGE_CURVE('',#9696,#9695,#3986,.T.);
#12624=EDGE_CURVE('',#9679,#9696,#5853,.T.);
#12625=EDGE_CURVE('',#9697,#9696,#5854,.T.);
#12626=EDGE_CURVE('',#9680,#9697,#5855,.T.);
#12627=EDGE_CURVE('',#9698,#9697,#3987,.T.);
#12628=EDGE_CURVE('',#9681,#9698,#5856,.T.);
#12629=EDGE_CURVE('',#9699,#9698,#3988,.T.);
#12630=EDGE_CURVE('',#9682,#9699,#5857,.T.);
#12631=EDGE_CURVE('',#9700,#9699,#3989,.T.);
#12632=EDGE_CURVE('',#9683,#9700,#5858,.T.);
#12633=EDGE_CURVE('',#9701,#9700,#5859,.T.);
#12634=EDGE_CURVE('',#9684,#9701,#5860,.T.);
#12635=EDGE_CURVE('',#9702,#9701,#3990,.T.);
#12636=EDGE_CURVE('',#9685,#9702,#5861,.T.);
#12637=EDGE_CURVE('',#9703,#9702,#5862,.T.);
#12638=EDGE_CURVE('',#9686,#9703,#5863,.T.);
#12639=EDGE_CURVE('',#9704,#9703,#3991,.T.);
#12640=EDGE_CURVE('',#9687,#9704,#5864,.T.);
#12641=EDGE_CURVE('',#9705,#9704,#5865,.T.);
#12642=EDGE_CURVE('',#9688,#9705,#5866,.T.);
#12643=EDGE_CURVE('',#9706,#9705,#3992,.T.);
#12644=EDGE_CURVE('',#9689,#9706,#5867,.T.);
#12645=EDGE_CURVE('',#9707,#9706,#5868,.T.);
#12646=EDGE_CURVE('',#9690,#9707,#5869,.T.);
#12647=EDGE_CURVE('',#9708,#9707,#5870,.T.);
#12648=EDGE_CURVE('',#9691,#9708,#5871,.T.);
#12649=EDGE_CURVE('',#9708,#9674,#5872,.T.);
#12650=EDGE_CURVE('',#9692,#9641,#5873,.T.);
#12651=ORIENTED_EDGE('',*,*,#9709,.T.);
#12652=ORIENTED_EDGE('',*,*,#9710,.T.);
#12653=ORIENTED_EDGE('',*,*,#9711,.T.);
#12654=ORIENTED_EDGE('',*,*,#9712,.T.);
#12655=ORIENTED_EDGE('',*,*,#9713,.T.);
#12656=ORIENTED_EDGE('',*,*,#9714,.T.);
#12657=ORIENTED_EDGE('',*,*,#9715,.T.);
#12658=ORIENTED_EDGE('',*,*,#9716,.T.);
#12659=ORIENTED_EDGE('',*,*,#9717,.T.);
#12660=ORIENTED_EDGE('',*,*,#9718,.T.);
#12661=ORIENTED_EDGE('',*,*,#9719,.T.);
#12662=ORIENTED_EDGE('',*,*,#9720,.T.);
#12663=ORIENTED_EDGE('',*,*,#9721,.T.);
#12664=ORIENTED_EDGE('',*,*,#9722,.T.);
#12665=ORIENTED_EDGE('',*,*,#9723,.T.);
#12666=ORIENTED_EDGE('',*,*,#9724,.T.);
#12667=ORIENTED_EDGE('',*,*,#9725,.T.);
#12668=ORIENTED_EDGE('',*,*,#9726,.T.);
#12669=ORIENTED_EDGE('',*,*,#9727,.T.);
#12670=ORIENTED_EDGE('',*,*,#9728,.T.);
#12671=ORIENTED_EDGE('',*,*,#9729,.T.);
#12672=ORIENTED_EDGE('',*,*,#9730,.T.);
#12673=ORIENTED_EDGE('',*,*,#9731,.T.);
#12674=ORIENTED_EDGE('',*,*,#9732,.T.);
#12675=ORIENTED_EDGE('',*,*,#9733,.T.);
#12676=ORIENTED_EDGE('',*,*,#9734,.T.);
#12677=ORIENTED_EDGE('',*,*,#9735,.T.);
#12678=ORIENTED_EDGE('',*,*,#9736,.T.);
#12679=ORIENTED_EDGE('',*,*,#9737,.T.);
#12680=ORIENTED_EDGE('',*,*,#9738,.T.);
#12681=ORIENTED_EDGE('',*,*,#9739,.T.);
#12682=ORIENTED_EDGE('',*,*,#9740,.T.);
#12683=ORIENTED_EDGE('',*,*,#9741,.T.);
#12684=ORIENTED_EDGE('',*,*,#9742,.T.);
#12685=ORIENTED_EDGE('',*,*,#9743,.T.);
#12686=ORIENTED_EDGE('',*,*,#9744,.T.);
#12687=ORIENTED_EDGE('',*,*,#9726,.F.);
#12688=ORIENTED_EDGE('',*,*,#9745,.T.);
#12689=ORIENTED_EDGE('',*,*,#9746,.T.);
#12690=ORIENTED_EDGE('',*,*,#9747,.F.);
#12691=ORIENTED_EDGE('',*,*,#9727,.F.);
#12692=ORIENTED_EDGE('',*,*,#9747,.T.);
#12693=ORIENTED_EDGE('',*,*,#9748,.T.);
#12694=ORIENTED_EDGE('',*,*,#9749,.F.);
#12695=ORIENTED_EDGE('',*,*,#9728,.F.);
#12696=ORIENTED_EDGE('',*,*,#9749,.T.);
#12697=ORIENTED_EDGE('',*,*,#9750,.T.);
#12698=ORIENTED_EDGE('',*,*,#9751,.F.);
#12699=ORIENTED_EDGE('',*,*,#9729,.F.);
#12700=ORIENTED_EDGE('',*,*,#9751,.T.);
#12701=ORIENTED_EDGE('',*,*,#9752,.T.);
#12702=ORIENTED_EDGE('',*,*,#9753,.F.);
#12703=ORIENTED_EDGE('',*,*,#9730,.F.);
#12704=ORIENTED_EDGE('',*,*,#9753,.T.);
#12705=ORIENTED_EDGE('',*,*,#9754,.T.);
#12706=ORIENTED_EDGE('',*,*,#9755,.F.);
#12707=ORIENTED_EDGE('',*,*,#9731,.F.);
#12708=ORIENTED_EDGE('',*,*,#9755,.T.);
#12709=ORIENTED_EDGE('',*,*,#9756,.T.);
#12710=ORIENTED_EDGE('',*,*,#9757,.F.);
#12711=ORIENTED_EDGE('',*,*,#9732,.F.);
#12712=ORIENTED_EDGE('',*,*,#9757,.T.);
#12713=ORIENTED_EDGE('',*,*,#9758,.T.);
#12714=ORIENTED_EDGE('',*,*,#9759,.F.);
#12715=ORIENTED_EDGE('',*,*,#9733,.F.);
#12716=ORIENTED_EDGE('',*,*,#9759,.T.);
#12717=ORIENTED_EDGE('',*,*,#9760,.T.);
#12718=ORIENTED_EDGE('',*,*,#9761,.F.);
#12719=ORIENTED_EDGE('',*,*,#9734,.F.);
#12720=ORIENTED_EDGE('',*,*,#9761,.T.);
#12721=ORIENTED_EDGE('',*,*,#9762,.T.);
#12722=ORIENTED_EDGE('',*,*,#9763,.F.);
#12723=ORIENTED_EDGE('',*,*,#9735,.F.);
#12724=ORIENTED_EDGE('',*,*,#9763,.T.);
#12725=ORIENTED_EDGE('',*,*,#9764,.T.);
#12726=ORIENTED_EDGE('',*,*,#9765,.F.);
#12727=ORIENTED_EDGE('',*,*,#9736,.F.);
#12728=ORIENTED_EDGE('',*,*,#9765,.T.);
#12729=ORIENTED_EDGE('',*,*,#9766,.T.);
#12730=ORIENTED_EDGE('',*,*,#9767,.F.);
#12731=ORIENTED_EDGE('',*,*,#9737,.F.);
#12732=ORIENTED_EDGE('',*,*,#9767,.T.);
#12733=ORIENTED_EDGE('',*,*,#9768,.T.);
#12734=ORIENTED_EDGE('',*,*,#9769,.F.);
#12735=ORIENTED_EDGE('',*,*,#9738,.F.);
#12736=ORIENTED_EDGE('',*,*,#9769,.T.);
#12737=ORIENTED_EDGE('',*,*,#9770,.T.);
#12738=ORIENTED_EDGE('',*,*,#9771,.F.);
#12739=ORIENTED_EDGE('',*,*,#9739,.F.);
#12740=ORIENTED_EDGE('',*,*,#9771,.T.);
#12741=ORIENTED_EDGE('',*,*,#9772,.T.);
#12742=ORIENTED_EDGE('',*,*,#9773,.F.);
#12743=ORIENTED_EDGE('',*,*,#9740,.F.);
#12744=ORIENTED_EDGE('',*,*,#9773,.T.);
#12745=ORIENTED_EDGE('',*,*,#9774,.T.);
#12746=ORIENTED_EDGE('',*,*,#9775,.F.);
#12747=ORIENTED_EDGE('',*,*,#9741,.F.);
#12748=ORIENTED_EDGE('',*,*,#9775,.T.);
#12749=ORIENTED_EDGE('',*,*,#9776,.T.);
#12750=ORIENTED_EDGE('',*,*,#9777,.F.);
#12751=ORIENTED_EDGE('',*,*,#9709,.F.);
#12752=ORIENTED_EDGE('',*,*,#9778,.T.);
#12753=ORIENTED_EDGE('',*,*,#9779,.T.);
#12754=ORIENTED_EDGE('',*,*,#9780,.F.);
#12755=ORIENTED_EDGE('',*,*,#9710,.F.);
#12756=ORIENTED_EDGE('',*,*,#9780,.T.);
#12757=ORIENTED_EDGE('',*,*,#9781,.T.);
#12758=ORIENTED_EDGE('',*,*,#9782,.F.);
#12759=ORIENTED_EDGE('',*,*,#9711,.F.);
#12760=ORIENTED_EDGE('',*,*,#9782,.T.);
#12761=ORIENTED_EDGE('',*,*,#9783,.T.);
#12762=ORIENTED_EDGE('',*,*,#9784,.F.);
#12763=ORIENTED_EDGE('',*,*,#9712,.F.);
#12764=ORIENTED_EDGE('',*,*,#9784,.T.);
#12765=ORIENTED_EDGE('',*,*,#9785,.T.);
#12766=ORIENTED_EDGE('',*,*,#9786,.F.);
#12767=ORIENTED_EDGE('',*,*,#9713,.F.);
#12768=ORIENTED_EDGE('',*,*,#9786,.T.);
#12769=ORIENTED_EDGE('',*,*,#9787,.T.);
#12770=ORIENTED_EDGE('',*,*,#9788,.F.);
#12771=ORIENTED_EDGE('',*,*,#9742,.F.);
#12772=ORIENTED_EDGE('',*,*,#9777,.T.);
#12773=ORIENTED_EDGE('',*,*,#9789,.T.);
#12774=ORIENTED_EDGE('',*,*,#9790,.F.);
#12775=ORIENTED_EDGE('',*,*,#9743,.F.);
#12776=ORIENTED_EDGE('',*,*,#9790,.T.);
#12777=ORIENTED_EDGE('',*,*,#9791,.T.);
#12778=ORIENTED_EDGE('',*,*,#9792,.F.);
#12779=ORIENTED_EDGE('',*,*,#9744,.F.);
#12780=ORIENTED_EDGE('',*,*,#9792,.T.);
#12781=ORIENTED_EDGE('',*,*,#9793,.T.);
#12782=ORIENTED_EDGE('',*,*,#9778,.F.);
#12783=ORIENTED_EDGE('',*,*,#9714,.F.);
#12784=ORIENTED_EDGE('',*,*,#9788,.T.);
#12785=ORIENTED_EDGE('',*,*,#9794,.T.);
#12786=ORIENTED_EDGE('',*,*,#9795,.T.);
#12787=ORIENTED_EDGE('',*,*,#9725,.F.);
#12788=ORIENTED_EDGE('',*,*,#9796,.T.);
#12789=ORIENTED_EDGE('',*,*,#9797,.T.);
#12790=ORIENTED_EDGE('',*,*,#9745,.F.);
#12791=ORIENTED_EDGE('',*,*,#9724,.F.);
#12792=ORIENTED_EDGE('',*,*,#9798,.T.);
#12793=ORIENTED_EDGE('',*,*,#9799,.T.);
#12794=ORIENTED_EDGE('',*,*,#9796,.F.);
#12795=ORIENTED_EDGE('',*,*,#9723,.F.);
#12796=ORIENTED_EDGE('',*,*,#9800,.T.);
#12797=ORIENTED_EDGE('',*,*,#9801,.T.);
#12798=ORIENTED_EDGE('',*,*,#9798,.F.);
#12799=ORIENTED_EDGE('',*,*,#9722,.F.);
#12800=ORIENTED_EDGE('',*,*,#9802,.T.);
#12801=ORIENTED_EDGE('',*,*,#9803,.T.);
#12802=ORIENTED_EDGE('',*,*,#9800,.F.);
#12803=ORIENTED_EDGE('',*,*,#9721,.F.);
#12804=ORIENTED_EDGE('',*,*,#9804,.T.);
#12805=ORIENTED_EDGE('',*,*,#9805,.T.);
#12806=ORIENTED_EDGE('',*,*,#9802,.F.);
#12807=ORIENTED_EDGE('',*,*,#9720,.F.);
#12808=ORIENTED_EDGE('',*,*,#9806,.T.);
#12809=ORIENTED_EDGE('',*,*,#9807,.T.);
#12810=ORIENTED_EDGE('',*,*,#9804,.F.);
#12811=ORIENTED_EDGE('',*,*,#9719,.F.);
#12812=ORIENTED_EDGE('',*,*,#9808,.T.);
#12813=ORIENTED_EDGE('',*,*,#9809,.T.);
#12814=ORIENTED_EDGE('',*,*,#9806,.F.);
#12815=ORIENTED_EDGE('',*,*,#9718,.F.);
#12816=ORIENTED_EDGE('',*,*,#9810,.T.);
#12817=ORIENTED_EDGE('',*,*,#9811,.T.);
#12818=ORIENTED_EDGE('',*,*,#9808,.F.);
#12819=ORIENTED_EDGE('',*,*,#9717,.F.);
#12820=ORIENTED_EDGE('',*,*,#9812,.T.);
#12821=ORIENTED_EDGE('',*,*,#9813,.T.);
#12822=ORIENTED_EDGE('',*,*,#9810,.F.);
#12823=ORIENTED_EDGE('',*,*,#9716,.F.);
#12824=ORIENTED_EDGE('',*,*,#9814,.T.);
#12825=ORIENTED_EDGE('',*,*,#9815,.T.);
#12826=ORIENTED_EDGE('',*,*,#9812,.F.);
#12827=ORIENTED_EDGE('',*,*,#9715,.F.);
#12828=ORIENTED_EDGE('',*,*,#9795,.F.);
#12829=ORIENTED_EDGE('',*,*,#9816,.T.);
#12830=ORIENTED_EDGE('',*,*,#9814,.F.);
#12831=ORIENTED_EDGE('',*,*,#9816,.F.);
#12832=ORIENTED_EDGE('',*,*,#9794,.F.);
#12833=ORIENTED_EDGE('',*,*,#9787,.F.);
#12834=ORIENTED_EDGE('',*,*,#9785,.F.);
#12835=ORIENTED_EDGE('',*,*,#9783,.F.);
#12836=ORIENTED_EDGE('',*,*,#9781,.F.);
#12837=ORIENTED_EDGE('',*,*,#9779,.F.);
#12838=ORIENTED_EDGE('',*,*,#9793,.F.);
#12839=ORIENTED_EDGE('',*,*,#9791,.F.);
#12840=ORIENTED_EDGE('',*,*,#9789,.F.);
#12841=ORIENTED_EDGE('',*,*,#9776,.F.);
#12842=ORIENTED_EDGE('',*,*,#9774,.F.);
#12843=ORIENTED_EDGE('',*,*,#9772,.F.);
#12844=ORIENTED_EDGE('',*,*,#9770,.F.);
#12845=ORIENTED_EDGE('',*,*,#9768,.F.);
#12846=ORIENTED_EDGE('',*,*,#9766,.F.);
#12847=ORIENTED_EDGE('',*,*,#9764,.F.);
#12848=ORIENTED_EDGE('',*,*,#9762,.F.);
#12849=ORIENTED_EDGE('',*,*,#9760,.F.);
#12850=ORIENTED_EDGE('',*,*,#9758,.F.);
#12851=ORIENTED_EDGE('',*,*,#9756,.F.);
#12852=ORIENTED_EDGE('',*,*,#9754,.F.);
#12853=ORIENTED_EDGE('',*,*,#9752,.F.);
#12854=ORIENTED_EDGE('',*,*,#9750,.F.);
#12855=ORIENTED_EDGE('',*,*,#9748,.F.);
#12856=ORIENTED_EDGE('',*,*,#9746,.F.);
#12857=ORIENTED_EDGE('',*,*,#9797,.F.);
#12858=ORIENTED_EDGE('',*,*,#9799,.F.);
#12859=ORIENTED_EDGE('',*,*,#9801,.F.);
#12860=ORIENTED_EDGE('',*,*,#9803,.F.);
#12861=ORIENTED_EDGE('',*,*,#9805,.F.);
#12862=ORIENTED_EDGE('',*,*,#9807,.F.);
#12863=ORIENTED_EDGE('',*,*,#9809,.F.);
#12864=ORIENTED_EDGE('',*,*,#9811,.F.);
#12865=ORIENTED_EDGE('',*,*,#9813,.F.);
#12866=ORIENTED_EDGE('',*,*,#9815,.F.);
#12867=ORIENTED_EDGE('',*,*,#9817,.T.);
#12868=ORIENTED_EDGE('',*,*,#9818,.F.);
#12869=ORIENTED_EDGE('',*,*,#9819,.F.);
#12870=ORIENTED_EDGE('',*,*,#9820,.T.);
#12871=ORIENTED_EDGE('',*,*,#9821,.T.);
#12872=ORIENTED_EDGE('',*,*,#9822,.F.);
#12873=ORIENTED_EDGE('',*,*,#9823,.F.);
#12874=ORIENTED_EDGE('',*,*,#9818,.T.);
#12875=ORIENTED_EDGE('',*,*,#9824,.T.);
#12876=ORIENTED_EDGE('',*,*,#9825,.F.);
#12877=ORIENTED_EDGE('',*,*,#9826,.F.);
#12878=ORIENTED_EDGE('',*,*,#9822,.T.);
#12879=ORIENTED_EDGE('',*,*,#9827,.T.);
#12880=ORIENTED_EDGE('',*,*,#9828,.F.);
#12881=ORIENTED_EDGE('',*,*,#9829,.F.);
#12882=ORIENTED_EDGE('',*,*,#9825,.T.);
#12883=ORIENTED_EDGE('',*,*,#9830,.T.);
#12884=ORIENTED_EDGE('',*,*,#9831,.F.);
#12885=ORIENTED_EDGE('',*,*,#9832,.F.);
#12886=ORIENTED_EDGE('',*,*,#9828,.T.);
#12887=ORIENTED_EDGE('',*,*,#9833,.T.);
#12888=ORIENTED_EDGE('',*,*,#9834,.F.);
#12889=ORIENTED_EDGE('',*,*,#9835,.F.);
#12890=ORIENTED_EDGE('',*,*,#9831,.T.);
#12891=ORIENTED_EDGE('',*,*,#9836,.T.);
#12892=ORIENTED_EDGE('',*,*,#9837,.F.);
#12893=ORIENTED_EDGE('',*,*,#9838,.F.);
#12894=ORIENTED_EDGE('',*,*,#9834,.T.);
#12895=ORIENTED_EDGE('',*,*,#9839,.F.);
#12896=ORIENTED_EDGE('',*,*,#9840,.F.);
#12897=ORIENTED_EDGE('',*,*,#9841,.F.);
#12898=ORIENTED_EDGE('',*,*,#9842,.F.);
#12899=ORIENTED_EDGE('',*,*,#9843,.F.);
#12900=ORIENTED_EDGE('',*,*,#9844,.F.);
#12901=ORIENTED_EDGE('',*,*,#9845,.F.);
#12902=ORIENTED_EDGE('',*,*,#9846,.F.);
#12903=ORIENTED_EDGE('',*,*,#9847,.F.);
#12904=ORIENTED_EDGE('',*,*,#9848,.F.);
#12905=ORIENTED_EDGE('',*,*,#9836,.F.);
#12906=ORIENTED_EDGE('',*,*,#9833,.F.);
#12907=ORIENTED_EDGE('',*,*,#9830,.F.);
#12908=ORIENTED_EDGE('',*,*,#9827,.F.);
#12909=ORIENTED_EDGE('',*,*,#9824,.F.);
#12910=ORIENTED_EDGE('',*,*,#9821,.F.);
#12911=ORIENTED_EDGE('',*,*,#9817,.F.);
#12912=ORIENTED_EDGE('',*,*,#9849,.F.);
#12913=ORIENTED_EDGE('',*,*,#9850,.F.);
#12914=ORIENTED_EDGE('',*,*,#9851,.F.);
#12915=ORIENTED_EDGE('',*,*,#9852,.F.);
#12916=ORIENTED_EDGE('',*,*,#9853,.F.);
#12917=ORIENTED_EDGE('',*,*,#9854,.F.);
#12918=ORIENTED_EDGE('',*,*,#9855,.F.);
#12919=ORIENTED_EDGE('',*,*,#9856,.F.);
#12920=ORIENTED_EDGE('',*,*,#9857,.F.);
#12921=ORIENTED_EDGE('',*,*,#9858,.F.);
#12922=ORIENTED_EDGE('',*,*,#9859,.F.);
#12923=ORIENTED_EDGE('',*,*,#9860,.F.);
#12924=ORIENTED_EDGE('',*,*,#9861,.F.);
#12925=ORIENTED_EDGE('',*,*,#9862,.F.);
#12926=ORIENTED_EDGE('',*,*,#9863,.F.);
#12927=ORIENTED_EDGE('',*,*,#9864,.F.);
#12928=ORIENTED_EDGE('',*,*,#9865,.F.);
#12929=ORIENTED_EDGE('',*,*,#9866,.T.);
#12930=ORIENTED_EDGE('',*,*,#9867,.T.);
#12931=ORIENTED_EDGE('',*,*,#9868,.T.);
#12932=ORIENTED_EDGE('',*,*,#9869,.T.);
#12933=ORIENTED_EDGE('',*,*,#9870,.T.);
#12934=ORIENTED_EDGE('',*,*,#9871,.F.);
#12935=ORIENTED_EDGE('',*,*,#9872,.F.);
#12936=ORIENTED_EDGE('',*,*,#9873,.F.);
#12937=ORIENTED_EDGE('',*,*,#9874,.F.);
#12938=ORIENTED_EDGE('',*,*,#9875,.F.);
#12939=ORIENTED_EDGE('',*,*,#9876,.F.);
#12940=ORIENTED_EDGE('',*,*,#9877,.T.);
#12941=ORIENTED_EDGE('',*,*,#9878,.T.);
#12942=ORIENTED_EDGE('',*,*,#9839,.T.);
#12943=ORIENTED_EDGE('',*,*,#9879,.F.);
#12944=ORIENTED_EDGE('',*,*,#9880,.T.);
#12945=ORIENTED_EDGE('',*,*,#9876,.T.);
#12946=ORIENTED_EDGE('',*,*,#9875,.T.);
#12947=ORIENTED_EDGE('',*,*,#9881,.F.);
#12948=ORIENTED_EDGE('',*,*,#9882,.T.);
#12949=ORIENTED_EDGE('',*,*,#9879,.T.);
#12950=ORIENTED_EDGE('',*,*,#9874,.T.);
#12951=ORIENTED_EDGE('',*,*,#9883,.F.);
#12952=ORIENTED_EDGE('',*,*,#9884,.T.);
#12953=ORIENTED_EDGE('',*,*,#9881,.T.);
#12954=ORIENTED_EDGE('',*,*,#9873,.T.);
#12955=ORIENTED_EDGE('',*,*,#9885,.F.);
#12956=ORIENTED_EDGE('',*,*,#9886,.F.);
#12957=ORIENTED_EDGE('',*,*,#9887,.F.);
#12958=ORIENTED_EDGE('',*,*,#9888,.T.);
#12959=ORIENTED_EDGE('',*,*,#9883,.T.);
#12960=ORIENTED_EDGE('',*,*,#9872,.T.);
#12961=ORIENTED_EDGE('',*,*,#9871,.T.);
#12962=ORIENTED_EDGE('',*,*,#9889,.F.);
#12963=ORIENTED_EDGE('',*,*,#9890,.F.);
#12964=ORIENTED_EDGE('',*,*,#9887,.T.);
#12965=ORIENTED_EDGE('',*,*,#9877,.F.);
#12966=ORIENTED_EDGE('',*,*,#9880,.F.);
#12967=ORIENTED_EDGE('',*,*,#9882,.F.);
#12968=ORIENTED_EDGE('',*,*,#9884,.F.);
#12969=ORIENTED_EDGE('',*,*,#9888,.F.);
#12970=ORIENTED_EDGE('',*,*,#9890,.T.);
#12971=ORIENTED_EDGE('',*,*,#9891,.T.);
#12972=ORIENTED_EDGE('',*,*,#9892,.T.);
#12973=ORIENTED_EDGE('',*,*,#9893,.T.);
#12974=ORIENTED_EDGE('',*,*,#9894,.T.);
#12975=ORIENTED_EDGE('',*,*,#9895,.T.);
#12976=ORIENTED_EDGE('',*,*,#9896,.T.);
#12977=ORIENTED_EDGE('',*,*,#9897,.T.);
#12978=ORIENTED_EDGE('',*,*,#9898,.T.);
#12979=ORIENTED_EDGE('',*,*,#9899,.T.);
#12980=ORIENTED_EDGE('',*,*,#9900,.T.);
#12981=ORIENTED_EDGE('',*,*,#9901,.T.);
#12982=ORIENTED_EDGE('',*,*,#9902,.T.);
#12983=ORIENTED_EDGE('',*,*,#9903,.T.);
#12984=ORIENTED_EDGE('',*,*,#9904,.T.);
#12985=ORIENTED_EDGE('',*,*,#9905,.T.);
#12986=ORIENTED_EDGE('',*,*,#9906,.T.);
#12987=ORIENTED_EDGE('',*,*,#9907,.T.);
#12988=ORIENTED_EDGE('',*,*,#9908,.T.);
#12989=ORIENTED_EDGE('',*,*,#9909,.T.);
#12990=ORIENTED_EDGE('',*,*,#9910,.T.);
#12991=ORIENTED_EDGE('',*,*,#9911,.T.);
#12992=ORIENTED_EDGE('',*,*,#9912,.T.);
#12993=ORIENTED_EDGE('',*,*,#9819,.T.);
#12994=ORIENTED_EDGE('',*,*,#9823,.T.);
#12995=ORIENTED_EDGE('',*,*,#9826,.T.);
#12996=ORIENTED_EDGE('',*,*,#9829,.T.);
#12997=ORIENTED_EDGE('',*,*,#9832,.T.);
#12998=ORIENTED_EDGE('',*,*,#9835,.T.);
#12999=ORIENTED_EDGE('',*,*,#9838,.T.);
#13000=ORIENTED_EDGE('',*,*,#9913,.T.);
#13001=ORIENTED_EDGE('',*,*,#9914,.T.);
#13002=ORIENTED_EDGE('',*,*,#9915,.T.);
#13003=ORIENTED_EDGE('',*,*,#9916,.T.);
#13004=ORIENTED_EDGE('',*,*,#9917,.T.);
#13005=ORIENTED_EDGE('',*,*,#9918,.T.);
#13006=ORIENTED_EDGE('',*,*,#9919,.T.);
#13007=ORIENTED_EDGE('',*,*,#9920,.T.);
#13008=ORIENTED_EDGE('',*,*,#9921,.T.);
#13009=ORIENTED_EDGE('',*,*,#9922,.T.);
#13010=ORIENTED_EDGE('',*,*,#9866,.F.);
#13011=ORIENTED_EDGE('',*,*,#9923,.T.);
#13012=ORIENTED_EDGE('',*,*,#9895,.F.);
#13013=ORIENTED_EDGE('',*,*,#9924,.T.);
#13014=ORIENTED_EDGE('',*,*,#9867,.F.);
#13015=ORIENTED_EDGE('',*,*,#9922,.F.);
#13016=ORIENTED_EDGE('',*,*,#9894,.F.);
#13017=ORIENTED_EDGE('',*,*,#9925,.T.);
#13018=ORIENTED_EDGE('',*,*,#9868,.F.);
#13019=ORIENTED_EDGE('',*,*,#9924,.F.);
#13020=ORIENTED_EDGE('',*,*,#9893,.F.);
#13021=ORIENTED_EDGE('',*,*,#9926,.T.);
#13022=ORIENTED_EDGE('',*,*,#9869,.F.);
#13023=ORIENTED_EDGE('',*,*,#9925,.F.);
#13024=ORIENTED_EDGE('',*,*,#9892,.F.);
#13025=ORIENTED_EDGE('',*,*,#9927,.F.);
#13026=ORIENTED_EDGE('',*,*,#9928,.F.);
#13027=ORIENTED_EDGE('',*,*,#9889,.T.);
#13028=ORIENTED_EDGE('',*,*,#9870,.F.);
#13029=ORIENTED_EDGE('',*,*,#9926,.F.);
#13030=ORIENTED_EDGE('',*,*,#9891,.F.);
#13031=ORIENTED_EDGE('',*,*,#9886,.T.);
#13032=ORIENTED_EDGE('',*,*,#9929,.T.);
#13033=ORIENTED_EDGE('',*,*,#9930,.T.);
#13034=ORIENTED_EDGE('',*,*,#9929,.F.);
#13035=ORIENTED_EDGE('',*,*,#9928,.T.);
#13036=ORIENTED_EDGE('',*,*,#9931,.T.);
#13037=ORIENTED_EDGE('',*,*,#9932,.T.);
#13038=ORIENTED_EDGE('',*,*,#9931,.F.);
#13039=ORIENTED_EDGE('',*,*,#9885,.T.);
#13040=ORIENTED_EDGE('',*,*,#9933,.T.);
#13041=ORIENTED_EDGE('',*,*,#9934,.T.);
#13042=ORIENTED_EDGE('',*,*,#9933,.F.);
#13043=ORIENTED_EDGE('',*,*,#9927,.T.);
#13044=ORIENTED_EDGE('',*,*,#9935,.T.);
#13045=ORIENTED_EDGE('',*,*,#9936,.T.);
#13046=ORIENTED_EDGE('',*,*,#9935,.F.);
#13047=ORIENTED_EDGE('',*,*,#9840,.T.);
#13048=ORIENTED_EDGE('',*,*,#9878,.F.);
#13049=ORIENTED_EDGE('',*,*,#9921,.F.);
#13050=ORIENTED_EDGE('',*,*,#9937,.T.);
#13051=ORIENTED_EDGE('',*,*,#9841,.T.);
#13052=ORIENTED_EDGE('',*,*,#9937,.F.);
#13053=ORIENTED_EDGE('',*,*,#9920,.F.);
#13054=ORIENTED_EDGE('',*,*,#9938,.T.);
#13055=ORIENTED_EDGE('',*,*,#9842,.T.);
#13056=ORIENTED_EDGE('',*,*,#9938,.F.);
#13057=ORIENTED_EDGE('',*,*,#9919,.F.);
#13058=ORIENTED_EDGE('',*,*,#9939,.T.);
#13059=ORIENTED_EDGE('',*,*,#9930,.F.);
#13060=ORIENTED_EDGE('',*,*,#9934,.F.);
#13061=ORIENTED_EDGE('',*,*,#9843,.T.);
#13062=ORIENTED_EDGE('',*,*,#9939,.F.);
#13063=ORIENTED_EDGE('',*,*,#9918,.F.);
#13064=ORIENTED_EDGE('',*,*,#9940,.T.);
#13065=ORIENTED_EDGE('',*,*,#9844,.T.);
#13066=ORIENTED_EDGE('',*,*,#9940,.F.);
#13067=ORIENTED_EDGE('',*,*,#9917,.F.);
#13068=ORIENTED_EDGE('',*,*,#9941,.T.);
#13069=ORIENTED_EDGE('',*,*,#9845,.T.);
#13070=ORIENTED_EDGE('',*,*,#9941,.F.);
#13071=ORIENTED_EDGE('',*,*,#9916,.F.);
#13072=ORIENTED_EDGE('',*,*,#9942,.T.);
#13073=ORIENTED_EDGE('',*,*,#9846,.T.);
#13074=ORIENTED_EDGE('',*,*,#9942,.F.);
#13075=ORIENTED_EDGE('',*,*,#9915,.F.);
#13076=ORIENTED_EDGE('',*,*,#9943,.T.);
#13077=ORIENTED_EDGE('',*,*,#9847,.T.);
#13078=ORIENTED_EDGE('',*,*,#9943,.F.);
#13079=ORIENTED_EDGE('',*,*,#9914,.F.);
#13080=ORIENTED_EDGE('',*,*,#9944,.T.);
#13081=ORIENTED_EDGE('',*,*,#9848,.T.);
#13082=ORIENTED_EDGE('',*,*,#9944,.F.);
#13083=ORIENTED_EDGE('',*,*,#9913,.F.);
#13084=ORIENTED_EDGE('',*,*,#9837,.T.);
#13085=ORIENTED_EDGE('',*,*,#9865,.T.);
#13086=ORIENTED_EDGE('',*,*,#9945,.F.);
#13087=ORIENTED_EDGE('',*,*,#9896,.F.);
#13088=ORIENTED_EDGE('',*,*,#9923,.F.);
#13089=ORIENTED_EDGE('',*,*,#9864,.T.);
#13090=ORIENTED_EDGE('',*,*,#9946,.F.);
#13091=ORIENTED_EDGE('',*,*,#9897,.F.);
#13092=ORIENTED_EDGE('',*,*,#9945,.T.);
#13093=ORIENTED_EDGE('',*,*,#9863,.T.);
#13094=ORIENTED_EDGE('',*,*,#9947,.F.);
#13095=ORIENTED_EDGE('',*,*,#9898,.F.);
#13096=ORIENTED_EDGE('',*,*,#9946,.T.);
#13097=ORIENTED_EDGE('',*,*,#9936,.F.);
#13098=ORIENTED_EDGE('',*,*,#9932,.F.);
#13099=ORIENTED_EDGE('',*,*,#9862,.T.);
#13100=ORIENTED_EDGE('',*,*,#9948,.F.);
#13101=ORIENTED_EDGE('',*,*,#9899,.F.);
#13102=ORIENTED_EDGE('',*,*,#9947,.T.);
#13103=ORIENTED_EDGE('',*,*,#9861,.T.);
#13104=ORIENTED_EDGE('',*,*,#9949,.F.);
#13105=ORIENTED_EDGE('',*,*,#9900,.F.);
#13106=ORIENTED_EDGE('',*,*,#9948,.T.);
#13107=ORIENTED_EDGE('',*,*,#9860,.T.);
#13108=ORIENTED_EDGE('',*,*,#9950,.T.);
#13109=ORIENTED_EDGE('',*,*,#9901,.F.);
#13110=ORIENTED_EDGE('',*,*,#9949,.T.);
#13111=ORIENTED_EDGE('',*,*,#9859,.T.);
#13112=ORIENTED_EDGE('',*,*,#9951,.F.);
#13113=ORIENTED_EDGE('',*,*,#9902,.F.);
#13114=ORIENTED_EDGE('',*,*,#9950,.F.);
#13115=ORIENTED_EDGE('',*,*,#9858,.T.);
#13116=ORIENTED_EDGE('',*,*,#9952,.F.);
#13117=ORIENTED_EDGE('',*,*,#9903,.F.);
#13118=ORIENTED_EDGE('',*,*,#9951,.T.);
#13119=ORIENTED_EDGE('',*,*,#9857,.T.);
#13120=ORIENTED_EDGE('',*,*,#9953,.F.);
#13121=ORIENTED_EDGE('',*,*,#9904,.F.);
#13122=ORIENTED_EDGE('',*,*,#9952,.T.);
#13123=ORIENTED_EDGE('',*,*,#9856,.T.);
#13124=ORIENTED_EDGE('',*,*,#9954,.F.);
#13125=ORIENTED_EDGE('',*,*,#9905,.F.);
#13126=ORIENTED_EDGE('',*,*,#9953,.T.);
#13127=ORIENTED_EDGE('',*,*,#9855,.T.);
#13128=ORIENTED_EDGE('',*,*,#9955,.F.);
#13129=ORIENTED_EDGE('',*,*,#9906,.F.);
#13130=ORIENTED_EDGE('',*,*,#9954,.T.);
#13131=ORIENTED_EDGE('',*,*,#9854,.T.);
#13132=ORIENTED_EDGE('',*,*,#9956,.F.);
#13133=ORIENTED_EDGE('',*,*,#9907,.F.);
#13134=ORIENTED_EDGE('',*,*,#9955,.T.);
#13135=ORIENTED_EDGE('',*,*,#9853,.T.);
#13136=ORIENTED_EDGE('',*,*,#9957,.F.);
#13137=ORIENTED_EDGE('',*,*,#9908,.F.);
#13138=ORIENTED_EDGE('',*,*,#9956,.T.);
#13139=ORIENTED_EDGE('',*,*,#9852,.T.);
#13140=ORIENTED_EDGE('',*,*,#9958,.F.);
#13141=ORIENTED_EDGE('',*,*,#9909,.F.);
#13142=ORIENTED_EDGE('',*,*,#9957,.T.);
#13143=ORIENTED_EDGE('',*,*,#9851,.T.);
#13144=ORIENTED_EDGE('',*,*,#9959,.F.);
#13145=ORIENTED_EDGE('',*,*,#9910,.F.);
#13146=ORIENTED_EDGE('',*,*,#9958,.T.);
#13147=ORIENTED_EDGE('',*,*,#9850,.T.);
#13148=ORIENTED_EDGE('',*,*,#9960,.F.);
#13149=ORIENTED_EDGE('',*,*,#9911,.F.);
#13150=ORIENTED_EDGE('',*,*,#9959,.T.);
#13151=ORIENTED_EDGE('',*,*,#9849,.T.);
#13152=ORIENTED_EDGE('',*,*,#9820,.F.);
#13153=ORIENTED_EDGE('',*,*,#9912,.F.);
#13154=ORIENTED_EDGE('',*,*,#9960,.T.);
#13155=ORIENTED_EDGE('',*,*,#9961,.T.);
#13156=ORIENTED_EDGE('',*,*,#9962,.F.);
#13157=ORIENTED_EDGE('',*,*,#9963,.T.);
#13158=ORIENTED_EDGE('',*,*,#9964,.T.);
#13159=ORIENTED_EDGE('',*,*,#9965,.T.);
#13160=ORIENTED_EDGE('',*,*,#9966,.F.);
#13161=ORIENTED_EDGE('',*,*,#9967,.T.);
#13162=ORIENTED_EDGE('',*,*,#9962,.T.);
#13163=ORIENTED_EDGE('',*,*,#9968,.T.);
#13164=ORIENTED_EDGE('',*,*,#9969,.F.);
#13165=ORIENTED_EDGE('',*,*,#9970,.T.);
#13166=ORIENTED_EDGE('',*,*,#9966,.T.);
#13167=ORIENTED_EDGE('',*,*,#9971,.T.);
#13168=ORIENTED_EDGE('',*,*,#9972,.F.);
#13169=ORIENTED_EDGE('',*,*,#9973,.T.);
#13170=ORIENTED_EDGE('',*,*,#9969,.T.);
#13171=ORIENTED_EDGE('',*,*,#9974,.T.);
#13172=ORIENTED_EDGE('',*,*,#9975,.F.);
#13173=ORIENTED_EDGE('',*,*,#9976,.T.);
#13174=ORIENTED_EDGE('',*,*,#9972,.T.);
#13175=ORIENTED_EDGE('',*,*,#9977,.T.);
#13176=ORIENTED_EDGE('',*,*,#9978,.F.);
#13177=ORIENTED_EDGE('',*,*,#9979,.T.);
#13178=ORIENTED_EDGE('',*,*,#9975,.T.);
#13179=ORIENTED_EDGE('',*,*,#9980,.T.);
#13180=ORIENTED_EDGE('',*,*,#9981,.F.);
#13181=ORIENTED_EDGE('',*,*,#9982,.T.);
#13182=ORIENTED_EDGE('',*,*,#9978,.T.);
#13183=ORIENTED_EDGE('',*,*,#9983,.T.);
#13184=ORIENTED_EDGE('',*,*,#9984,.F.);
#13185=ORIENTED_EDGE('',*,*,#9985,.T.);
#13186=ORIENTED_EDGE('',*,*,#9981,.T.);
#13187=ORIENTED_EDGE('',*,*,#9986,.F.);
#13188=ORIENTED_EDGE('',*,*,#9987,.F.);
#13189=ORIENTED_EDGE('',*,*,#9988,.T.);
#13190=ORIENTED_EDGE('',*,*,#9989,.T.);
#13191=ORIENTED_EDGE('',*,*,#9990,.F.);
#13192=ORIENTED_EDGE('',*,*,#9991,.F.);
#13193=ORIENTED_EDGE('',*,*,#9992,.T.);
#13194=ORIENTED_EDGE('',*,*,#9987,.T.);
#13195=ORIENTED_EDGE('',*,*,#9993,.F.);
#13196=ORIENTED_EDGE('',*,*,#9994,.F.);
#13197=ORIENTED_EDGE('',*,*,#9995,.T.);
#13198=ORIENTED_EDGE('',*,*,#9991,.T.);
#13199=ORIENTED_EDGE('',*,*,#9996,.T.);
#13200=ORIENTED_EDGE('',*,*,#9997,.F.);
#13201=ORIENTED_EDGE('',*,*,#9998,.T.);
#13202=ORIENTED_EDGE('',*,*,#9994,.T.);
#13203=ORIENTED_EDGE('',*,*,#9999,.T.);
#13204=ORIENTED_EDGE('',*,*,#10000,.F.);
#13205=ORIENTED_EDGE('',*,*,#10001,.T.);
#13206=ORIENTED_EDGE('',*,*,#9997,.T.);
#13207=ORIENTED_EDGE('',*,*,#10002,.T.);
#13208=ORIENTED_EDGE('',*,*,#10003,.F.);
#13209=ORIENTED_EDGE('',*,*,#10004,.T.);
#13210=ORIENTED_EDGE('',*,*,#10000,.T.);
#13211=ORIENTED_EDGE('',*,*,#10005,.T.);
#13212=ORIENTED_EDGE('',*,*,#10006,.F.);
#13213=ORIENTED_EDGE('',*,*,#10007,.T.);
#13214=ORIENTED_EDGE('',*,*,#10003,.T.);
#13215=ORIENTED_EDGE('',*,*,#10008,.T.);
#13216=ORIENTED_EDGE('',*,*,#10009,.F.);
#13217=ORIENTED_EDGE('',*,*,#10010,.T.);
#13218=ORIENTED_EDGE('',*,*,#10006,.T.);
#13219=ORIENTED_EDGE('',*,*,#10011,.F.);
#13220=ORIENTED_EDGE('',*,*,#10012,.F.);
#13221=ORIENTED_EDGE('',*,*,#10013,.F.);
#13222=ORIENTED_EDGE('',*,*,#10014,.F.);
#13223=ORIENTED_EDGE('',*,*,#10015,.F.);
#13224=ORIENTED_EDGE('',*,*,#10016,.F.);
#13225=ORIENTED_EDGE('',*,*,#10017,.F.);
#13226=ORIENTED_EDGE('',*,*,#10018,.F.);
#13227=ORIENTED_EDGE('',*,*,#10019,.F.);
#13228=ORIENTED_EDGE('',*,*,#10020,.F.);
#13229=ORIENTED_EDGE('',*,*,#10021,.F.);
#13230=ORIENTED_EDGE('',*,*,#10022,.F.);
#13231=ORIENTED_EDGE('',*,*,#10023,.F.);
#13232=ORIENTED_EDGE('',*,*,#10024,.F.);
#13233=ORIENTED_EDGE('',*,*,#10025,.F.);
#13234=ORIENTED_EDGE('',*,*,#10026,.F.);
#13235=ORIENTED_EDGE('',*,*,#10027,.F.);
#13236=ORIENTED_EDGE('',*,*,#10028,.F.);
#13237=ORIENTED_EDGE('',*,*,#9963,.F.);
#13238=ORIENTED_EDGE('',*,*,#9967,.F.);
#13239=ORIENTED_EDGE('',*,*,#9970,.F.);
#13240=ORIENTED_EDGE('',*,*,#9973,.F.);
#13241=ORIENTED_EDGE('',*,*,#9976,.F.);
#13242=ORIENTED_EDGE('',*,*,#9979,.F.);
#13243=ORIENTED_EDGE('',*,*,#9982,.F.);
#13244=ORIENTED_EDGE('',*,*,#9985,.F.);
#13245=ORIENTED_EDGE('',*,*,#10029,.F.);
#13246=ORIENTED_EDGE('',*,*,#9988,.F.);
#13247=ORIENTED_EDGE('',*,*,#9992,.F.);
#13248=ORIENTED_EDGE('',*,*,#9995,.F.);
#13249=ORIENTED_EDGE('',*,*,#9998,.F.);
#13250=ORIENTED_EDGE('',*,*,#10001,.F.);
#13251=ORIENTED_EDGE('',*,*,#10004,.F.);
#13252=ORIENTED_EDGE('',*,*,#10007,.F.);
#13253=ORIENTED_EDGE('',*,*,#10010,.F.);
#13254=ORIENTED_EDGE('',*,*,#10030,.F.);
#13255=ORIENTED_EDGE('',*,*,#10031,.T.);
#13256=ORIENTED_EDGE('',*,*,#9989,.F.);
#13257=ORIENTED_EDGE('',*,*,#10029,.T.);
#13258=ORIENTED_EDGE('',*,*,#9984,.T.);
#13259=ORIENTED_EDGE('',*,*,#10032,.T.);
#13260=ORIENTED_EDGE('',*,*,#10033,.T.);
#13261=ORIENTED_EDGE('',*,*,#10030,.T.);
#13262=ORIENTED_EDGE('',*,*,#10009,.T.);
#13263=ORIENTED_EDGE('',*,*,#10034,.T.);
#13264=ORIENTED_EDGE('',*,*,#10035,.F.);
#13265=ORIENTED_EDGE('',*,*,#10011,.T.);
#13266=ORIENTED_EDGE('',*,*,#10033,.F.);
#13267=ORIENTED_EDGE('',*,*,#10036,.T.);
#13268=ORIENTED_EDGE('',*,*,#10037,.F.);
#13269=ORIENTED_EDGE('',*,*,#10012,.T.);
#13270=ORIENTED_EDGE('',*,*,#10035,.T.);
#13271=ORIENTED_EDGE('',*,*,#10038,.T.);
#13272=ORIENTED_EDGE('',*,*,#10039,.F.);
#13273=ORIENTED_EDGE('',*,*,#10013,.T.);
#13274=ORIENTED_EDGE('',*,*,#10037,.T.);
#13275=ORIENTED_EDGE('',*,*,#10040,.T.);
#13276=ORIENTED_EDGE('',*,*,#10041,.F.);
#13277=ORIENTED_EDGE('',*,*,#10014,.T.);
#13278=ORIENTED_EDGE('',*,*,#10039,.T.);
#13279=ORIENTED_EDGE('',*,*,#10042,.T.);
#13280=ORIENTED_EDGE('',*,*,#10043,.F.);
#13281=ORIENTED_EDGE('',*,*,#10015,.T.);
#13282=ORIENTED_EDGE('',*,*,#10041,.T.);
#13283=ORIENTED_EDGE('',*,*,#10044,.T.);
#13284=ORIENTED_EDGE('',*,*,#10045,.F.);
#13285=ORIENTED_EDGE('',*,*,#10016,.T.);
#13286=ORIENTED_EDGE('',*,*,#10043,.T.);
#13287=ORIENTED_EDGE('',*,*,#10046,.T.);
#13288=ORIENTED_EDGE('',*,*,#10047,.F.);
#13289=ORIENTED_EDGE('',*,*,#10017,.T.);
#13290=ORIENTED_EDGE('',*,*,#10045,.T.);
#13291=ORIENTED_EDGE('',*,*,#10048,.T.);
#13292=ORIENTED_EDGE('',*,*,#10049,.F.);
#13293=ORIENTED_EDGE('',*,*,#10018,.T.);
#13294=ORIENTED_EDGE('',*,*,#10047,.T.);
#13295=ORIENTED_EDGE('',*,*,#10050,.T.);
#13296=ORIENTED_EDGE('',*,*,#10051,.F.);
#13297=ORIENTED_EDGE('',*,*,#10019,.T.);
#13298=ORIENTED_EDGE('',*,*,#10049,.T.);
#13299=ORIENTED_EDGE('',*,*,#10052,.T.);
#13300=ORIENTED_EDGE('',*,*,#10053,.F.);
#13301=ORIENTED_EDGE('',*,*,#10020,.T.);
#13302=ORIENTED_EDGE('',*,*,#10051,.T.);
#13303=ORIENTED_EDGE('',*,*,#10054,.T.);
#13304=ORIENTED_EDGE('',*,*,#10055,.F.);
#13305=ORIENTED_EDGE('',*,*,#10021,.T.);
#13306=ORIENTED_EDGE('',*,*,#10053,.T.);
#13307=ORIENTED_EDGE('',*,*,#10056,.T.);
#13308=ORIENTED_EDGE('',*,*,#10057,.F.);
#13309=ORIENTED_EDGE('',*,*,#10022,.T.);
#13310=ORIENTED_EDGE('',*,*,#10055,.T.);
#13311=ORIENTED_EDGE('',*,*,#10058,.T.);
#13312=ORIENTED_EDGE('',*,*,#10059,.F.);
#13313=ORIENTED_EDGE('',*,*,#10023,.T.);
#13314=ORIENTED_EDGE('',*,*,#10057,.T.);
#13315=ORIENTED_EDGE('',*,*,#10060,.T.);
#13316=ORIENTED_EDGE('',*,*,#10061,.F.);
#13317=ORIENTED_EDGE('',*,*,#10024,.T.);
#13318=ORIENTED_EDGE('',*,*,#10059,.T.);
#13319=ORIENTED_EDGE('',*,*,#10062,.T.);
#13320=ORIENTED_EDGE('',*,*,#10063,.F.);
#13321=ORIENTED_EDGE('',*,*,#10025,.T.);
#13322=ORIENTED_EDGE('',*,*,#10061,.T.);
#13323=ORIENTED_EDGE('',*,*,#10064,.T.);
#13324=ORIENTED_EDGE('',*,*,#10065,.F.);
#13325=ORIENTED_EDGE('',*,*,#10026,.T.);
#13326=ORIENTED_EDGE('',*,*,#10063,.T.);
#13327=ORIENTED_EDGE('',*,*,#10066,.T.);
#13328=ORIENTED_EDGE('',*,*,#10067,.F.);
#13329=ORIENTED_EDGE('',*,*,#10027,.T.);
#13330=ORIENTED_EDGE('',*,*,#10065,.T.);
#13331=ORIENTED_EDGE('',*,*,#10068,.T.);
#13332=ORIENTED_EDGE('',*,*,#9964,.F.);
#13333=ORIENTED_EDGE('',*,*,#10028,.T.);
#13334=ORIENTED_EDGE('',*,*,#10067,.T.);
#13335=ORIENTED_EDGE('',*,*,#10032,.F.);
#13336=ORIENTED_EDGE('',*,*,#10008,.F.);
#13337=ORIENTED_EDGE('',*,*,#10005,.F.);
#13338=ORIENTED_EDGE('',*,*,#10002,.F.);
#13339=ORIENTED_EDGE('',*,*,#9999,.F.);
#13340=ORIENTED_EDGE('',*,*,#9996,.F.);
#13341=ORIENTED_EDGE('',*,*,#9993,.T.);
#13342=ORIENTED_EDGE('',*,*,#9990,.T.);
#13343=ORIENTED_EDGE('',*,*,#9986,.T.);
#13344=ORIENTED_EDGE('',*,*,#10031,.F.);
#13345=ORIENTED_EDGE('',*,*,#9983,.F.);
#13346=ORIENTED_EDGE('',*,*,#9980,.F.);
#13347=ORIENTED_EDGE('',*,*,#9977,.F.);
#13348=ORIENTED_EDGE('',*,*,#9974,.F.);
#13349=ORIENTED_EDGE('',*,*,#9971,.F.);
#13350=ORIENTED_EDGE('',*,*,#9968,.F.);
#13351=ORIENTED_EDGE('',*,*,#9965,.F.);
#13352=ORIENTED_EDGE('',*,*,#9961,.F.);
#13353=ORIENTED_EDGE('',*,*,#10068,.F.);
#13354=ORIENTED_EDGE('',*,*,#10066,.F.);
#13355=ORIENTED_EDGE('',*,*,#10064,.F.);
#13356=ORIENTED_EDGE('',*,*,#10062,.F.);
#13357=ORIENTED_EDGE('',*,*,#10060,.F.);
#13358=ORIENTED_EDGE('',*,*,#10058,.F.);
#13359=ORIENTED_EDGE('',*,*,#10056,.F.);
#13360=ORIENTED_EDGE('',*,*,#10054,.F.);
#13361=ORIENTED_EDGE('',*,*,#10052,.F.);
#13362=ORIENTED_EDGE('',*,*,#10050,.F.);
#13363=ORIENTED_EDGE('',*,*,#10048,.F.);
#13364=ORIENTED_EDGE('',*,*,#10046,.F.);
#13365=ORIENTED_EDGE('',*,*,#10044,.F.);
#13366=ORIENTED_EDGE('',*,*,#10042,.F.);
#13367=ORIENTED_EDGE('',*,*,#10040,.F.);
#13368=ORIENTED_EDGE('',*,*,#10038,.F.);
#13369=ORIENTED_EDGE('',*,*,#10036,.F.);
#13370=ORIENTED_EDGE('',*,*,#10034,.F.);
#13371=ORIENTED_EDGE('',*,*,#10069,.F.);
#13372=ORIENTED_EDGE('',*,*,#10070,.F.);
#13373=ORIENTED_EDGE('',*,*,#10071,.F.);
#13374=ORIENTED_EDGE('',*,*,#10072,.F.);
#13375=ORIENTED_EDGE('',*,*,#10073,.F.);
#13376=ORIENTED_EDGE('',*,*,#10074,.F.);
#13377=ORIENTED_EDGE('',*,*,#10075,.F.);
#13378=ORIENTED_EDGE('',*,*,#10076,.F.);
#13379=ORIENTED_EDGE('',*,*,#10077,.F.);
#13380=ORIENTED_EDGE('',*,*,#10078,.F.);
#13381=ORIENTED_EDGE('',*,*,#10079,.F.);
#13382=ORIENTED_EDGE('',*,*,#10080,.F.);
#13383=ORIENTED_EDGE('',*,*,#10081,.F.);
#13384=ORIENTED_EDGE('',*,*,#10082,.F.);
#13385=ORIENTED_EDGE('',*,*,#10083,.F.);
#13386=ORIENTED_EDGE('',*,*,#10084,.F.);
#13387=ORIENTED_EDGE('',*,*,#10085,.F.);
#13388=ORIENTED_EDGE('',*,*,#10086,.F.);
#13389=ORIENTED_EDGE('',*,*,#10087,.F.);
#13390=ORIENTED_EDGE('',*,*,#10088,.F.);
#13391=ORIENTED_EDGE('',*,*,#10089,.F.);
#13392=ORIENTED_EDGE('',*,*,#10090,.F.);
#13393=ORIENTED_EDGE('',*,*,#10091,.F.);
#13394=ORIENTED_EDGE('',*,*,#10092,.F.);
#13395=ORIENTED_EDGE('',*,*,#10093,.F.);
#13396=ORIENTED_EDGE('',*,*,#10094,.F.);
#13397=ORIENTED_EDGE('',*,*,#10095,.F.);
#13398=ORIENTED_EDGE('',*,*,#10096,.F.);
#13399=ORIENTED_EDGE('',*,*,#10097,.F.);
#13400=ORIENTED_EDGE('',*,*,#10098,.F.);
#13401=ORIENTED_EDGE('',*,*,#10099,.F.);
#13402=ORIENTED_EDGE('',*,*,#10100,.F.);
#13403=ORIENTED_EDGE('',*,*,#10101,.F.);
#13404=ORIENTED_EDGE('',*,*,#10102,.F.);
#13405=ORIENTED_EDGE('',*,*,#10103,.F.);
#13406=ORIENTED_EDGE('',*,*,#10104,.F.);
#13407=ORIENTED_EDGE('',*,*,#10088,.T.);
#13408=ORIENTED_EDGE('',*,*,#10105,.T.);
#13409=ORIENTED_EDGE('',*,*,#10106,.F.);
#13410=ORIENTED_EDGE('',*,*,#10107,.F.);
#13411=ORIENTED_EDGE('',*,*,#10087,.T.);
#13412=ORIENTED_EDGE('',*,*,#10108,.T.);
#13413=ORIENTED_EDGE('',*,*,#10109,.F.);
#13414=ORIENTED_EDGE('',*,*,#10105,.F.);
#13415=ORIENTED_EDGE('',*,*,#10086,.T.);
#13416=ORIENTED_EDGE('',*,*,#10110,.T.);
#13417=ORIENTED_EDGE('',*,*,#10111,.F.);
#13418=ORIENTED_EDGE('',*,*,#10108,.F.);
#13419=ORIENTED_EDGE('',*,*,#10085,.T.);
#13420=ORIENTED_EDGE('',*,*,#10112,.T.);
#13421=ORIENTED_EDGE('',*,*,#10113,.F.);
#13422=ORIENTED_EDGE('',*,*,#10110,.F.);
#13423=ORIENTED_EDGE('',*,*,#10084,.T.);
#13424=ORIENTED_EDGE('',*,*,#10114,.T.);
#13425=ORIENTED_EDGE('',*,*,#10115,.F.);
#13426=ORIENTED_EDGE('',*,*,#10112,.F.);
#13427=ORIENTED_EDGE('',*,*,#10083,.T.);
#13428=ORIENTED_EDGE('',*,*,#10116,.T.);
#13429=ORIENTED_EDGE('',*,*,#10117,.F.);
#13430=ORIENTED_EDGE('',*,*,#10114,.F.);
#13431=ORIENTED_EDGE('',*,*,#10082,.T.);
#13432=ORIENTED_EDGE('',*,*,#10118,.T.);
#13433=ORIENTED_EDGE('',*,*,#10119,.F.);
#13434=ORIENTED_EDGE('',*,*,#10116,.F.);
#13435=ORIENTED_EDGE('',*,*,#10081,.T.);
#13436=ORIENTED_EDGE('',*,*,#10120,.T.);
#13437=ORIENTED_EDGE('',*,*,#10121,.F.);
#13438=ORIENTED_EDGE('',*,*,#10118,.F.);
#13439=ORIENTED_EDGE('',*,*,#10080,.T.);
#13440=ORIENTED_EDGE('',*,*,#10122,.T.);
#13441=ORIENTED_EDGE('',*,*,#10123,.F.);
#13442=ORIENTED_EDGE('',*,*,#10120,.F.);
#13443=ORIENTED_EDGE('',*,*,#10079,.T.);
#13444=ORIENTED_EDGE('',*,*,#10124,.T.);
#13445=ORIENTED_EDGE('',*,*,#10125,.F.);
#13446=ORIENTED_EDGE('',*,*,#10122,.F.);
#13447=ORIENTED_EDGE('',*,*,#10078,.T.);
#13448=ORIENTED_EDGE('',*,*,#10126,.T.);
#13449=ORIENTED_EDGE('',*,*,#10127,.F.);
#13450=ORIENTED_EDGE('',*,*,#10124,.F.);
#13451=ORIENTED_EDGE('',*,*,#10077,.T.);
#13452=ORIENTED_EDGE('',*,*,#10128,.T.);
#13453=ORIENTED_EDGE('',*,*,#10129,.F.);
#13454=ORIENTED_EDGE('',*,*,#10126,.F.);
#13455=ORIENTED_EDGE('',*,*,#10076,.T.);
#13456=ORIENTED_EDGE('',*,*,#10130,.T.);
#13457=ORIENTED_EDGE('',*,*,#10131,.F.);
#13458=ORIENTED_EDGE('',*,*,#10128,.F.);
#13459=ORIENTED_EDGE('',*,*,#10075,.T.);
#13460=ORIENTED_EDGE('',*,*,#10132,.T.);
#13461=ORIENTED_EDGE('',*,*,#10133,.F.);
#13462=ORIENTED_EDGE('',*,*,#10130,.F.);
#13463=ORIENTED_EDGE('',*,*,#10074,.T.);
#13464=ORIENTED_EDGE('',*,*,#10134,.T.);
#13465=ORIENTED_EDGE('',*,*,#10135,.F.);
#13466=ORIENTED_EDGE('',*,*,#10132,.F.);
#13467=ORIENTED_EDGE('',*,*,#10073,.T.);
#13468=ORIENTED_EDGE('',*,*,#10136,.T.);
#13469=ORIENTED_EDGE('',*,*,#10137,.F.);
#13470=ORIENTED_EDGE('',*,*,#10134,.F.);
#13471=ORIENTED_EDGE('',*,*,#10069,.T.);
#13472=ORIENTED_EDGE('',*,*,#10138,.T.);
#13473=ORIENTED_EDGE('',*,*,#10139,.F.);
#13474=ORIENTED_EDGE('',*,*,#10140,.F.);
#13475=ORIENTED_EDGE('',*,*,#10104,.T.);
#13476=ORIENTED_EDGE('',*,*,#10141,.T.);
#13477=ORIENTED_EDGE('',*,*,#10142,.F.);
#13478=ORIENTED_EDGE('',*,*,#10138,.F.);
#13479=ORIENTED_EDGE('',*,*,#10103,.T.);
#13480=ORIENTED_EDGE('',*,*,#10143,.T.);
#13481=ORIENTED_EDGE('',*,*,#10144,.F.);
#13482=ORIENTED_EDGE('',*,*,#10141,.F.);
#13483=ORIENTED_EDGE('',*,*,#10102,.T.);
#13484=ORIENTED_EDGE('',*,*,#10145,.T.);
#13485=ORIENTED_EDGE('',*,*,#10146,.F.);
#13486=ORIENTED_EDGE('',*,*,#10143,.F.);
#13487=ORIENTED_EDGE('',*,*,#10101,.T.);
#13488=ORIENTED_EDGE('',*,*,#10147,.T.);
#13489=ORIENTED_EDGE('',*,*,#10148,.F.);
#13490=ORIENTED_EDGE('',*,*,#10145,.F.);
#13491=ORIENTED_EDGE('',*,*,#10072,.T.);
#13492=ORIENTED_EDGE('',*,*,#10149,.T.);
#13493=ORIENTED_EDGE('',*,*,#10150,.F.);
#13494=ORIENTED_EDGE('',*,*,#10136,.F.);
#13495=ORIENTED_EDGE('',*,*,#10071,.T.);
#13496=ORIENTED_EDGE('',*,*,#10151,.T.);
#13497=ORIENTED_EDGE('',*,*,#10152,.F.);
#13498=ORIENTED_EDGE('',*,*,#10149,.F.);
#13499=ORIENTED_EDGE('',*,*,#10070,.T.);
#13500=ORIENTED_EDGE('',*,*,#10140,.T.);
#13501=ORIENTED_EDGE('',*,*,#10153,.F.);
#13502=ORIENTED_EDGE('',*,*,#10151,.F.);
#13503=ORIENTED_EDGE('',*,*,#10100,.T.);
#13504=ORIENTED_EDGE('',*,*,#10154,.F.);
#13505=ORIENTED_EDGE('',*,*,#10155,.F.);
#13506=ORIENTED_EDGE('',*,*,#10147,.F.);
#13507=ORIENTED_EDGE('',*,*,#10089,.T.);
#13508=ORIENTED_EDGE('',*,*,#10107,.T.);
#13509=ORIENTED_EDGE('',*,*,#10156,.F.);
#13510=ORIENTED_EDGE('',*,*,#10157,.F.);
#13511=ORIENTED_EDGE('',*,*,#10090,.T.);
#13512=ORIENTED_EDGE('',*,*,#10157,.T.);
#13513=ORIENTED_EDGE('',*,*,#10158,.F.);
#13514=ORIENTED_EDGE('',*,*,#10159,.F.);
#13515=ORIENTED_EDGE('',*,*,#10091,.T.);
#13516=ORIENTED_EDGE('',*,*,#10159,.T.);
#13517=ORIENTED_EDGE('',*,*,#10160,.F.);
#13518=ORIENTED_EDGE('',*,*,#10161,.F.);
#13519=ORIENTED_EDGE('',*,*,#10092,.T.);
#13520=ORIENTED_EDGE('',*,*,#10161,.T.);
#13521=ORIENTED_EDGE('',*,*,#10162,.F.);
#13522=ORIENTED_EDGE('',*,*,#10163,.F.);
#13523=ORIENTED_EDGE('',*,*,#10093,.T.);
#13524=ORIENTED_EDGE('',*,*,#10163,.T.);
#13525=ORIENTED_EDGE('',*,*,#10164,.F.);
#13526=ORIENTED_EDGE('',*,*,#10165,.F.);
#13527=ORIENTED_EDGE('',*,*,#10094,.T.);
#13528=ORIENTED_EDGE('',*,*,#10165,.T.);
#13529=ORIENTED_EDGE('',*,*,#10166,.F.);
#13530=ORIENTED_EDGE('',*,*,#10167,.F.);
#13531=ORIENTED_EDGE('',*,*,#10095,.T.);
#13532=ORIENTED_EDGE('',*,*,#10167,.T.);
#13533=ORIENTED_EDGE('',*,*,#10168,.F.);
#13534=ORIENTED_EDGE('',*,*,#10169,.F.);
#13535=ORIENTED_EDGE('',*,*,#10096,.T.);
#13536=ORIENTED_EDGE('',*,*,#10169,.T.);
#13537=ORIENTED_EDGE('',*,*,#10170,.F.);
#13538=ORIENTED_EDGE('',*,*,#10171,.F.);
#13539=ORIENTED_EDGE('',*,*,#10097,.T.);
#13540=ORIENTED_EDGE('',*,*,#10171,.T.);
#13541=ORIENTED_EDGE('',*,*,#10172,.F.);
#13542=ORIENTED_EDGE('',*,*,#10173,.F.);
#13543=ORIENTED_EDGE('',*,*,#10098,.T.);
#13544=ORIENTED_EDGE('',*,*,#10173,.T.);
#13545=ORIENTED_EDGE('',*,*,#10174,.F.);
#13546=ORIENTED_EDGE('',*,*,#10175,.F.);
#13547=ORIENTED_EDGE('',*,*,#10099,.T.);
#13548=ORIENTED_EDGE('',*,*,#10175,.T.);
#13549=ORIENTED_EDGE('',*,*,#10176,.F.);
#13550=ORIENTED_EDGE('',*,*,#10154,.T.);
#13551=ORIENTED_EDGE('',*,*,#10176,.T.);
#13552=ORIENTED_EDGE('',*,*,#10174,.T.);
#13553=ORIENTED_EDGE('',*,*,#10172,.T.);
#13554=ORIENTED_EDGE('',*,*,#10170,.T.);
#13555=ORIENTED_EDGE('',*,*,#10168,.T.);
#13556=ORIENTED_EDGE('',*,*,#10166,.T.);
#13557=ORIENTED_EDGE('',*,*,#10164,.T.);
#13558=ORIENTED_EDGE('',*,*,#10162,.T.);
#13559=ORIENTED_EDGE('',*,*,#10160,.T.);
#13560=ORIENTED_EDGE('',*,*,#10158,.T.);
#13561=ORIENTED_EDGE('',*,*,#10156,.T.);
#13562=ORIENTED_EDGE('',*,*,#10106,.T.);
#13563=ORIENTED_EDGE('',*,*,#10109,.T.);
#13564=ORIENTED_EDGE('',*,*,#10111,.T.);
#13565=ORIENTED_EDGE('',*,*,#10113,.T.);
#13566=ORIENTED_EDGE('',*,*,#10115,.T.);
#13567=ORIENTED_EDGE('',*,*,#10117,.T.);
#13568=ORIENTED_EDGE('',*,*,#10119,.T.);
#13569=ORIENTED_EDGE('',*,*,#10121,.T.);
#13570=ORIENTED_EDGE('',*,*,#10123,.T.);
#13571=ORIENTED_EDGE('',*,*,#10125,.T.);
#13572=ORIENTED_EDGE('',*,*,#10127,.T.);
#13573=ORIENTED_EDGE('',*,*,#10129,.T.);
#13574=ORIENTED_EDGE('',*,*,#10131,.T.);
#13575=ORIENTED_EDGE('',*,*,#10133,.T.);
#13576=ORIENTED_EDGE('',*,*,#10135,.T.);
#13577=ORIENTED_EDGE('',*,*,#10137,.T.);
#13578=ORIENTED_EDGE('',*,*,#10150,.T.);
#13579=ORIENTED_EDGE('',*,*,#10152,.T.);
#13580=ORIENTED_EDGE('',*,*,#10153,.T.);
#13581=ORIENTED_EDGE('',*,*,#10139,.T.);
#13582=ORIENTED_EDGE('',*,*,#10142,.T.);
#13583=ORIENTED_EDGE('',*,*,#10144,.T.);
#13584=ORIENTED_EDGE('',*,*,#10146,.T.);
#13585=ORIENTED_EDGE('',*,*,#10148,.T.);
#13586=ORIENTED_EDGE('',*,*,#10155,.T.);
#13587=ORIENTED_EDGE('',*,*,#10177,.F.);
#13588=ORIENTED_EDGE('',*,*,#10178,.F.);
#13589=ORIENTED_EDGE('',*,*,#10179,.T.);
#13590=ORIENTED_EDGE('',*,*,#10180,.T.);
#13591=ORIENTED_EDGE('',*,*,#10181,.F.);
#13592=ORIENTED_EDGE('',*,*,#10180,.F.);
#13593=ORIENTED_EDGE('',*,*,#10182,.T.);
#13594=ORIENTED_EDGE('',*,*,#10183,.T.);
#13595=ORIENTED_EDGE('',*,*,#10184,.F.);
#13596=ORIENTED_EDGE('',*,*,#10183,.F.);
#13597=ORIENTED_EDGE('',*,*,#10185,.T.);
#13598=ORIENTED_EDGE('',*,*,#10186,.T.);
#13599=ORIENTED_EDGE('',*,*,#10187,.F.);
#13600=ORIENTED_EDGE('',*,*,#10186,.F.);
#13601=ORIENTED_EDGE('',*,*,#10188,.T.);
#13602=ORIENTED_EDGE('',*,*,#10189,.T.);
#13603=ORIENTED_EDGE('',*,*,#10190,.F.);
#13604=ORIENTED_EDGE('',*,*,#10189,.F.);
#13605=ORIENTED_EDGE('',*,*,#10191,.T.);
#13606=ORIENTED_EDGE('',*,*,#10192,.T.);
#13607=ORIENTED_EDGE('',*,*,#10193,.F.);
#13608=ORIENTED_EDGE('',*,*,#10192,.F.);
#13609=ORIENTED_EDGE('',*,*,#10194,.T.);
#13610=ORIENTED_EDGE('',*,*,#10195,.T.);
#13611=ORIENTED_EDGE('',*,*,#10196,.F.);
#13612=ORIENTED_EDGE('',*,*,#10195,.F.);
#13613=ORIENTED_EDGE('',*,*,#10197,.T.);
#13614=ORIENTED_EDGE('',*,*,#10198,.T.);
#13615=ORIENTED_EDGE('',*,*,#10199,.T.);
#13616=ORIENTED_EDGE('',*,*,#10200,.T.);
#13617=ORIENTED_EDGE('',*,*,#10201,.T.);
#13618=ORIENTED_EDGE('',*,*,#10202,.T.);
#13619=ORIENTED_EDGE('',*,*,#10203,.T.);
#13620=ORIENTED_EDGE('',*,*,#10204,.T.);
#13621=ORIENTED_EDGE('',*,*,#10205,.F.);
#13622=ORIENTED_EDGE('',*,*,#10206,.F.);
#13623=ORIENTED_EDGE('',*,*,#10207,.F.);
#13624=ORIENTED_EDGE('',*,*,#10208,.F.);
#13625=ORIENTED_EDGE('',*,*,#10209,.F.);
#13626=ORIENTED_EDGE('',*,*,#10210,.T.);
#13627=ORIENTED_EDGE('',*,*,#10211,.T.);
#13628=ORIENTED_EDGE('',*,*,#10212,.T.);
#13629=ORIENTED_EDGE('',*,*,#10213,.T.);
#13630=ORIENTED_EDGE('',*,*,#10214,.T.);
#13631=ORIENTED_EDGE('',*,*,#10215,.T.);
#13632=ORIENTED_EDGE('',*,*,#10216,.T.);
#13633=ORIENTED_EDGE('',*,*,#10217,.T.);
#13634=ORIENTED_EDGE('',*,*,#10218,.T.);
#13635=ORIENTED_EDGE('',*,*,#10219,.T.);
#13636=ORIENTED_EDGE('',*,*,#10220,.T.);
#13637=ORIENTED_EDGE('',*,*,#10221,.T.);
#13638=ORIENTED_EDGE('',*,*,#10222,.T.);
#13639=ORIENTED_EDGE('',*,*,#10223,.T.);
#13640=ORIENTED_EDGE('',*,*,#10224,.T.);
#13641=ORIENTED_EDGE('',*,*,#10225,.T.);
#13642=ORIENTED_EDGE('',*,*,#10226,.T.);
#13643=ORIENTED_EDGE('',*,*,#10177,.T.);
#13644=ORIENTED_EDGE('',*,*,#10181,.T.);
#13645=ORIENTED_EDGE('',*,*,#10184,.T.);
#13646=ORIENTED_EDGE('',*,*,#10187,.T.);
#13647=ORIENTED_EDGE('',*,*,#10190,.T.);
#13648=ORIENTED_EDGE('',*,*,#10193,.T.);
#13649=ORIENTED_EDGE('',*,*,#10196,.T.);
#13650=ORIENTED_EDGE('',*,*,#10227,.T.);
#13651=ORIENTED_EDGE('',*,*,#10228,.T.);
#13652=ORIENTED_EDGE('',*,*,#10229,.T.);
#13653=ORIENTED_EDGE('',*,*,#10230,.T.);
#13654=ORIENTED_EDGE('',*,*,#10231,.T.);
#13655=ORIENTED_EDGE('',*,*,#10232,.T.);
#13656=ORIENTED_EDGE('',*,*,#10233,.T.);
#13657=ORIENTED_EDGE('',*,*,#10234,.T.);
#13658=ORIENTED_EDGE('',*,*,#10235,.T.);
#13659=ORIENTED_EDGE('',*,*,#10236,.T.);
#13660=ORIENTED_EDGE('',*,*,#10199,.F.);
#13661=ORIENTED_EDGE('',*,*,#10237,.F.);
#13662=ORIENTED_EDGE('',*,*,#10238,.F.);
#13663=ORIENTED_EDGE('',*,*,#10239,.T.);
#13664=ORIENTED_EDGE('',*,*,#10200,.F.);
#13665=ORIENTED_EDGE('',*,*,#10236,.F.);
#13666=ORIENTED_EDGE('',*,*,#10240,.F.);
#13667=ORIENTED_EDGE('',*,*,#10241,.T.);
#13668=ORIENTED_EDGE('',*,*,#10201,.F.);
#13669=ORIENTED_EDGE('',*,*,#10239,.F.);
#13670=ORIENTED_EDGE('',*,*,#10242,.F.);
#13671=ORIENTED_EDGE('',*,*,#10243,.T.);
#13672=ORIENTED_EDGE('',*,*,#10202,.F.);
#13673=ORIENTED_EDGE('',*,*,#10241,.F.);
#13674=ORIENTED_EDGE('',*,*,#10244,.F.);
#13675=ORIENTED_EDGE('',*,*,#10245,.T.);
#13676=ORIENTED_EDGE('',*,*,#10246,.T.);
#13677=ORIENTED_EDGE('',*,*,#10247,.T.);
#13678=ORIENTED_EDGE('',*,*,#10203,.F.);
#13679=ORIENTED_EDGE('',*,*,#10243,.F.);
#13680=ORIENTED_EDGE('',*,*,#10248,.F.);
#13681=ORIENTED_EDGE('',*,*,#10204,.F.);
#13682=ORIENTED_EDGE('',*,*,#10247,.F.);
#13683=ORIENTED_EDGE('',*,*,#10249,.T.);
#13684=ORIENTED_EDGE('',*,*,#10250,.T.);
#13685=ORIENTED_EDGE('',*,*,#10238,.T.);
#13686=ORIENTED_EDGE('',*,*,#10251,.F.);
#13687=ORIENTED_EDGE('',*,*,#10252,.F.);
#13688=ORIENTED_EDGE('',*,*,#10253,.F.);
#13689=ORIENTED_EDGE('',*,*,#10254,.F.);
#13690=ORIENTED_EDGE('',*,*,#10255,.F.);
#13691=ORIENTED_EDGE('',*,*,#10256,.F.);
#13692=ORIENTED_EDGE('',*,*,#10257,.F.);
#13693=ORIENTED_EDGE('',*,*,#10258,.F.);
#13694=ORIENTED_EDGE('',*,*,#10259,.F.);
#13695=ORIENTED_EDGE('',*,*,#10197,.F.);
#13696=ORIENTED_EDGE('',*,*,#10194,.F.);
#13697=ORIENTED_EDGE('',*,*,#10191,.F.);
#13698=ORIENTED_EDGE('',*,*,#10188,.F.);
#13699=ORIENTED_EDGE('',*,*,#10185,.F.);
#13700=ORIENTED_EDGE('',*,*,#10182,.F.);
#13701=ORIENTED_EDGE('',*,*,#10179,.F.);
#13702=ORIENTED_EDGE('',*,*,#10260,.F.);
#13703=ORIENTED_EDGE('',*,*,#10261,.F.);
#13704=ORIENTED_EDGE('',*,*,#10262,.F.);
#13705=ORIENTED_EDGE('',*,*,#10263,.F.);
#13706=ORIENTED_EDGE('',*,*,#10264,.F.);
#13707=ORIENTED_EDGE('',*,*,#10265,.F.);
#13708=ORIENTED_EDGE('',*,*,#10266,.F.);
#13709=ORIENTED_EDGE('',*,*,#10267,.F.);
#13710=ORIENTED_EDGE('',*,*,#10268,.F.);
#13711=ORIENTED_EDGE('',*,*,#10269,.F.);
#13712=ORIENTED_EDGE('',*,*,#10270,.F.);
#13713=ORIENTED_EDGE('',*,*,#10271,.F.);
#13714=ORIENTED_EDGE('',*,*,#10272,.F.);
#13715=ORIENTED_EDGE('',*,*,#10273,.F.);
#13716=ORIENTED_EDGE('',*,*,#10274,.F.);
#13717=ORIENTED_EDGE('',*,*,#10275,.F.);
#13718=ORIENTED_EDGE('',*,*,#10276,.F.);
#13719=ORIENTED_EDGE('',*,*,#10277,.F.);
#13720=ORIENTED_EDGE('',*,*,#10278,.F.);
#13721=ORIENTED_EDGE('',*,*,#10279,.F.);
#13722=ORIENTED_EDGE('',*,*,#10280,.F.);
#13723=ORIENTED_EDGE('',*,*,#10281,.F.);
#13724=ORIENTED_EDGE('',*,*,#10249,.F.);
#13725=ORIENTED_EDGE('',*,*,#10248,.T.);
#13726=ORIENTED_EDGE('',*,*,#10244,.T.);
#13727=ORIENTED_EDGE('',*,*,#10242,.T.);
#13728=ORIENTED_EDGE('',*,*,#10240,.T.);
#13729=ORIENTED_EDGE('',*,*,#10282,.F.);
#13730=ORIENTED_EDGE('',*,*,#10277,.T.);
#13731=ORIENTED_EDGE('',*,*,#10283,.F.);
#13732=ORIENTED_EDGE('',*,*,#10209,.T.);
#13733=ORIENTED_EDGE('',*,*,#10284,.F.);
#13734=ORIENTED_EDGE('',*,*,#10278,.T.);
#13735=ORIENTED_EDGE('',*,*,#10282,.T.);
#13736=ORIENTED_EDGE('',*,*,#10208,.T.);
#13737=ORIENTED_EDGE('',*,*,#10285,.F.);
#13738=ORIENTED_EDGE('',*,*,#10279,.T.);
#13739=ORIENTED_EDGE('',*,*,#10284,.T.);
#13740=ORIENTED_EDGE('',*,*,#10207,.T.);
#13741=ORIENTED_EDGE('',*,*,#10286,.F.);
#13742=ORIENTED_EDGE('',*,*,#10280,.T.);
#13743=ORIENTED_EDGE('',*,*,#10285,.T.);
#13744=ORIENTED_EDGE('',*,*,#10206,.T.);
#13745=ORIENTED_EDGE('',*,*,#10287,.T.);
#13746=ORIENTED_EDGE('',*,*,#10288,.T.);
#13747=ORIENTED_EDGE('',*,*,#10250,.F.);
#13748=ORIENTED_EDGE('',*,*,#10281,.T.);
#13749=ORIENTED_EDGE('',*,*,#10286,.T.);
#13750=ORIENTED_EDGE('',*,*,#10205,.T.);
#13751=ORIENTED_EDGE('',*,*,#10246,.F.);
#13752=ORIENTED_EDGE('',*,*,#10289,.T.);
#13753=ORIENTED_EDGE('',*,*,#10290,.F.);
#13754=ORIENTED_EDGE('',*,*,#10289,.F.);
#13755=ORIENTED_EDGE('',*,*,#10288,.F.);
#13756=ORIENTED_EDGE('',*,*,#10291,.T.);
#13757=ORIENTED_EDGE('',*,*,#10292,.F.);
#13758=ORIENTED_EDGE('',*,*,#10291,.F.);
#13759=ORIENTED_EDGE('',*,*,#10245,.F.);
#13760=ORIENTED_EDGE('',*,*,#10293,.T.);
#13761=ORIENTED_EDGE('',*,*,#10294,.F.);
#13762=ORIENTED_EDGE('',*,*,#10293,.F.);
#13763=ORIENTED_EDGE('',*,*,#10287,.F.);
#13764=ORIENTED_EDGE('',*,*,#10295,.T.);
#13765=ORIENTED_EDGE('',*,*,#10296,.F.);
#13766=ORIENTED_EDGE('',*,*,#10295,.F.);
#13767=ORIENTED_EDGE('',*,*,#10235,.F.);
#13768=ORIENTED_EDGE('',*,*,#10297,.F.);
#13769=ORIENTED_EDGE('',*,*,#10251,.T.);
#13770=ORIENTED_EDGE('',*,*,#10237,.T.);
#13771=ORIENTED_EDGE('',*,*,#10234,.F.);
#13772=ORIENTED_EDGE('',*,*,#10298,.F.);
#13773=ORIENTED_EDGE('',*,*,#10252,.T.);
#13774=ORIENTED_EDGE('',*,*,#10297,.T.);
#13775=ORIENTED_EDGE('',*,*,#10233,.F.);
#13776=ORIENTED_EDGE('',*,*,#10299,.F.);
#13777=ORIENTED_EDGE('',*,*,#10253,.T.);
#13778=ORIENTED_EDGE('',*,*,#10298,.T.);
#13779=ORIENTED_EDGE('',*,*,#10290,.T.);
#13780=ORIENTED_EDGE('',*,*,#10294,.T.);
#13781=ORIENTED_EDGE('',*,*,#10232,.F.);
#13782=ORIENTED_EDGE('',*,*,#10300,.F.);
#13783=ORIENTED_EDGE('',*,*,#10254,.T.);
#13784=ORIENTED_EDGE('',*,*,#10299,.T.);
#13785=ORIENTED_EDGE('',*,*,#10231,.F.);
#13786=ORIENTED_EDGE('',*,*,#10301,.F.);
#13787=ORIENTED_EDGE('',*,*,#10255,.T.);
#13788=ORIENTED_EDGE('',*,*,#10300,.T.);
#13789=ORIENTED_EDGE('',*,*,#10230,.F.);
#13790=ORIENTED_EDGE('',*,*,#10302,.F.);
#13791=ORIENTED_EDGE('',*,*,#10256,.T.);
#13792=ORIENTED_EDGE('',*,*,#10301,.T.);
#13793=ORIENTED_EDGE('',*,*,#10229,.F.);
#13794=ORIENTED_EDGE('',*,*,#10303,.F.);
#13795=ORIENTED_EDGE('',*,*,#10257,.T.);
#13796=ORIENTED_EDGE('',*,*,#10302,.T.);
#13797=ORIENTED_EDGE('',*,*,#10228,.F.);
#13798=ORIENTED_EDGE('',*,*,#10304,.F.);
#13799=ORIENTED_EDGE('',*,*,#10258,.T.);
#13800=ORIENTED_EDGE('',*,*,#10303,.T.);
#13801=ORIENTED_EDGE('',*,*,#10227,.F.);
#13802=ORIENTED_EDGE('',*,*,#10198,.F.);
#13803=ORIENTED_EDGE('',*,*,#10259,.T.);
#13804=ORIENTED_EDGE('',*,*,#10304,.T.);
#13805=ORIENTED_EDGE('',*,*,#10210,.F.);
#13806=ORIENTED_EDGE('',*,*,#10283,.T.);
#13807=ORIENTED_EDGE('',*,*,#10276,.T.);
#13808=ORIENTED_EDGE('',*,*,#10305,.T.);
#13809=ORIENTED_EDGE('',*,*,#10211,.F.);
#13810=ORIENTED_EDGE('',*,*,#10305,.F.);
#13811=ORIENTED_EDGE('',*,*,#10275,.T.);
#13812=ORIENTED_EDGE('',*,*,#10306,.T.);
#13813=ORIENTED_EDGE('',*,*,#10212,.F.);
#13814=ORIENTED_EDGE('',*,*,#10306,.F.);
#13815=ORIENTED_EDGE('',*,*,#10274,.T.);
#13816=ORIENTED_EDGE('',*,*,#10307,.T.);
#13817=ORIENTED_EDGE('',*,*,#10296,.T.);
#13818=ORIENTED_EDGE('',*,*,#10292,.T.);
#13819=ORIENTED_EDGE('',*,*,#10213,.F.);
#13820=ORIENTED_EDGE('',*,*,#10307,.F.);
#13821=ORIENTED_EDGE('',*,*,#10273,.T.);
#13822=ORIENTED_EDGE('',*,*,#10308,.T.);
#13823=ORIENTED_EDGE('',*,*,#10214,.F.);
#13824=ORIENTED_EDGE('',*,*,#10308,.F.);
#13825=ORIENTED_EDGE('',*,*,#10272,.T.);
#13826=ORIENTED_EDGE('',*,*,#10309,.T.);
#13827=ORIENTED_EDGE('',*,*,#10215,.F.);
#13828=ORIENTED_EDGE('',*,*,#10309,.F.);
#13829=ORIENTED_EDGE('',*,*,#10271,.T.);
#13830=ORIENTED_EDGE('',*,*,#10310,.F.);
#13831=ORIENTED_EDGE('',*,*,#10216,.F.);
#13832=ORIENTED_EDGE('',*,*,#10310,.T.);
#13833=ORIENTED_EDGE('',*,*,#10270,.T.);
#13834=ORIENTED_EDGE('',*,*,#10311,.T.);
#13835=ORIENTED_EDGE('',*,*,#10217,.F.);
#13836=ORIENTED_EDGE('',*,*,#10311,.F.);
#13837=ORIENTED_EDGE('',*,*,#10269,.T.);
#13838=ORIENTED_EDGE('',*,*,#10312,.T.);
#13839=ORIENTED_EDGE('',*,*,#10218,.F.);
#13840=ORIENTED_EDGE('',*,*,#10312,.F.);
#13841=ORIENTED_EDGE('',*,*,#10268,.T.);
#13842=ORIENTED_EDGE('',*,*,#10313,.T.);
#13843=ORIENTED_EDGE('',*,*,#10219,.F.);
#13844=ORIENTED_EDGE('',*,*,#10313,.F.);
#13845=ORIENTED_EDGE('',*,*,#10267,.T.);
#13846=ORIENTED_EDGE('',*,*,#10314,.T.);
#13847=ORIENTED_EDGE('',*,*,#10220,.F.);
#13848=ORIENTED_EDGE('',*,*,#10314,.F.);
#13849=ORIENTED_EDGE('',*,*,#10266,.T.);
#13850=ORIENTED_EDGE('',*,*,#10315,.T.);
#13851=ORIENTED_EDGE('',*,*,#10221,.F.);
#13852=ORIENTED_EDGE('',*,*,#10315,.F.);
#13853=ORIENTED_EDGE('',*,*,#10265,.T.);
#13854=ORIENTED_EDGE('',*,*,#10316,.T.);
#13855=ORIENTED_EDGE('',*,*,#10222,.F.);
#13856=ORIENTED_EDGE('',*,*,#10316,.F.);
#13857=ORIENTED_EDGE('',*,*,#10264,.T.);
#13858=ORIENTED_EDGE('',*,*,#10317,.T.);
#13859=ORIENTED_EDGE('',*,*,#10223,.F.);
#13860=ORIENTED_EDGE('',*,*,#10317,.F.);
#13861=ORIENTED_EDGE('',*,*,#10263,.T.);
#13862=ORIENTED_EDGE('',*,*,#10318,.T.);
#13863=ORIENTED_EDGE('',*,*,#10224,.F.);
#13864=ORIENTED_EDGE('',*,*,#10318,.F.);
#13865=ORIENTED_EDGE('',*,*,#10262,.T.);
#13866=ORIENTED_EDGE('',*,*,#10319,.T.);
#13867=ORIENTED_EDGE('',*,*,#10225,.F.);
#13868=ORIENTED_EDGE('',*,*,#10319,.F.);
#13869=ORIENTED_EDGE('',*,*,#10261,.T.);
#13870=ORIENTED_EDGE('',*,*,#10320,.T.);
#13871=ORIENTED_EDGE('',*,*,#10226,.F.);
#13872=ORIENTED_EDGE('',*,*,#10320,.F.);
#13873=ORIENTED_EDGE('',*,*,#10260,.T.);
#13874=ORIENTED_EDGE('',*,*,#10178,.T.);
#13875=ORIENTED_EDGE('',*,*,#10321,.F.);
#13876=ORIENTED_EDGE('',*,*,#10322,.F.);
#13877=ORIENTED_EDGE('',*,*,#10323,.F.);
#13878=ORIENTED_EDGE('',*,*,#10324,.T.);
#13879=ORIENTED_EDGE('',*,*,#10325,.F.);
#13880=ORIENTED_EDGE('',*,*,#10324,.F.);
#13881=ORIENTED_EDGE('',*,*,#10326,.F.);
#13882=ORIENTED_EDGE('',*,*,#10327,.T.);
#13883=ORIENTED_EDGE('',*,*,#10328,.F.);
#13884=ORIENTED_EDGE('',*,*,#10327,.F.);
#13885=ORIENTED_EDGE('',*,*,#10329,.F.);
#13886=ORIENTED_EDGE('',*,*,#10330,.T.);
#13887=ORIENTED_EDGE('',*,*,#10331,.F.);
#13888=ORIENTED_EDGE('',*,*,#10330,.F.);
#13889=ORIENTED_EDGE('',*,*,#10332,.F.);
#13890=ORIENTED_EDGE('',*,*,#10333,.T.);
#13891=ORIENTED_EDGE('',*,*,#10334,.F.);
#13892=ORIENTED_EDGE('',*,*,#10333,.F.);
#13893=ORIENTED_EDGE('',*,*,#10335,.F.);
#13894=ORIENTED_EDGE('',*,*,#10336,.T.);
#13895=ORIENTED_EDGE('',*,*,#10337,.F.);
#13896=ORIENTED_EDGE('',*,*,#10336,.F.);
#13897=ORIENTED_EDGE('',*,*,#10338,.F.);
#13898=ORIENTED_EDGE('',*,*,#10339,.T.);
#13899=ORIENTED_EDGE('',*,*,#10340,.F.);
#13900=ORIENTED_EDGE('',*,*,#10339,.F.);
#13901=ORIENTED_EDGE('',*,*,#10341,.F.);
#13902=ORIENTED_EDGE('',*,*,#10342,.T.);
#13903=ORIENTED_EDGE('',*,*,#10343,.F.);
#13904=ORIENTED_EDGE('',*,*,#10342,.F.);
#13905=ORIENTED_EDGE('',*,*,#10344,.F.);
#13906=ORIENTED_EDGE('',*,*,#10345,.T.);
#13907=ORIENTED_EDGE('',*,*,#10346,.T.);
#13908=ORIENTED_EDGE('',*,*,#10347,.F.);
#13909=ORIENTED_EDGE('',*,*,#10348,.F.);
#13910=ORIENTED_EDGE('',*,*,#10349,.T.);
#13911=ORIENTED_EDGE('',*,*,#10350,.T.);
#13912=ORIENTED_EDGE('',*,*,#10349,.F.);
#13913=ORIENTED_EDGE('',*,*,#10351,.F.);
#13914=ORIENTED_EDGE('',*,*,#10352,.T.);
#13915=ORIENTED_EDGE('',*,*,#10353,.T.);
#13916=ORIENTED_EDGE('',*,*,#10352,.F.);
#13917=ORIENTED_EDGE('',*,*,#10354,.F.);
#13918=ORIENTED_EDGE('',*,*,#10355,.T.);
#13919=ORIENTED_EDGE('',*,*,#10356,.F.);
#13920=ORIENTED_EDGE('',*,*,#10355,.F.);
#13921=ORIENTED_EDGE('',*,*,#10357,.F.);
#13922=ORIENTED_EDGE('',*,*,#10358,.T.);
#13923=ORIENTED_EDGE('',*,*,#10359,.F.);
#13924=ORIENTED_EDGE('',*,*,#10358,.F.);
#13925=ORIENTED_EDGE('',*,*,#10360,.F.);
#13926=ORIENTED_EDGE('',*,*,#10361,.T.);
#13927=ORIENTED_EDGE('',*,*,#10362,.F.);
#13928=ORIENTED_EDGE('',*,*,#10361,.F.);
#13929=ORIENTED_EDGE('',*,*,#10363,.F.);
#13930=ORIENTED_EDGE('',*,*,#10364,.T.);
#13931=ORIENTED_EDGE('',*,*,#10365,.F.);
#13932=ORIENTED_EDGE('',*,*,#10364,.F.);
#13933=ORIENTED_EDGE('',*,*,#10366,.F.);
#13934=ORIENTED_EDGE('',*,*,#10367,.T.);
#13935=ORIENTED_EDGE('',*,*,#10368,.F.);
#13936=ORIENTED_EDGE('',*,*,#10367,.F.);
#13937=ORIENTED_EDGE('',*,*,#10369,.F.);
#13938=ORIENTED_EDGE('',*,*,#10370,.T.);
#13939=ORIENTED_EDGE('',*,*,#10371,.T.);
#13940=ORIENTED_EDGE('',*,*,#10372,.T.);
#13941=ORIENTED_EDGE('',*,*,#10369,.T.);
#13942=ORIENTED_EDGE('',*,*,#10366,.T.);
#13943=ORIENTED_EDGE('',*,*,#10363,.T.);
#13944=ORIENTED_EDGE('',*,*,#10360,.T.);
#13945=ORIENTED_EDGE('',*,*,#10357,.T.);
#13946=ORIENTED_EDGE('',*,*,#10354,.T.);
#13947=ORIENTED_EDGE('',*,*,#10351,.T.);
#13948=ORIENTED_EDGE('',*,*,#10348,.T.);
#13949=ORIENTED_EDGE('',*,*,#10373,.T.);
#13950=ORIENTED_EDGE('',*,*,#10344,.T.);
#13951=ORIENTED_EDGE('',*,*,#10341,.T.);
#13952=ORIENTED_EDGE('',*,*,#10338,.T.);
#13953=ORIENTED_EDGE('',*,*,#10335,.T.);
#13954=ORIENTED_EDGE('',*,*,#10332,.T.);
#13955=ORIENTED_EDGE('',*,*,#10329,.T.);
#13956=ORIENTED_EDGE('',*,*,#10326,.T.);
#13957=ORIENTED_EDGE('',*,*,#10323,.T.);
#13958=ORIENTED_EDGE('',*,*,#10374,.T.);
#13959=ORIENTED_EDGE('',*,*,#10375,.T.);
#13960=ORIENTED_EDGE('',*,*,#10376,.T.);
#13961=ORIENTED_EDGE('',*,*,#10377,.T.);
#13962=ORIENTED_EDGE('',*,*,#10378,.T.);
#13963=ORIENTED_EDGE('',*,*,#10379,.T.);
#13964=ORIENTED_EDGE('',*,*,#10380,.T.);
#13965=ORIENTED_EDGE('',*,*,#10381,.T.);
#13966=ORIENTED_EDGE('',*,*,#10382,.T.);
#13967=ORIENTED_EDGE('',*,*,#10383,.T.);
#13968=ORIENTED_EDGE('',*,*,#10384,.T.);
#13969=ORIENTED_EDGE('',*,*,#10385,.T.);
#13970=ORIENTED_EDGE('',*,*,#10386,.T.);
#13971=ORIENTED_EDGE('',*,*,#10387,.T.);
#13972=ORIENTED_EDGE('',*,*,#10388,.T.);
#13973=ORIENTED_EDGE('',*,*,#10389,.T.);
#13974=ORIENTED_EDGE('',*,*,#10390,.T.);
#13975=ORIENTED_EDGE('',*,*,#10391,.F.);
#13976=ORIENTED_EDGE('',*,*,#10345,.F.);
#13977=ORIENTED_EDGE('',*,*,#10373,.F.);
#13978=ORIENTED_EDGE('',*,*,#10347,.T.);
#13979=ORIENTED_EDGE('',*,*,#10392,.F.);
#13980=ORIENTED_EDGE('',*,*,#10370,.F.);
#13981=ORIENTED_EDGE('',*,*,#10372,.F.);
#13982=ORIENTED_EDGE('',*,*,#10393,.F.);
#13983=ORIENTED_EDGE('',*,*,#10394,.F.);
#13984=ORIENTED_EDGE('',*,*,#10393,.T.);
#13985=ORIENTED_EDGE('',*,*,#10371,.F.);
#13986=ORIENTED_EDGE('',*,*,#10395,.T.);
#13987=ORIENTED_EDGE('',*,*,#10396,.F.);
#13988=ORIENTED_EDGE('',*,*,#10395,.F.);
#13989=ORIENTED_EDGE('',*,*,#10390,.F.);
#13990=ORIENTED_EDGE('',*,*,#10397,.T.);
#13991=ORIENTED_EDGE('',*,*,#10398,.F.);
#13992=ORIENTED_EDGE('',*,*,#10397,.F.);
#13993=ORIENTED_EDGE('',*,*,#10389,.F.);
#13994=ORIENTED_EDGE('',*,*,#10399,.T.);
#13995=ORIENTED_EDGE('',*,*,#10400,.F.);
#13996=ORIENTED_EDGE('',*,*,#10399,.F.);
#13997=ORIENTED_EDGE('',*,*,#10388,.F.);
#13998=ORIENTED_EDGE('',*,*,#10401,.T.);
#13999=ORIENTED_EDGE('',*,*,#10402,.F.);
#14000=ORIENTED_EDGE('',*,*,#10401,.F.);
#14001=ORIENTED_EDGE('',*,*,#10387,.F.);
#14002=ORIENTED_EDGE('',*,*,#10403,.T.);
#14003=ORIENTED_EDGE('',*,*,#10404,.F.);
#14004=ORIENTED_EDGE('',*,*,#10403,.F.);
#14005=ORIENTED_EDGE('',*,*,#10386,.F.);
#14006=ORIENTED_EDGE('',*,*,#10405,.T.);
#14007=ORIENTED_EDGE('',*,*,#10406,.F.);
#14008=ORIENTED_EDGE('',*,*,#10405,.F.);
#14009=ORIENTED_EDGE('',*,*,#10385,.F.);
#14010=ORIENTED_EDGE('',*,*,#10407,.T.);
#14011=ORIENTED_EDGE('',*,*,#10408,.F.);
#14012=ORIENTED_EDGE('',*,*,#10407,.F.);
#14013=ORIENTED_EDGE('',*,*,#10384,.F.);
#14014=ORIENTED_EDGE('',*,*,#10409,.T.);
#14015=ORIENTED_EDGE('',*,*,#10410,.F.);
#14016=ORIENTED_EDGE('',*,*,#10409,.F.);
#14017=ORIENTED_EDGE('',*,*,#10383,.F.);
#14018=ORIENTED_EDGE('',*,*,#10411,.T.);
#14019=ORIENTED_EDGE('',*,*,#10412,.F.);
#14020=ORIENTED_EDGE('',*,*,#10411,.F.);
#14021=ORIENTED_EDGE('',*,*,#10382,.F.);
#14022=ORIENTED_EDGE('',*,*,#10413,.T.);
#14023=ORIENTED_EDGE('',*,*,#10414,.F.);
#14024=ORIENTED_EDGE('',*,*,#10413,.F.);
#14025=ORIENTED_EDGE('',*,*,#10381,.F.);
#14026=ORIENTED_EDGE('',*,*,#10415,.T.);
#14027=ORIENTED_EDGE('',*,*,#10416,.F.);
#14028=ORIENTED_EDGE('',*,*,#10415,.F.);
#14029=ORIENTED_EDGE('',*,*,#10380,.F.);
#14030=ORIENTED_EDGE('',*,*,#10417,.T.);
#14031=ORIENTED_EDGE('',*,*,#10418,.F.);
#14032=ORIENTED_EDGE('',*,*,#10417,.F.);
#14033=ORIENTED_EDGE('',*,*,#10379,.F.);
#14034=ORIENTED_EDGE('',*,*,#10419,.T.);
#14035=ORIENTED_EDGE('',*,*,#10420,.F.);
#14036=ORIENTED_EDGE('',*,*,#10419,.F.);
#14037=ORIENTED_EDGE('',*,*,#10378,.F.);
#14038=ORIENTED_EDGE('',*,*,#10421,.T.);
#14039=ORIENTED_EDGE('',*,*,#10422,.F.);
#14040=ORIENTED_EDGE('',*,*,#10421,.F.);
#14041=ORIENTED_EDGE('',*,*,#10377,.F.);
#14042=ORIENTED_EDGE('',*,*,#10423,.T.);
#14043=ORIENTED_EDGE('',*,*,#10424,.F.);
#14044=ORIENTED_EDGE('',*,*,#10423,.F.);
#14045=ORIENTED_EDGE('',*,*,#10376,.F.);
#14046=ORIENTED_EDGE('',*,*,#10425,.T.);
#14047=ORIENTED_EDGE('',*,*,#10426,.F.);
#14048=ORIENTED_EDGE('',*,*,#10425,.F.);
#14049=ORIENTED_EDGE('',*,*,#10375,.F.);
#14050=ORIENTED_EDGE('',*,*,#10427,.T.);
#14051=ORIENTED_EDGE('',*,*,#10428,.F.);
#14052=ORIENTED_EDGE('',*,*,#10427,.F.);
#14053=ORIENTED_EDGE('',*,*,#10374,.F.);
#14054=ORIENTED_EDGE('',*,*,#10322,.T.);
#14055=ORIENTED_EDGE('',*,*,#10392,.T.);
#14056=ORIENTED_EDGE('',*,*,#10394,.T.);
#14057=ORIENTED_EDGE('',*,*,#10396,.T.);
#14058=ORIENTED_EDGE('',*,*,#10398,.T.);
#14059=ORIENTED_EDGE('',*,*,#10400,.T.);
#14060=ORIENTED_EDGE('',*,*,#10402,.T.);
#14061=ORIENTED_EDGE('',*,*,#10404,.T.);
#14062=ORIENTED_EDGE('',*,*,#10406,.T.);
#14063=ORIENTED_EDGE('',*,*,#10408,.T.);
#14064=ORIENTED_EDGE('',*,*,#10410,.T.);
#14065=ORIENTED_EDGE('',*,*,#10412,.T.);
#14066=ORIENTED_EDGE('',*,*,#10414,.T.);
#14067=ORIENTED_EDGE('',*,*,#10416,.T.);
#14068=ORIENTED_EDGE('',*,*,#10418,.T.);
#14069=ORIENTED_EDGE('',*,*,#10420,.T.);
#14070=ORIENTED_EDGE('',*,*,#10422,.T.);
#14071=ORIENTED_EDGE('',*,*,#10424,.T.);
#14072=ORIENTED_EDGE('',*,*,#10426,.T.);
#14073=ORIENTED_EDGE('',*,*,#10428,.T.);
#14074=ORIENTED_EDGE('',*,*,#10321,.T.);
#14075=ORIENTED_EDGE('',*,*,#10325,.T.);
#14076=ORIENTED_EDGE('',*,*,#10328,.T.);
#14077=ORIENTED_EDGE('',*,*,#10331,.T.);
#14078=ORIENTED_EDGE('',*,*,#10334,.T.);
#14079=ORIENTED_EDGE('',*,*,#10337,.T.);
#14080=ORIENTED_EDGE('',*,*,#10340,.T.);
#14081=ORIENTED_EDGE('',*,*,#10343,.T.);
#14082=ORIENTED_EDGE('',*,*,#10391,.T.);
#14083=ORIENTED_EDGE('',*,*,#10346,.F.);
#14084=ORIENTED_EDGE('',*,*,#10350,.F.);
#14085=ORIENTED_EDGE('',*,*,#10353,.F.);
#14086=ORIENTED_EDGE('',*,*,#10356,.T.);
#14087=ORIENTED_EDGE('',*,*,#10359,.T.);
#14088=ORIENTED_EDGE('',*,*,#10362,.T.);
#14089=ORIENTED_EDGE('',*,*,#10365,.T.);
#14090=ORIENTED_EDGE('',*,*,#10368,.T.);
#14091=ORIENTED_EDGE('',*,*,#10429,.T.);
#14092=ORIENTED_EDGE('',*,*,#10430,.T.);
#14093=ORIENTED_EDGE('',*,*,#10431,.F.);
#14094=ORIENTED_EDGE('',*,*,#10430,.F.);
#14095=ORIENTED_EDGE('',*,*,#10432,.T.);
#14096=ORIENTED_EDGE('',*,*,#10433,.T.);
#14097=ORIENTED_EDGE('',*,*,#10429,.F.);
#14098=ORIENTED_EDGE('',*,*,#10433,.F.);
#14099=ORIENTED_EDGE('',*,*,#10434,.T.);
#14100=ORIENTED_EDGE('',*,*,#10435,.T.);
#14101=ORIENTED_EDGE('',*,*,#10436,.F.);
#14102=ORIENTED_EDGE('',*,*,#10435,.F.);
#14103=ORIENTED_EDGE('',*,*,#10437,.T.);
#14104=ORIENTED_EDGE('',*,*,#10438,.T.);
#14105=ORIENTED_EDGE('',*,*,#10434,.F.);
#14106=ORIENTED_EDGE('',*,*,#10438,.F.);
#14107=ORIENTED_EDGE('',*,*,#10439,.T.);
#14108=ORIENTED_EDGE('',*,*,#10440,.T.);
#14109=ORIENTED_EDGE('',*,*,#10441,.T.);
#14110=ORIENTED_EDGE('',*,*,#10442,.T.);
#14111=ORIENTED_EDGE('',*,*,#10443,.T.);
#14112=ORIENTED_EDGE('',*,*,#10444,.T.);
#14113=ORIENTED_EDGE('',*,*,#10445,.T.);
#14114=ORIENTED_EDGE('',*,*,#10446,.T.);
#14115=ORIENTED_EDGE('',*,*,#10447,.T.);
#14116=ORIENTED_EDGE('',*,*,#10448,.T.);
#14117=ORIENTED_EDGE('',*,*,#10437,.F.);
#14118=ORIENTED_EDGE('',*,*,#10448,.F.);
#14119=ORIENTED_EDGE('',*,*,#10449,.T.);
#14120=ORIENTED_EDGE('',*,*,#10450,.T.);
#14121=ORIENTED_EDGE('',*,*,#10451,.T.);
#14122=ORIENTED_EDGE('',*,*,#10452,.T.);
#14123=ORIENTED_EDGE('',*,*,#10453,.T.);
#14124=ORIENTED_EDGE('',*,*,#10454,.T.);
#14125=ORIENTED_EDGE('',*,*,#10455,.T.);
#14126=ORIENTED_EDGE('',*,*,#10456,.T.);
#14127=ORIENTED_EDGE('',*,*,#10457,.T.);
#14128=ORIENTED_EDGE('',*,*,#10458,.T.);
#14129=ORIENTED_EDGE('',*,*,#10459,.F.);
#14130=ORIENTED_EDGE('',*,*,#10458,.F.);
#14131=ORIENTED_EDGE('',*,*,#10460,.T.);
#14132=ORIENTED_EDGE('',*,*,#10461,.T.);
#14133=ORIENTED_EDGE('',*,*,#10457,.F.);
#14134=ORIENTED_EDGE('',*,*,#10461,.F.);
#14135=ORIENTED_EDGE('',*,*,#10459,.T.);
#14136=ORIENTED_EDGE('',*,*,#10462,.T.);
#14137=ORIENTED_EDGE('',*,*,#10463,.T.);
#14138=ORIENTED_EDGE('',*,*,#10464,.F.);
#14139=ORIENTED_EDGE('',*,*,#10465,.F.);
#14140=ORIENTED_EDGE('',*,*,#10466,.F.);
#14141=ORIENTED_EDGE('',*,*,#10467,.T.);
#14142=ORIENTED_EDGE('',*,*,#10468,.F.);
#14143=ORIENTED_EDGE('',*,*,#10469,.F.);
#14144=ORIENTED_EDGE('',*,*,#10470,.F.);
#14145=ORIENTED_EDGE('',*,*,#10471,.T.);
#14146=ORIENTED_EDGE('',*,*,#10472,.F.);
#14147=ORIENTED_EDGE('',*,*,#10473,.F.);
#14148=ORIENTED_EDGE('',*,*,#10474,.F.);
#14149=ORIENTED_EDGE('',*,*,#10475,.T.);
#14150=ORIENTED_EDGE('',*,*,#10476,.F.);
#14151=ORIENTED_EDGE('',*,*,#10477,.F.);
#14152=ORIENTED_EDGE('',*,*,#10478,.F.);
#14153=ORIENTED_EDGE('',*,*,#10479,.T.);
#14154=ORIENTED_EDGE('',*,*,#10480,.F.);
#14155=ORIENTED_EDGE('',*,*,#10481,.F.);
#14156=ORIENTED_EDGE('',*,*,#10482,.F.);
#14157=ORIENTED_EDGE('',*,*,#10483,.T.);
#14158=ORIENTED_EDGE('',*,*,#10484,.F.);
#14159=ORIENTED_EDGE('',*,*,#10485,.F.);
#14160=ORIENTED_EDGE('',*,*,#10486,.F.);
#14161=ORIENTED_EDGE('',*,*,#10487,.T.);
#14162=ORIENTED_EDGE('',*,*,#10488,.F.);
#14163=ORIENTED_EDGE('',*,*,#10489,.F.);
#14164=ORIENTED_EDGE('',*,*,#10490,.F.);
#14165=ORIENTED_EDGE('',*,*,#10491,.T.);
#14166=ORIENTED_EDGE('',*,*,#10492,.F.);
#14167=ORIENTED_EDGE('',*,*,#10493,.F.);
#14168=ORIENTED_EDGE('',*,*,#10494,.F.);
#14169=ORIENTED_EDGE('',*,*,#10495,.T.);
#14170=ORIENTED_EDGE('',*,*,#10462,.F.);
#14171=ORIENTED_EDGE('',*,*,#10493,.T.);
#14172=ORIENTED_EDGE('',*,*,#10496,.F.);
#14173=ORIENTED_EDGE('',*,*,#10497,.F.);
#14174=ORIENTED_EDGE('',*,*,#10498,.F.);
#14175=ORIENTED_EDGE('',*,*,#10499,.F.);
#14176=ORIENTED_EDGE('',*,*,#10500,.F.);
#14177=ORIENTED_EDGE('',*,*,#10465,.T.);
#14178=ORIENTED_EDGE('',*,*,#10501,.F.);
#14179=ORIENTED_EDGE('',*,*,#10489,.T.);
#14180=ORIENTED_EDGE('',*,*,#10502,.F.);
#14181=ORIENTED_EDGE('',*,*,#10503,.F.);
#14182=ORIENTED_EDGE('',*,*,#10504,.F.);
#14183=ORIENTED_EDGE('',*,*,#10485,.T.);
#14184=ORIENTED_EDGE('',*,*,#10505,.F.);
#14185=ORIENTED_EDGE('',*,*,#10506,.F.);
#14186=ORIENTED_EDGE('',*,*,#10507,.F.);
#14187=ORIENTED_EDGE('',*,*,#10481,.T.);
#14188=ORIENTED_EDGE('',*,*,#10508,.F.);
#14189=ORIENTED_EDGE('',*,*,#10509,.F.);
#14190=ORIENTED_EDGE('',*,*,#10510,.F.);
#14191=ORIENTED_EDGE('',*,*,#10477,.T.);
#14192=ORIENTED_EDGE('',*,*,#10511,.F.);
#14193=ORIENTED_EDGE('',*,*,#10512,.F.);
#14194=ORIENTED_EDGE('',*,*,#10513,.F.);
#14195=ORIENTED_EDGE('',*,*,#10473,.T.);
#14196=ORIENTED_EDGE('',*,*,#10514,.F.);
#14197=ORIENTED_EDGE('',*,*,#10515,.F.);
#14198=ORIENTED_EDGE('',*,*,#10516,.F.);
#14199=ORIENTED_EDGE('',*,*,#10517,.F.);
#14200=ORIENTED_EDGE('',*,*,#10518,.F.);
#14201=ORIENTED_EDGE('',*,*,#10469,.T.);
#14202=ORIENTED_EDGE('',*,*,#10519,.F.);
#14203=ORIENTED_EDGE('',*,*,#10497,.T.);
#14204=ORIENTED_EDGE('',*,*,#10520,.F.);
#14205=ORIENTED_EDGE('',*,*,#10521,.F.);
#14206=ORIENTED_EDGE('',*,*,#10522,.F.);
#14207=ORIENTED_EDGE('',*,*,#10523,.F.);
#14208=ORIENTED_EDGE('',*,*,#10524,.F.);
#14209=ORIENTED_EDGE('',*,*,#10499,.T.);
#14210=ORIENTED_EDGE('',*,*,#10525,.F.);
#14211=ORIENTED_EDGE('',*,*,#10503,.T.);
#14212=ORIENTED_EDGE('',*,*,#10526,.F.);
#14213=ORIENTED_EDGE('',*,*,#10527,.F.);
#14214=ORIENTED_EDGE('',*,*,#10528,.F.);
#14215=ORIENTED_EDGE('',*,*,#10506,.T.);
#14216=ORIENTED_EDGE('',*,*,#10529,.F.);
#14217=ORIENTED_EDGE('',*,*,#10530,.F.);
#14218=ORIENTED_EDGE('',*,*,#10531,.F.);
#14219=ORIENTED_EDGE('',*,*,#10509,.T.);
#14220=ORIENTED_EDGE('',*,*,#10532,.F.);
#14221=ORIENTED_EDGE('',*,*,#10533,.F.);
#14222=ORIENTED_EDGE('',*,*,#10534,.F.);
#14223=ORIENTED_EDGE('',*,*,#10512,.T.);
#14224=ORIENTED_EDGE('',*,*,#10535,.F.);
#14225=ORIENTED_EDGE('',*,*,#10536,.F.);
#14226=ORIENTED_EDGE('',*,*,#10537,.F.);
#14227=ORIENTED_EDGE('',*,*,#10515,.T.);
#14228=ORIENTED_EDGE('',*,*,#10538,.F.);
#14229=ORIENTED_EDGE('',*,*,#10539,.F.);
#14230=ORIENTED_EDGE('',*,*,#10540,.F.);
#14231=ORIENTED_EDGE('',*,*,#10541,.F.);
#14232=ORIENTED_EDGE('',*,*,#10542,.F.);
#14233=ORIENTED_EDGE('',*,*,#10517,.T.);
#14234=ORIENTED_EDGE('',*,*,#10543,.F.);
#14235=ORIENTED_EDGE('',*,*,#10521,.T.);
#14236=ORIENTED_EDGE('',*,*,#10544,.F.);
#14237=ORIENTED_EDGE('',*,*,#10450,.F.);
#14238=ORIENTED_EDGE('',*,*,#10545,.F.);
#14239=ORIENTED_EDGE('',*,*,#10446,.F.);
#14240=ORIENTED_EDGE('',*,*,#10546,.F.);
#14241=ORIENTED_EDGE('',*,*,#10523,.T.);
#14242=ORIENTED_EDGE('',*,*,#10547,.F.);
#14243=ORIENTED_EDGE('',*,*,#10527,.T.);
#14244=ORIENTED_EDGE('',*,*,#10548,.F.);
#14245=ORIENTED_EDGE('',*,*,#10452,.F.);
#14246=ORIENTED_EDGE('',*,*,#10549,.F.);
#14247=ORIENTED_EDGE('',*,*,#10530,.T.);
#14248=ORIENTED_EDGE('',*,*,#10550,.F.);
#14249=ORIENTED_EDGE('',*,*,#10454,.F.);
#14250=ORIENTED_EDGE('',*,*,#10551,.F.);
#14251=ORIENTED_EDGE('',*,*,#10533,.T.);
#14252=ORIENTED_EDGE('',*,*,#10552,.F.);
#14253=ORIENTED_EDGE('',*,*,#10456,.F.);
#14254=ORIENTED_EDGE('',*,*,#10553,.F.);
#14255=ORIENTED_EDGE('',*,*,#10536,.T.);
#14256=ORIENTED_EDGE('',*,*,#10554,.F.);
#14257=ORIENTED_EDGE('',*,*,#10440,.F.);
#14258=ORIENTED_EDGE('',*,*,#10555,.F.);
#14259=ORIENTED_EDGE('',*,*,#10539,.T.);
#14260=ORIENTED_EDGE('',*,*,#10556,.F.);
#14261=ORIENTED_EDGE('',*,*,#10442,.F.);
#14262=ORIENTED_EDGE('',*,*,#10557,.F.);
#14263=ORIENTED_EDGE('',*,*,#10444,.F.);
#14264=ORIENTED_EDGE('',*,*,#10558,.F.);
#14265=ORIENTED_EDGE('',*,*,#10541,.T.);
#14266=ORIENTED_EDGE('',*,*,#10559,.F.);
#14267=ORIENTED_EDGE('',*,*,#10436,.T.);
#14268=ORIENTED_EDGE('',*,*,#10432,.F.);
#14269=ORIENTED_EDGE('',*,*,#10460,.F.);
#14270=ORIENTED_EDGE('',*,*,#10431,.T.);
#14271=ORIENTED_EDGE('',*,*,#10560,.T.);
#14272=ORIENTED_EDGE('',*,*,#10470,.T.);
#14273=ORIENTED_EDGE('',*,*,#10518,.T.);
#14274=ORIENTED_EDGE('',*,*,#10542,.T.);
#14275=ORIENTED_EDGE('',*,*,#10558,.T.);
#14276=ORIENTED_EDGE('',*,*,#10514,.T.);
#14277=ORIENTED_EDGE('',*,*,#10472,.T.);
#14278=ORIENTED_EDGE('',*,*,#10561,.T.);
#14279=ORIENTED_EDGE('',*,*,#10556,.T.);
#14280=ORIENTED_EDGE('',*,*,#10538,.T.);
#14281=ORIENTED_EDGE('',*,*,#10471,.F.);
#14282=ORIENTED_EDGE('',*,*,#10560,.F.);
#14283=ORIENTED_EDGE('',*,*,#10443,.F.);
#14284=ORIENTED_EDGE('',*,*,#10561,.F.);
#14285=ORIENTED_EDGE('',*,*,#10562,.T.);
#14286=ORIENTED_EDGE('',*,*,#10466,.T.);
#14287=ORIENTED_EDGE('',*,*,#10500,.T.);
#14288=ORIENTED_EDGE('',*,*,#10524,.T.);
#14289=ORIENTED_EDGE('',*,*,#10546,.T.);
#14290=ORIENTED_EDGE('',*,*,#10519,.T.);
#14291=ORIENTED_EDGE('',*,*,#10468,.T.);
#14292=ORIENTED_EDGE('',*,*,#10563,.T.);
#14293=ORIENTED_EDGE('',*,*,#10559,.T.);
#14294=ORIENTED_EDGE('',*,*,#10543,.T.);
#14295=ORIENTED_EDGE('',*,*,#10467,.F.);
#14296=ORIENTED_EDGE('',*,*,#10562,.F.);
#14297=ORIENTED_EDGE('',*,*,#10445,.F.);
#14298=ORIENTED_EDGE('',*,*,#10563,.F.);
#14299=ORIENTED_EDGE('',*,*,#10564,.T.);
#14300=ORIENTED_EDGE('',*,*,#10474,.T.);
#14301=ORIENTED_EDGE('',*,*,#10516,.T.);
#14302=ORIENTED_EDGE('',*,*,#10540,.T.);
#14303=ORIENTED_EDGE('',*,*,#10557,.T.);
#14304=ORIENTED_EDGE('',*,*,#10511,.T.);
#14305=ORIENTED_EDGE('',*,*,#10476,.T.);
#14306=ORIENTED_EDGE('',*,*,#10565,.T.);
#14307=ORIENTED_EDGE('',*,*,#10554,.T.);
#14308=ORIENTED_EDGE('',*,*,#10535,.T.);
#14309=ORIENTED_EDGE('',*,*,#10475,.F.);
#14310=ORIENTED_EDGE('',*,*,#10564,.F.);
#14311=ORIENTED_EDGE('',*,*,#10441,.F.);
#14312=ORIENTED_EDGE('',*,*,#10565,.F.);
#14313=ORIENTED_EDGE('',*,*,#10566,.T.);
#14314=ORIENTED_EDGE('',*,*,#10478,.T.);
#14315=ORIENTED_EDGE('',*,*,#10513,.T.);
#14316=ORIENTED_EDGE('',*,*,#10537,.T.);
#14317=ORIENTED_EDGE('',*,*,#10555,.T.);
#14318=ORIENTED_EDGE('',*,*,#10508,.T.);
#14319=ORIENTED_EDGE('',*,*,#10480,.T.);
#14320=ORIENTED_EDGE('',*,*,#10567,.T.);
#14321=ORIENTED_EDGE('',*,*,#10552,.T.);
#14322=ORIENTED_EDGE('',*,*,#10532,.T.);
#14323=ORIENTED_EDGE('',*,*,#10479,.F.);
#14324=ORIENTED_EDGE('',*,*,#10566,.F.);
#14325=ORIENTED_EDGE('',*,*,#10439,.F.);
#14326=ORIENTED_EDGE('',*,*,#10567,.F.);
#14327=ORIENTED_EDGE('',*,*,#10568,.T.);
#14328=ORIENTED_EDGE('',*,*,#10482,.T.);
#14329=ORIENTED_EDGE('',*,*,#10510,.T.);
#14330=ORIENTED_EDGE('',*,*,#10534,.T.);
#14331=ORIENTED_EDGE('',*,*,#10553,.T.);
#14332=ORIENTED_EDGE('',*,*,#10505,.T.);
#14333=ORIENTED_EDGE('',*,*,#10484,.T.);
#14334=ORIENTED_EDGE('',*,*,#10569,.T.);
#14335=ORIENTED_EDGE('',*,*,#10550,.T.);
#14336=ORIENTED_EDGE('',*,*,#10529,.T.);
#14337=ORIENTED_EDGE('',*,*,#10483,.F.);
#14338=ORIENTED_EDGE('',*,*,#10568,.F.);
#14339=ORIENTED_EDGE('',*,*,#10455,.F.);
#14340=ORIENTED_EDGE('',*,*,#10569,.F.);
#14341=ORIENTED_EDGE('',*,*,#10570,.T.);
#14342=ORIENTED_EDGE('',*,*,#10486,.T.);
#14343=ORIENTED_EDGE('',*,*,#10507,.T.);
#14344=ORIENTED_EDGE('',*,*,#10531,.T.);
#14345=ORIENTED_EDGE('',*,*,#10551,.T.);
#14346=ORIENTED_EDGE('',*,*,#10502,.T.);
#14347=ORIENTED_EDGE('',*,*,#10488,.T.);
#14348=ORIENTED_EDGE('',*,*,#10571,.T.);
#14349=ORIENTED_EDGE('',*,*,#10548,.T.);
#14350=ORIENTED_EDGE('',*,*,#10526,.T.);
#14351=ORIENTED_EDGE('',*,*,#10487,.F.);
#14352=ORIENTED_EDGE('',*,*,#10570,.F.);
#14353=ORIENTED_EDGE('',*,*,#10453,.F.);
#14354=ORIENTED_EDGE('',*,*,#10571,.F.);
#14355=ORIENTED_EDGE('',*,*,#10572,.T.);
#14356=ORIENTED_EDGE('',*,*,#10490,.T.);
#14357=ORIENTED_EDGE('',*,*,#10504,.T.);
#14358=ORIENTED_EDGE('',*,*,#10528,.T.);
#14359=ORIENTED_EDGE('',*,*,#10549,.T.);
#14360=ORIENTED_EDGE('',*,*,#10496,.T.);
#14361=ORIENTED_EDGE('',*,*,#10492,.T.);
#14362=ORIENTED_EDGE('',*,*,#10573,.T.);
#14363=ORIENTED_EDGE('',*,*,#10544,.T.);
#14364=ORIENTED_EDGE('',*,*,#10520,.T.);
#14365=ORIENTED_EDGE('',*,*,#10491,.F.);
#14366=ORIENTED_EDGE('',*,*,#10572,.F.);
#14367=ORIENTED_EDGE('',*,*,#10451,.F.);
#14368=ORIENTED_EDGE('',*,*,#10573,.F.);
#14369=ORIENTED_EDGE('',*,*,#10574,.T.);
#14370=ORIENTED_EDGE('',*,*,#10494,.T.);
#14371=ORIENTED_EDGE('',*,*,#10498,.T.);
#14372=ORIENTED_EDGE('',*,*,#10522,.T.);
#14373=ORIENTED_EDGE('',*,*,#10545,.T.);
#14374=ORIENTED_EDGE('',*,*,#10501,.T.);
#14375=ORIENTED_EDGE('',*,*,#10464,.T.);
#14376=ORIENTED_EDGE('',*,*,#10575,.T.);
#14377=ORIENTED_EDGE('',*,*,#10547,.T.);
#14378=ORIENTED_EDGE('',*,*,#10525,.T.);
#14379=ORIENTED_EDGE('',*,*,#10495,.F.);
#14380=ORIENTED_EDGE('',*,*,#10574,.F.);
#14381=ORIENTED_EDGE('',*,*,#10449,.F.);
#14382=ORIENTED_EDGE('',*,*,#10447,.F.);
#14383=ORIENTED_EDGE('',*,*,#10575,.F.);
#14384=ORIENTED_EDGE('',*,*,#10463,.F.);
#14385=ORIENTED_EDGE('',*,*,#10576,.T.);
#14386=ORIENTED_EDGE('',*,*,#10576,.F.);
#14387=ORIENTED_EDGE('',*,*,#10577,.T.);
#14388=ORIENTED_EDGE('',*,*,#10578,.T.);
#14389=ORIENTED_EDGE('',*,*,#10579,.T.);
#14390=ORIENTED_EDGE('',*,*,#10578,.F.);
#14391=ORIENTED_EDGE('',*,*,#10580,.F.);
#14392=ORIENTED_EDGE('',*,*,#10581,.T.);
#14393=ORIENTED_EDGE('',*,*,#10582,.T.);
#14394=ORIENTED_EDGE('',*,*,#10583,.T.);
#14395=ORIENTED_EDGE('',*,*,#10581,.F.);
#14396=ORIENTED_EDGE('',*,*,#10584,.T.);
#14397=ORIENTED_EDGE('',*,*,#10585,.T.);
#14398=ORIENTED_EDGE('',*,*,#10582,.F.);
#14399=ORIENTED_EDGE('',*,*,#10583,.F.);
#14400=ORIENTED_EDGE('',*,*,#10585,.F.);
#14401=ORIENTED_EDGE('',*,*,#10586,.T.);
#14402=ORIENTED_EDGE('',*,*,#10584,.F.);
#14403=ORIENTED_EDGE('',*,*,#10587,.T.);
#14404=ORIENTED_EDGE('',*,*,#10588,.T.);
#14405=ORIENTED_EDGE('',*,*,#10587,.F.);
#14406=ORIENTED_EDGE('',*,*,#10586,.F.);
#14407=ORIENTED_EDGE('',*,*,#10588,.F.);
#14408=ORIENTED_EDGE('',*,*,#10589,.T.);
#14409=ORIENTED_EDGE('',*,*,#10590,.T.);
#14410=ORIENTED_EDGE('',*,*,#10589,.F.);
#14411=ORIENTED_EDGE('',*,*,#10590,.F.);
#14412=ORIENTED_EDGE('',*,*,#10591,.T.);
#14413=ORIENTED_EDGE('',*,*,#10592,.T.);
#14414=ORIENTED_EDGE('',*,*,#10591,.F.);
#14415=ORIENTED_EDGE('',*,*,#10593,.F.);
#14416=ORIENTED_EDGE('',*,*,#10594,.T.);
#14417=ORIENTED_EDGE('',*,*,#10595,.T.);
#14418=ORIENTED_EDGE('',*,*,#10594,.F.);
#14419=ORIENTED_EDGE('',*,*,#10596,.F.);
#14420=ORIENTED_EDGE('',*,*,#10597,.T.);
#14421=ORIENTED_EDGE('',*,*,#10598,.T.);
#14422=ORIENTED_EDGE('',*,*,#10597,.F.);
#14423=ORIENTED_EDGE('',*,*,#10579,.F.);
#14424=ORIENTED_EDGE('',*,*,#10599,.T.);
#14425=ORIENTED_EDGE('',*,*,#10596,.T.);
#14426=ORIENTED_EDGE('',*,*,#10599,.F.);
#14427=ORIENTED_EDGE('',*,*,#10595,.F.);
#14428=ORIENTED_EDGE('',*,*,#10600,.T.);
#14429=ORIENTED_EDGE('',*,*,#10577,.F.);
#14430=ORIENTED_EDGE('',*,*,#10600,.F.);
#14431=ORIENTED_EDGE('',*,*,#10593,.T.);
#14432=ORIENTED_EDGE('',*,*,#10592,.F.);
#14433=ORIENTED_EDGE('',*,*,#10598,.F.);
#14434=ORIENTED_EDGE('',*,*,#10580,.T.);
#14435=ORIENTED_EDGE('',*,*,#10601,.T.);
#14436=ORIENTED_EDGE('',*,*,#10602,.T.);
#14437=ORIENTED_EDGE('',*,*,#10603,.T.);
#14438=ORIENTED_EDGE('',*,*,#10602,.F.);
#14439=ORIENTED_EDGE('',*,*,#10604,.F.);
#14440=ORIENTED_EDGE('',*,*,#10605,.T.);
#14441=ORIENTED_EDGE('',*,*,#10606,.T.);
#14442=ORIENTED_EDGE('',*,*,#10605,.F.);
#14443=ORIENTED_EDGE('',*,*,#10606,.F.);
#14444=ORIENTED_EDGE('',*,*,#10607,.T.);
#14445=ORIENTED_EDGE('',*,*,#10608,.T.);
#14446=ORIENTED_EDGE('',*,*,#10607,.F.);
#14447=ORIENTED_EDGE('',*,*,#10608,.F.);
#14448=ORIENTED_EDGE('',*,*,#10609,.T.);
#14449=ORIENTED_EDGE('',*,*,#10610,.T.);
#14450=ORIENTED_EDGE('',*,*,#10609,.F.);
#14451=ORIENTED_EDGE('',*,*,#10611,.T.);
#14452=ORIENTED_EDGE('',*,*,#10612,.T.);
#14453=ORIENTED_EDGE('',*,*,#10613,.F.);
#14454=ORIENTED_EDGE('',*,*,#10612,.F.);
#14455=ORIENTED_EDGE('',*,*,#10614,.T.);
#14456=ORIENTED_EDGE('',*,*,#10611,.F.);
#14457=ORIENTED_EDGE('',*,*,#10615,.T.);
#14458=ORIENTED_EDGE('',*,*,#10604,.T.);
#14459=ORIENTED_EDGE('',*,*,#10615,.F.);
#14460=ORIENTED_EDGE('',*,*,#10614,.F.);
#14461=ORIENTED_EDGE('',*,*,#10616,.F.);
#14462=ORIENTED_EDGE('',*,*,#10617,.T.);
#14463=ORIENTED_EDGE('',*,*,#10601,.F.);
#14464=ORIENTED_EDGE('',*,*,#10617,.F.);
#14465=ORIENTED_EDGE('',*,*,#10603,.F.);
#14466=ORIENTED_EDGE('',*,*,#10618,.T.);
#14467=ORIENTED_EDGE('',*,*,#10619,.T.);
#14468=ORIENTED_EDGE('',*,*,#10618,.F.);
#14469=ORIENTED_EDGE('',*,*,#10613,.T.);
#14470=ORIENTED_EDGE('',*,*,#10619,.F.);
#14471=ORIENTED_EDGE('',*,*,#10610,.F.);
#14472=ORIENTED_EDGE('',*,*,#10616,.T.);
#14473=ORIENTED_EDGE('',*,*,#10620,.T.);
#14474=ORIENTED_EDGE('',*,*,#10620,.F.);
#14475=ORIENTED_EDGE('',*,*,#10621,.T.);
#14476=ORIENTED_EDGE('',*,*,#10621,.F.);
#14477=ORIENTED_EDGE('',*,*,#10622,.T.);
#14478=ORIENTED_EDGE('',*,*,#10622,.F.);
#14479=ORIENTED_EDGE('',*,*,#10623,.T.);
#14480=ORIENTED_EDGE('',*,*,#10623,.F.);
#14481=ORIENTED_EDGE('',*,*,#10624,.T.);
#14482=ORIENTED_EDGE('',*,*,#10624,.F.);
#14483=ORIENTED_EDGE('',*,*,#10625,.T.);
#14484=ORIENTED_EDGE('',*,*,#10625,.F.);
#14485=ORIENTED_EDGE('',*,*,#10626,.T.);
#14486=ORIENTED_EDGE('',*,*,#10626,.F.);
#14487=ORIENTED_EDGE('',*,*,#10627,.F.);
#14488=ORIENTED_EDGE('',*,*,#10628,.F.);
#14489=ORIENTED_EDGE('',*,*,#10629,.T.);
#14490=ORIENTED_EDGE('',*,*,#10630,.F.);
#14491=ORIENTED_EDGE('',*,*,#10631,.F.);
#14492=ORIENTED_EDGE('',*,*,#10629,.F.);
#14493=ORIENTED_EDGE('',*,*,#10632,.F.);
#14494=ORIENTED_EDGE('',*,*,#10633,.T.);
#14495=ORIENTED_EDGE('',*,*,#10634,.T.);
#14496=ORIENTED_EDGE('',*,*,#10633,.F.);
#14497=ORIENTED_EDGE('',*,*,#10635,.F.);
#14498=ORIENTED_EDGE('',*,*,#10636,.T.);
#14499=ORIENTED_EDGE('',*,*,#10632,.T.);
#14500=ORIENTED_EDGE('',*,*,#10636,.F.);
#14501=ORIENTED_EDGE('',*,*,#10637,.F.);
#14502=ORIENTED_EDGE('',*,*,#10638,.T.);
#14503=ORIENTED_EDGE('',*,*,#10639,.T.);
#14504=ORIENTED_EDGE('',*,*,#10638,.F.);
#14505=ORIENTED_EDGE('',*,*,#10640,.F.);
#14506=ORIENTED_EDGE('',*,*,#10641,.T.);
#14507=ORIENTED_EDGE('',*,*,#10637,.T.);
#14508=ORIENTED_EDGE('',*,*,#10641,.F.);
#14509=ORIENTED_EDGE('',*,*,#10642,.F.);
#14510=ORIENTED_EDGE('',*,*,#10643,.F.);
#14511=ORIENTED_EDGE('',*,*,#10644,.F.);
#14512=ORIENTED_EDGE('',*,*,#10645,.F.);
#14513=ORIENTED_EDGE('',*,*,#10646,.F.);
#14514=ORIENTED_EDGE('',*,*,#10647,.F.);
#14515=ORIENTED_EDGE('',*,*,#10648,.F.);
#14516=ORIENTED_EDGE('',*,*,#10649,.F.);
#14517=ORIENTED_EDGE('',*,*,#10650,.F.);
#14518=ORIENTED_EDGE('',*,*,#10651,.T.);
#14519=ORIENTED_EDGE('',*,*,#10640,.T.);
#14520=ORIENTED_EDGE('',*,*,#10651,.F.);
#14521=ORIENTED_EDGE('',*,*,#10652,.F.);
#14522=ORIENTED_EDGE('',*,*,#10653,.F.);
#14523=ORIENTED_EDGE('',*,*,#10654,.F.);
#14524=ORIENTED_EDGE('',*,*,#10655,.F.);
#14525=ORIENTED_EDGE('',*,*,#10656,.F.);
#14526=ORIENTED_EDGE('',*,*,#10657,.F.);
#14527=ORIENTED_EDGE('',*,*,#10658,.F.);
#14528=ORIENTED_EDGE('',*,*,#10659,.F.);
#14529=ORIENTED_EDGE('',*,*,#10660,.F.);
#14530=ORIENTED_EDGE('',*,*,#10661,.T.);
#14531=ORIENTED_EDGE('',*,*,#10662,.T.);
#14532=ORIENTED_EDGE('',*,*,#10661,.F.);
#14533=ORIENTED_EDGE('',*,*,#10662,.F.);
#14534=ORIENTED_EDGE('',*,*,#10663,.T.);
#14535=ORIENTED_EDGE('',*,*,#10630,.T.);
#14536=ORIENTED_EDGE('',*,*,#10631,.T.);
#14537=ORIENTED_EDGE('',*,*,#10663,.F.);
#14538=ORIENTED_EDGE('',*,*,#10627,.T.);
#14539=ORIENTED_EDGE('',*,*,#10628,.T.);
#14540=ORIENTED_EDGE('',*,*,#10664,.T.);
#14541=ORIENTED_EDGE('',*,*,#10665,.F.);
#14542=ORIENTED_EDGE('',*,*,#10666,.T.);
#14543=ORIENTED_EDGE('',*,*,#10667,.T.);
#14544=ORIENTED_EDGE('',*,*,#10668,.T.);
#14545=ORIENTED_EDGE('',*,*,#10669,.F.);
#14546=ORIENTED_EDGE('',*,*,#10670,.T.);
#14547=ORIENTED_EDGE('',*,*,#10671,.T.);
#14548=ORIENTED_EDGE('',*,*,#10672,.T.);
#14549=ORIENTED_EDGE('',*,*,#10673,.F.);
#14550=ORIENTED_EDGE('',*,*,#10674,.T.);
#14551=ORIENTED_EDGE('',*,*,#10675,.T.);
#14552=ORIENTED_EDGE('',*,*,#10676,.T.);
#14553=ORIENTED_EDGE('',*,*,#10677,.F.);
#14554=ORIENTED_EDGE('',*,*,#10678,.T.);
#14555=ORIENTED_EDGE('',*,*,#10679,.T.);
#14556=ORIENTED_EDGE('',*,*,#10680,.T.);
#14557=ORIENTED_EDGE('',*,*,#10681,.F.);
#14558=ORIENTED_EDGE('',*,*,#10682,.T.);
#14559=ORIENTED_EDGE('',*,*,#10683,.T.);
#14560=ORIENTED_EDGE('',*,*,#10684,.T.);
#14561=ORIENTED_EDGE('',*,*,#10685,.F.);
#14562=ORIENTED_EDGE('',*,*,#10686,.T.);
#14563=ORIENTED_EDGE('',*,*,#10687,.T.);
#14564=ORIENTED_EDGE('',*,*,#10688,.T.);
#14565=ORIENTED_EDGE('',*,*,#10689,.F.);
#14566=ORIENTED_EDGE('',*,*,#10690,.T.);
#14567=ORIENTED_EDGE('',*,*,#10691,.T.);
#14568=ORIENTED_EDGE('',*,*,#10692,.T.);
#14569=ORIENTED_EDGE('',*,*,#10693,.F.);
#14570=ORIENTED_EDGE('',*,*,#10694,.T.);
#14571=ORIENTED_EDGE('',*,*,#10695,.T.);
#14572=ORIENTED_EDGE('',*,*,#10696,.T.);
#14573=ORIENTED_EDGE('',*,*,#10697,.F.);
#14574=ORIENTED_EDGE('',*,*,#10664,.F.);
#14575=ORIENTED_EDGE('',*,*,#10667,.F.);
#14576=ORIENTED_EDGE('',*,*,#10698,.T.);
#14577=ORIENTED_EDGE('',*,*,#10699,.T.);
#14578=ORIENTED_EDGE('',*,*,#10700,.T.);
#14579=ORIENTED_EDGE('',*,*,#10701,.T.);
#14580=ORIENTED_EDGE('',*,*,#10702,.T.);
#14581=ORIENTED_EDGE('',*,*,#10695,.F.);
#14582=ORIENTED_EDGE('',*,*,#10703,.T.);
#14583=ORIENTED_EDGE('',*,*,#10671,.F.);
#14584=ORIENTED_EDGE('',*,*,#10704,.T.);
#14585=ORIENTED_EDGE('',*,*,#10705,.T.);
#14586=ORIENTED_EDGE('',*,*,#10706,.T.);
#14587=ORIENTED_EDGE('',*,*,#10675,.F.);
#14588=ORIENTED_EDGE('',*,*,#10707,.T.);
#14589=ORIENTED_EDGE('',*,*,#10708,.T.);
#14590=ORIENTED_EDGE('',*,*,#10709,.T.);
#14591=ORIENTED_EDGE('',*,*,#10679,.F.);
#14592=ORIENTED_EDGE('',*,*,#10710,.T.);
#14593=ORIENTED_EDGE('',*,*,#10711,.T.);
#14594=ORIENTED_EDGE('',*,*,#10712,.T.);
#14595=ORIENTED_EDGE('',*,*,#10683,.F.);
#14596=ORIENTED_EDGE('',*,*,#10713,.T.);
#14597=ORIENTED_EDGE('',*,*,#10714,.T.);
#14598=ORIENTED_EDGE('',*,*,#10715,.T.);
#14599=ORIENTED_EDGE('',*,*,#10687,.F.);
#14600=ORIENTED_EDGE('',*,*,#10716,.T.);
#14601=ORIENTED_EDGE('',*,*,#10717,.T.);
#14602=ORIENTED_EDGE('',*,*,#10718,.T.);
#14603=ORIENTED_EDGE('',*,*,#10719,.T.);
#14604=ORIENTED_EDGE('',*,*,#10720,.T.);
#14605=ORIENTED_EDGE('',*,*,#10691,.F.);
#14606=ORIENTED_EDGE('',*,*,#10721,.T.);
#14607=ORIENTED_EDGE('',*,*,#10699,.F.);
#14608=ORIENTED_EDGE('',*,*,#10722,.T.);
#14609=ORIENTED_EDGE('',*,*,#10723,.T.);
#14610=ORIENTED_EDGE('',*,*,#10724,.T.);
#14611=ORIENTED_EDGE('',*,*,#10725,.T.);
#14612=ORIENTED_EDGE('',*,*,#10726,.T.);
#14613=ORIENTED_EDGE('',*,*,#10701,.F.);
#14614=ORIENTED_EDGE('',*,*,#10727,.T.);
#14615=ORIENTED_EDGE('',*,*,#10705,.F.);
#14616=ORIENTED_EDGE('',*,*,#10728,.T.);
#14617=ORIENTED_EDGE('',*,*,#10729,.T.);
#14618=ORIENTED_EDGE('',*,*,#10730,.T.);
#14619=ORIENTED_EDGE('',*,*,#10708,.F.);
#14620=ORIENTED_EDGE('',*,*,#10731,.T.);
#14621=ORIENTED_EDGE('',*,*,#10732,.T.);
#14622=ORIENTED_EDGE('',*,*,#10733,.T.);
#14623=ORIENTED_EDGE('',*,*,#10711,.F.);
#14624=ORIENTED_EDGE('',*,*,#10734,.T.);
#14625=ORIENTED_EDGE('',*,*,#10735,.T.);
#14626=ORIENTED_EDGE('',*,*,#10736,.T.);
#14627=ORIENTED_EDGE('',*,*,#10714,.F.);
#14628=ORIENTED_EDGE('',*,*,#10737,.T.);
#14629=ORIENTED_EDGE('',*,*,#10738,.T.);
#14630=ORIENTED_EDGE('',*,*,#10739,.T.);
#14631=ORIENTED_EDGE('',*,*,#10717,.F.);
#14632=ORIENTED_EDGE('',*,*,#10740,.T.);
#14633=ORIENTED_EDGE('',*,*,#10741,.T.);
#14634=ORIENTED_EDGE('',*,*,#10742,.T.);
#14635=ORIENTED_EDGE('',*,*,#10743,.T.);
#14636=ORIENTED_EDGE('',*,*,#10744,.T.);
#14637=ORIENTED_EDGE('',*,*,#10719,.F.);
#14638=ORIENTED_EDGE('',*,*,#10745,.T.);
#14639=ORIENTED_EDGE('',*,*,#10723,.F.);
#14640=ORIENTED_EDGE('',*,*,#10746,.T.);
#14641=ORIENTED_EDGE('',*,*,#10649,.T.);
#14642=ORIENTED_EDGE('',*,*,#10747,.T.);
#14643=ORIENTED_EDGE('',*,*,#10653,.T.);
#14644=ORIENTED_EDGE('',*,*,#10748,.T.);
#14645=ORIENTED_EDGE('',*,*,#10725,.F.);
#14646=ORIENTED_EDGE('',*,*,#10749,.T.);
#14647=ORIENTED_EDGE('',*,*,#10729,.F.);
#14648=ORIENTED_EDGE('',*,*,#10750,.T.);
#14649=ORIENTED_EDGE('',*,*,#10647,.T.);
#14650=ORIENTED_EDGE('',*,*,#10751,.T.);
#14651=ORIENTED_EDGE('',*,*,#10732,.F.);
#14652=ORIENTED_EDGE('',*,*,#10752,.T.);
#14653=ORIENTED_EDGE('',*,*,#10645,.T.);
#14654=ORIENTED_EDGE('',*,*,#10753,.T.);
#14655=ORIENTED_EDGE('',*,*,#10735,.F.);
#14656=ORIENTED_EDGE('',*,*,#10754,.T.);
#14657=ORIENTED_EDGE('',*,*,#10643,.T.);
#14658=ORIENTED_EDGE('',*,*,#10755,.T.);
#14659=ORIENTED_EDGE('',*,*,#10738,.F.);
#14660=ORIENTED_EDGE('',*,*,#10756,.T.);
#14661=ORIENTED_EDGE('',*,*,#10659,.T.);
#14662=ORIENTED_EDGE('',*,*,#10757,.T.);
#14663=ORIENTED_EDGE('',*,*,#10741,.F.);
#14664=ORIENTED_EDGE('',*,*,#10758,.T.);
#14665=ORIENTED_EDGE('',*,*,#10657,.T.);
#14666=ORIENTED_EDGE('',*,*,#10759,.T.);
#14667=ORIENTED_EDGE('',*,*,#10655,.T.);
#14668=ORIENTED_EDGE('',*,*,#10760,.T.);
#14669=ORIENTED_EDGE('',*,*,#10743,.F.);
#14670=ORIENTED_EDGE('',*,*,#10761,.T.);
#14671=ORIENTED_EDGE('',*,*,#10639,.F.);
#14672=ORIENTED_EDGE('',*,*,#10635,.T.);
#14673=ORIENTED_EDGE('',*,*,#10660,.T.);
#14674=ORIENTED_EDGE('',*,*,#10634,.F.);
#14675=ORIENTED_EDGE('',*,*,#10762,.F.);
#14676=ORIENTED_EDGE('',*,*,#10761,.F.);
#14677=ORIENTED_EDGE('',*,*,#10745,.F.);
#14678=ORIENTED_EDGE('',*,*,#10721,.F.);
#14679=ORIENTED_EDGE('',*,*,#10690,.F.);
#14680=ORIENTED_EDGE('',*,*,#10718,.F.);
#14681=ORIENTED_EDGE('',*,*,#10742,.F.);
#14682=ORIENTED_EDGE('',*,*,#10759,.F.);
#14683=ORIENTED_EDGE('',*,*,#10763,.F.);
#14684=ORIENTED_EDGE('',*,*,#10688,.F.);
#14685=ORIENTED_EDGE('',*,*,#10689,.T.);
#14686=ORIENTED_EDGE('',*,*,#10763,.T.);
#14687=ORIENTED_EDGE('',*,*,#10656,.T.);
#14688=ORIENTED_EDGE('',*,*,#10762,.T.);
#14689=ORIENTED_EDGE('',*,*,#10764,.F.);
#14690=ORIENTED_EDGE('',*,*,#10749,.F.);
#14691=ORIENTED_EDGE('',*,*,#10727,.F.);
#14692=ORIENTED_EDGE('',*,*,#10703,.F.);
#14693=ORIENTED_EDGE('',*,*,#10694,.F.);
#14694=ORIENTED_EDGE('',*,*,#10720,.F.);
#14695=ORIENTED_EDGE('',*,*,#10744,.F.);
#14696=ORIENTED_EDGE('',*,*,#10760,.F.);
#14697=ORIENTED_EDGE('',*,*,#10765,.F.);
#14698=ORIENTED_EDGE('',*,*,#10692,.F.);
#14699=ORIENTED_EDGE('',*,*,#10693,.T.);
#14700=ORIENTED_EDGE('',*,*,#10765,.T.);
#14701=ORIENTED_EDGE('',*,*,#10654,.T.);
#14702=ORIENTED_EDGE('',*,*,#10764,.T.);
#14703=ORIENTED_EDGE('',*,*,#10766,.F.);
#14704=ORIENTED_EDGE('',*,*,#10758,.F.);
#14705=ORIENTED_EDGE('',*,*,#10740,.F.);
#14706=ORIENTED_EDGE('',*,*,#10716,.F.);
#14707=ORIENTED_EDGE('',*,*,#10686,.F.);
#14708=ORIENTED_EDGE('',*,*,#10715,.F.);
#14709=ORIENTED_EDGE('',*,*,#10739,.F.);
#14710=ORIENTED_EDGE('',*,*,#10757,.F.);
#14711=ORIENTED_EDGE('',*,*,#10767,.F.);
#14712=ORIENTED_EDGE('',*,*,#10684,.F.);
#14713=ORIENTED_EDGE('',*,*,#10685,.T.);
#14714=ORIENTED_EDGE('',*,*,#10767,.T.);
#14715=ORIENTED_EDGE('',*,*,#10658,.T.);
#14716=ORIENTED_EDGE('',*,*,#10766,.T.);
#14717=ORIENTED_EDGE('',*,*,#10768,.F.);
#14718=ORIENTED_EDGE('',*,*,#10756,.F.);
#14719=ORIENTED_EDGE('',*,*,#10737,.F.);
#14720=ORIENTED_EDGE('',*,*,#10713,.F.);
#14721=ORIENTED_EDGE('',*,*,#10682,.F.);
#14722=ORIENTED_EDGE('',*,*,#10712,.F.);
#14723=ORIENTED_EDGE('',*,*,#10736,.F.);
#14724=ORIENTED_EDGE('',*,*,#10755,.F.);
#14725=ORIENTED_EDGE('',*,*,#10769,.F.);
#14726=ORIENTED_EDGE('',*,*,#10680,.F.);
#14727=ORIENTED_EDGE('',*,*,#10681,.T.);
#14728=ORIENTED_EDGE('',*,*,#10769,.T.);
#14729=ORIENTED_EDGE('',*,*,#10642,.T.);
#14730=ORIENTED_EDGE('',*,*,#10768,.T.);
#14731=ORIENTED_EDGE('',*,*,#10770,.F.);
#14732=ORIENTED_EDGE('',*,*,#10754,.F.);
#14733=ORIENTED_EDGE('',*,*,#10734,.F.);
#14734=ORIENTED_EDGE('',*,*,#10710,.F.);
#14735=ORIENTED_EDGE('',*,*,#10678,.F.);
#14736=ORIENTED_EDGE('',*,*,#10709,.F.);
#14737=ORIENTED_EDGE('',*,*,#10733,.F.);
#14738=ORIENTED_EDGE('',*,*,#10753,.F.);
#14739=ORIENTED_EDGE('',*,*,#10771,.F.);
#14740=ORIENTED_EDGE('',*,*,#10676,.F.);
#14741=ORIENTED_EDGE('',*,*,#10677,.T.);
#14742=ORIENTED_EDGE('',*,*,#10771,.T.);
#14743=ORIENTED_EDGE('',*,*,#10644,.T.);
#14744=ORIENTED_EDGE('',*,*,#10770,.T.);
#14745=ORIENTED_EDGE('',*,*,#10772,.F.);
#14746=ORIENTED_EDGE('',*,*,#10752,.F.);
#14747=ORIENTED_EDGE('',*,*,#10731,.F.);
#14748=ORIENTED_EDGE('',*,*,#10707,.F.);
#14749=ORIENTED_EDGE('',*,*,#10674,.F.);
#14750=ORIENTED_EDGE('',*,*,#10706,.F.);
#14751=ORIENTED_EDGE('',*,*,#10730,.F.);
#14752=ORIENTED_EDGE('',*,*,#10751,.F.);
#14753=ORIENTED_EDGE('',*,*,#10773,.F.);
#14754=ORIENTED_EDGE('',*,*,#10672,.F.);
#14755=ORIENTED_EDGE('',*,*,#10673,.T.);
#14756=ORIENTED_EDGE('',*,*,#10773,.T.);
#14757=ORIENTED_EDGE('',*,*,#10646,.T.);
#14758=ORIENTED_EDGE('',*,*,#10772,.T.);
#14759=ORIENTED_EDGE('',*,*,#10774,.F.);
#14760=ORIENTED_EDGE('',*,*,#10750,.F.);
#14761=ORIENTED_EDGE('',*,*,#10728,.F.);
#14762=ORIENTED_EDGE('',*,*,#10704,.F.);
#14763=ORIENTED_EDGE('',*,*,#10670,.F.);
#14764=ORIENTED_EDGE('',*,*,#10700,.F.);
#14765=ORIENTED_EDGE('',*,*,#10724,.F.);
#14766=ORIENTED_EDGE('',*,*,#10747,.F.);
#14767=ORIENTED_EDGE('',*,*,#10775,.F.);
#14768=ORIENTED_EDGE('',*,*,#10668,.F.);
#14769=ORIENTED_EDGE('',*,*,#10669,.T.);
#14770=ORIENTED_EDGE('',*,*,#10775,.T.);
#14771=ORIENTED_EDGE('',*,*,#10648,.T.);
#14772=ORIENTED_EDGE('',*,*,#10774,.T.);
#14773=ORIENTED_EDGE('',*,*,#10776,.F.);
#14774=ORIENTED_EDGE('',*,*,#10746,.F.);
#14775=ORIENTED_EDGE('',*,*,#10722,.F.);
#14776=ORIENTED_EDGE('',*,*,#10698,.F.);
#14777=ORIENTED_EDGE('',*,*,#10666,.F.);
#14778=ORIENTED_EDGE('',*,*,#10702,.F.);
#14779=ORIENTED_EDGE('',*,*,#10726,.F.);
#14780=ORIENTED_EDGE('',*,*,#10748,.F.);
#14781=ORIENTED_EDGE('',*,*,#10777,.F.);
#14782=ORIENTED_EDGE('',*,*,#10696,.F.);
#14783=ORIENTED_EDGE('',*,*,#10665,.T.);
#14784=ORIENTED_EDGE('',*,*,#10697,.T.);
#14785=ORIENTED_EDGE('',*,*,#10777,.T.);
#14786=ORIENTED_EDGE('',*,*,#10652,.T.);
#14787=ORIENTED_EDGE('',*,*,#10650,.T.);
#14788=ORIENTED_EDGE('',*,*,#10776,.T.);
#14789=ORIENTED_EDGE('',*,*,#10778,.T.);
#14790=ORIENTED_EDGE('',*,*,#10779,.T.);
#14791=ORIENTED_EDGE('',*,*,#10780,.F.);
#14792=ORIENTED_EDGE('',*,*,#10781,.F.);
#14793=ORIENTED_EDGE('',*,*,#10782,.T.);
#14794=ORIENTED_EDGE('',*,*,#10783,.T.);
#14795=ORIENTED_EDGE('',*,*,#10784,.F.);
#14796=ORIENTED_EDGE('',*,*,#10779,.F.);
#14797=ORIENTED_EDGE('',*,*,#10785,.T.);
#14798=ORIENTED_EDGE('',*,*,#10786,.T.);
#14799=ORIENTED_EDGE('',*,*,#10787,.F.);
#14800=ORIENTED_EDGE('',*,*,#10783,.F.);
#14801=ORIENTED_EDGE('',*,*,#10788,.T.);
#14802=ORIENTED_EDGE('',*,*,#10789,.T.);
#14803=ORIENTED_EDGE('',*,*,#10790,.F.);
#14804=ORIENTED_EDGE('',*,*,#10791,.F.);
#14805=ORIENTED_EDGE('',*,*,#10792,.T.);
#14806=ORIENTED_EDGE('',*,*,#10791,.T.);
#14807=ORIENTED_EDGE('',*,*,#10793,.F.);
#14808=ORIENTED_EDGE('',*,*,#10794,.F.);
#14809=ORIENTED_EDGE('',*,*,#10795,.T.);
#14810=ORIENTED_EDGE('',*,*,#10794,.T.);
#14811=ORIENTED_EDGE('',*,*,#10796,.F.);
#14812=ORIENTED_EDGE('',*,*,#10797,.F.);
#14813=ORIENTED_EDGE('',*,*,#10798,.T.);
#14814=ORIENTED_EDGE('',*,*,#10797,.T.);
#14815=ORIENTED_EDGE('',*,*,#10799,.F.);
#14816=ORIENTED_EDGE('',*,*,#10800,.F.);
#14817=ORIENTED_EDGE('',*,*,#10801,.T.);
#14818=ORIENTED_EDGE('',*,*,#10800,.T.);
#14819=ORIENTED_EDGE('',*,*,#10802,.F.);
#14820=ORIENTED_EDGE('',*,*,#10803,.F.);
#14821=ORIENTED_EDGE('',*,*,#10804,.T.);
#14822=ORIENTED_EDGE('',*,*,#10803,.T.);
#14823=ORIENTED_EDGE('',*,*,#10805,.F.);
#14824=ORIENTED_EDGE('',*,*,#10806,.F.);
#14825=ORIENTED_EDGE('',*,*,#10807,.F.);
#14826=ORIENTED_EDGE('',*,*,#10808,.T.);
#14827=ORIENTED_EDGE('',*,*,#10809,.T.);
#14828=ORIENTED_EDGE('',*,*,#10810,.F.);
#14829=ORIENTED_EDGE('',*,*,#10811,.F.);
#14830=ORIENTED_EDGE('',*,*,#10810,.T.);
#14831=ORIENTED_EDGE('',*,*,#10812,.T.);
#14832=ORIENTED_EDGE('',*,*,#10813,.F.);
#14833=ORIENTED_EDGE('',*,*,#10814,.F.);
#14834=ORIENTED_EDGE('',*,*,#10813,.T.);
#14835=ORIENTED_EDGE('',*,*,#10815,.T.);
#14836=ORIENTED_EDGE('',*,*,#10816,.F.);
#14837=ORIENTED_EDGE('',*,*,#10817,.F.);
#14838=ORIENTED_EDGE('',*,*,#10806,.T.);
#14839=ORIENTED_EDGE('',*,*,#10818,.F.);
#14840=ORIENTED_EDGE('',*,*,#10819,.F.);
#14841=ORIENTED_EDGE('',*,*,#10820,.F.);
#14842=ORIENTED_EDGE('',*,*,#10821,.T.);
#14843=ORIENTED_EDGE('',*,*,#10822,.T.);
#14844=ORIENTED_EDGE('',*,*,#10823,.F.);
#14845=ORIENTED_EDGE('',*,*,#10824,.F.);
#14846=ORIENTED_EDGE('',*,*,#10825,.T.);
#14847=ORIENTED_EDGE('',*,*,#10826,.T.);
#14848=ORIENTED_EDGE('',*,*,#10821,.F.);
#14849=ORIENTED_EDGE('',*,*,#10827,.F.);
#14850=ORIENTED_EDGE('',*,*,#10828,.T.);
#14851=ORIENTED_EDGE('',*,*,#10829,.T.);
#14852=ORIENTED_EDGE('',*,*,#10825,.F.);
#14853=ORIENTED_EDGE('',*,*,#10830,.F.);
#14854=ORIENTED_EDGE('',*,*,#10831,.T.);
#14855=ORIENTED_EDGE('',*,*,#10832,.T.);
#14856=ORIENTED_EDGE('',*,*,#10828,.F.);
#14857=ORIENTED_EDGE('',*,*,#10833,.F.);
#14858=ORIENTED_EDGE('',*,*,#10834,.T.);
#14859=ORIENTED_EDGE('',*,*,#10835,.T.);
#14860=ORIENTED_EDGE('',*,*,#10831,.F.);
#14861=ORIENTED_EDGE('',*,*,#10836,.F.);
#14862=ORIENTED_EDGE('',*,*,#10819,.T.);
#14863=ORIENTED_EDGE('',*,*,#10837,.T.);
#14864=ORIENTED_EDGE('',*,*,#10834,.F.);
#14865=ORIENTED_EDGE('',*,*,#10838,.F.);
#14866=ORIENTED_EDGE('',*,*,#10839,.T.);
#14867=ORIENTED_EDGE('',*,*,#10840,.T.);
#14868=ORIENTED_EDGE('',*,*,#10841,.F.);
#14869=ORIENTED_EDGE('',*,*,#10842,.F.);
#14870=ORIENTED_EDGE('',*,*,#10841,.T.);
#14871=ORIENTED_EDGE('',*,*,#10843,.T.);
#14872=ORIENTED_EDGE('',*,*,#10844,.F.);
#14873=ORIENTED_EDGE('',*,*,#10845,.F.);
#14874=ORIENTED_EDGE('',*,*,#10844,.T.);
#14875=ORIENTED_EDGE('',*,*,#10846,.T.);
#14876=ORIENTED_EDGE('',*,*,#10847,.F.);
#14877=ORIENTED_EDGE('',*,*,#10848,.T.);
#14878=ORIENTED_EDGE('',*,*,#10847,.T.);
#14879=ORIENTED_EDGE('',*,*,#10849,.T.);
#14880=ORIENTED_EDGE('',*,*,#10786,.F.);
#14881=ORIENTED_EDGE('',*,*,#10850,.F.);
#14882=ORIENTED_EDGE('',*,*,#10851,.T.);
#14883=ORIENTED_EDGE('',*,*,#10852,.T.);
#14884=ORIENTED_EDGE('',*,*,#10853,.F.);
#14885=ORIENTED_EDGE('',*,*,#10854,.F.);
#14886=ORIENTED_EDGE('',*,*,#10855,.T.);
#14887=ORIENTED_EDGE('',*,*,#10856,.T.);
#14888=ORIENTED_EDGE('',*,*,#10851,.F.);
#14889=ORIENTED_EDGE('',*,*,#10857,.F.);
#14890=ORIENTED_EDGE('',*,*,#10858,.T.);
#14891=ORIENTED_EDGE('',*,*,#10859,.T.);
#14892=ORIENTED_EDGE('',*,*,#10855,.F.);
#14893=ORIENTED_EDGE('',*,*,#10860,.F.);
#14894=ORIENTED_EDGE('',*,*,#10861,.T.);
#14895=ORIENTED_EDGE('',*,*,#10862,.T.);
#14896=ORIENTED_EDGE('',*,*,#10858,.F.);
#14897=ORIENTED_EDGE('',*,*,#10863,.F.);
#14898=ORIENTED_EDGE('',*,*,#10864,.T.);
#14899=ORIENTED_EDGE('',*,*,#10865,.T.);
#14900=ORIENTED_EDGE('',*,*,#10861,.F.);
#14901=ORIENTED_EDGE('',*,*,#10866,.F.);
#14902=ORIENTED_EDGE('',*,*,#10867,.T.);
#14903=ORIENTED_EDGE('',*,*,#10868,.T.);
#14904=ORIENTED_EDGE('',*,*,#10864,.F.);
#14905=ORIENTED_EDGE('',*,*,#10869,.T.);
#14906=ORIENTED_EDGE('',*,*,#10870,.T.);
#14907=ORIENTED_EDGE('',*,*,#10871,.F.);
#14908=ORIENTED_EDGE('',*,*,#10872,.F.);
#14909=ORIENTED_EDGE('',*,*,#10873,.T.);
#14910=ORIENTED_EDGE('',*,*,#10874,.T.);
#14911=ORIENTED_EDGE('',*,*,#10875,.F.);
#14912=ORIENTED_EDGE('',*,*,#10870,.F.);
#14913=ORIENTED_EDGE('',*,*,#10876,.T.);
#14914=ORIENTED_EDGE('',*,*,#10877,.T.);
#14915=ORIENTED_EDGE('',*,*,#10878,.F.);
#14916=ORIENTED_EDGE('',*,*,#10874,.F.);
#14917=ORIENTED_EDGE('',*,*,#10879,.F.);
#14918=ORIENTED_EDGE('',*,*,#10816,.T.);
#14919=ORIENTED_EDGE('',*,*,#10880,.F.);
#14920=ORIENTED_EDGE('',*,*,#10877,.F.);
#14921=ORIENTED_EDGE('',*,*,#10881,.T.);
#14922=ORIENTED_EDGE('',*,*,#10882,.T.);
#14923=ORIENTED_EDGE('',*,*,#10883,.F.);
#14924=ORIENTED_EDGE('',*,*,#10882,.F.);
#14925=ORIENTED_EDGE('',*,*,#10884,.T.);
#14926=ORIENTED_EDGE('',*,*,#10885,.T.);
#14927=ORIENTED_EDGE('',*,*,#10886,.T.);
#14928=ORIENTED_EDGE('',*,*,#10867,.F.);
#14929=ORIENTED_EDGE('',*,*,#10887,.T.);
#14930=ORIENTED_EDGE('',*,*,#10888,.T.);
#14931=ORIENTED_EDGE('',*,*,#10889,.F.);
#14932=ORIENTED_EDGE('',*,*,#10890,.F.);
#14933=ORIENTED_EDGE('',*,*,#10891,.T.);
#14934=ORIENTED_EDGE('',*,*,#10890,.T.);
#14935=ORIENTED_EDGE('',*,*,#10892,.F.);
#14936=ORIENTED_EDGE('',*,*,#10893,.F.);
#14937=ORIENTED_EDGE('',*,*,#10894,.T.);
#14938=ORIENTED_EDGE('',*,*,#10893,.T.);
#14939=ORIENTED_EDGE('',*,*,#10895,.F.);
#14940=ORIENTED_EDGE('',*,*,#10896,.F.);
#14941=ORIENTED_EDGE('',*,*,#10897,.T.);
#14942=ORIENTED_EDGE('',*,*,#10896,.T.);
#14943=ORIENTED_EDGE('',*,*,#10898,.F.);
#14944=ORIENTED_EDGE('',*,*,#10899,.F.);
#14945=ORIENTED_EDGE('',*,*,#10900,.T.);
#14946=ORIENTED_EDGE('',*,*,#10899,.T.);
#14947=ORIENTED_EDGE('',*,*,#10901,.F.);
#14948=ORIENTED_EDGE('',*,*,#10902,.F.);
#14949=ORIENTED_EDGE('',*,*,#10903,.T.);
#14950=ORIENTED_EDGE('',*,*,#10902,.T.);
#14951=ORIENTED_EDGE('',*,*,#10904,.F.);
#14952=ORIENTED_EDGE('',*,*,#10885,.F.);
#14953=ORIENTED_EDGE('',*,*,#10905,.F.);
#14954=ORIENTED_EDGE('',*,*,#10906,.T.);
#14955=ORIENTED_EDGE('',*,*,#10907,.T.);
#14956=ORIENTED_EDGE('',*,*,#10908,.F.);
#14957=ORIENTED_EDGE('',*,*,#10909,.F.);
#14958=ORIENTED_EDGE('',*,*,#10908,.T.);
#14959=ORIENTED_EDGE('',*,*,#10910,.T.);
#14960=ORIENTED_EDGE('',*,*,#10911,.F.);
#14961=ORIENTED_EDGE('',*,*,#10912,.F.);
#14962=ORIENTED_EDGE('',*,*,#10911,.T.);
#14963=ORIENTED_EDGE('',*,*,#10913,.T.);
#14964=ORIENTED_EDGE('',*,*,#10914,.F.);
#14965=ORIENTED_EDGE('',*,*,#10915,.F.);
#14966=ORIENTED_EDGE('',*,*,#10914,.T.);
#14967=ORIENTED_EDGE('',*,*,#10916,.T.);
#14968=ORIENTED_EDGE('',*,*,#10917,.F.);
#14969=ORIENTED_EDGE('',*,*,#10918,.F.);
#14970=ORIENTED_EDGE('',*,*,#10919,.T.);
#14971=ORIENTED_EDGE('',*,*,#10920,.T.);
#14972=ORIENTED_EDGE('',*,*,#10921,.F.);
#14973=ORIENTED_EDGE('',*,*,#10922,.F.);
#14974=ORIENTED_EDGE('',*,*,#10921,.T.);
#14975=ORIENTED_EDGE('',*,*,#10923,.T.);
#14976=ORIENTED_EDGE('',*,*,#10924,.F.);
#14977=ORIENTED_EDGE('',*,*,#10925,.F.);
#14978=ORIENTED_EDGE('',*,*,#10924,.T.);
#14979=ORIENTED_EDGE('',*,*,#10926,.T.);
#14980=ORIENTED_EDGE('',*,*,#10927,.F.);
#14981=ORIENTED_EDGE('',*,*,#10928,.F.);
#14982=ORIENTED_EDGE('',*,*,#10927,.T.);
#14983=ORIENTED_EDGE('',*,*,#10929,.T.);
#14984=ORIENTED_EDGE('',*,*,#10930,.F.);
#14985=ORIENTED_EDGE('',*,*,#10931,.F.);
#14986=ORIENTED_EDGE('',*,*,#10930,.T.);
#14987=ORIENTED_EDGE('',*,*,#10932,.T.);
#14988=ORIENTED_EDGE('',*,*,#10933,.F.);
#14989=ORIENTED_EDGE('',*,*,#10934,.F.);
#14990=ORIENTED_EDGE('',*,*,#10933,.T.);
#14991=ORIENTED_EDGE('',*,*,#10935,.T.);
#14992=ORIENTED_EDGE('',*,*,#10936,.F.);
#14993=ORIENTED_EDGE('',*,*,#10937,.T.);
#14994=ORIENTED_EDGE('',*,*,#10936,.T.);
#14995=ORIENTED_EDGE('',*,*,#10938,.T.);
#14996=ORIENTED_EDGE('',*,*,#10888,.F.);
#14997=ORIENTED_EDGE('',*,*,#10939,.F.);
#14998=ORIENTED_EDGE('',*,*,#10872,.T.);
#14999=ORIENTED_EDGE('',*,*,#10940,.F.);
#15000=ORIENTED_EDGE('',*,*,#10941,.F.);
#15001=ORIENTED_EDGE('',*,*,#10942,.F.);
#15002=ORIENTED_EDGE('',*,*,#10941,.T.);
#15003=ORIENTED_EDGE('',*,*,#10943,.T.);
#15004=ORIENTED_EDGE('',*,*,#10944,.F.);
#15005=ORIENTED_EDGE('',*,*,#10945,.F.);
#15006=ORIENTED_EDGE('',*,*,#10944,.T.);
#15007=ORIENTED_EDGE('',*,*,#10946,.T.);
#15008=ORIENTED_EDGE('',*,*,#10947,.F.);
#15009=ORIENTED_EDGE('',*,*,#10948,.F.);
#15010=ORIENTED_EDGE('',*,*,#10947,.T.);
#15011=ORIENTED_EDGE('',*,*,#10949,.T.);
#15012=ORIENTED_EDGE('',*,*,#10950,.F.);
#15013=ORIENTED_EDGE('',*,*,#10951,.F.);
#15014=ORIENTED_EDGE('',*,*,#10952,.T.);
#15015=ORIENTED_EDGE('',*,*,#10953,.T.);
#15016=ORIENTED_EDGE('',*,*,#10906,.F.);
#15017=ORIENTED_EDGE('',*,*,#10954,.F.);
#15018=ORIENTED_EDGE('',*,*,#10955,.T.);
#15019=ORIENTED_EDGE('',*,*,#10956,.T.);
#15020=ORIENTED_EDGE('',*,*,#10952,.F.);
#15021=ORIENTED_EDGE('',*,*,#10957,.F.);
#15022=ORIENTED_EDGE('',*,*,#10958,.T.);
#15023=ORIENTED_EDGE('',*,*,#10959,.T.);
#15024=ORIENTED_EDGE('',*,*,#10955,.F.);
#15025=ORIENTED_EDGE('',*,*,#10960,.F.);
#15026=ORIENTED_EDGE('',*,*,#10917,.T.);
#15027=ORIENTED_EDGE('',*,*,#10961,.T.);
#15028=ORIENTED_EDGE('',*,*,#10958,.F.);
#15029=ORIENTED_EDGE('',*,*,#10962,.F.);
#15030=ORIENTED_EDGE('',*,*,#10963,.T.);
#15031=ORIENTED_EDGE('',*,*,#10964,.T.);
#15032=ORIENTED_EDGE('',*,*,#10919,.F.);
#15033=ORIENTED_EDGE('',*,*,#10965,.F.);
#15034=ORIENTED_EDGE('',*,*,#10966,.T.);
#15035=ORIENTED_EDGE('',*,*,#10967,.T.);
#15036=ORIENTED_EDGE('',*,*,#10963,.F.);
#15037=ORIENTED_EDGE('',*,*,#10968,.F.);
#15038=ORIENTED_EDGE('',*,*,#10969,.T.);
#15039=ORIENTED_EDGE('',*,*,#10970,.T.);
#15040=ORIENTED_EDGE('',*,*,#10966,.F.);
#15041=ORIENTED_EDGE('',*,*,#10971,.F.);
#15042=ORIENTED_EDGE('',*,*,#10972,.T.);
#15043=ORIENTED_EDGE('',*,*,#10973,.T.);
#15044=ORIENTED_EDGE('',*,*,#10969,.F.);
#15045=ORIENTED_EDGE('',*,*,#10974,.F.);
#15046=ORIENTED_EDGE('',*,*,#10975,.T.);
#15047=ORIENTED_EDGE('',*,*,#10976,.T.);
#15048=ORIENTED_EDGE('',*,*,#10972,.F.);
#15049=ORIENTED_EDGE('',*,*,#10977,.F.);
#15050=ORIENTED_EDGE('',*,*,#10978,.T.);
#15051=ORIENTED_EDGE('',*,*,#10979,.T.);
#15052=ORIENTED_EDGE('',*,*,#10975,.F.);
#15053=ORIENTED_EDGE('',*,*,#10980,.F.);
#15054=ORIENTED_EDGE('',*,*,#10981,.T.);
#15055=ORIENTED_EDGE('',*,*,#10982,.T.);
#15056=ORIENTED_EDGE('',*,*,#10978,.F.);
#15057=ORIENTED_EDGE('',*,*,#10983,.F.);
#15058=ORIENTED_EDGE('',*,*,#10984,.T.);
#15059=ORIENTED_EDGE('',*,*,#10985,.T.);
#15060=ORIENTED_EDGE('',*,*,#10981,.F.);
#15061=ORIENTED_EDGE('',*,*,#10986,.F.);
#15062=ORIENTED_EDGE('',*,*,#10987,.T.);
#15063=ORIENTED_EDGE('',*,*,#10988,.T.);
#15064=ORIENTED_EDGE('',*,*,#10984,.F.);
#15065=ORIENTED_EDGE('',*,*,#10989,.F.);
#15066=ORIENTED_EDGE('',*,*,#10990,.T.);
#15067=ORIENTED_EDGE('',*,*,#10991,.T.);
#15068=ORIENTED_EDGE('',*,*,#10987,.F.);
#15069=ORIENTED_EDGE('',*,*,#10992,.F.);
#15070=ORIENTED_EDGE('',*,*,#10993,.T.);
#15071=ORIENTED_EDGE('',*,*,#10994,.T.);
#15072=ORIENTED_EDGE('',*,*,#10990,.F.);
#15073=ORIENTED_EDGE('',*,*,#10995,.F.);
#15074=ORIENTED_EDGE('',*,*,#10996,.T.);
#15075=ORIENTED_EDGE('',*,*,#10997,.T.);
#15076=ORIENTED_EDGE('',*,*,#10993,.F.);
#15077=ORIENTED_EDGE('',*,*,#10998,.F.);
#15078=ORIENTED_EDGE('',*,*,#10999,.T.);
#15079=ORIENTED_EDGE('',*,*,#11000,.T.);
#15080=ORIENTED_EDGE('',*,*,#10996,.F.);
#15081=ORIENTED_EDGE('',*,*,#11001,.F.);
#15082=ORIENTED_EDGE('',*,*,#11002,.T.);
#15083=ORIENTED_EDGE('',*,*,#11003,.T.);
#15084=ORIENTED_EDGE('',*,*,#10999,.F.);
#15085=ORIENTED_EDGE('',*,*,#11004,.F.);
#15086=ORIENTED_EDGE('',*,*,#11005,.T.);
#15087=ORIENTED_EDGE('',*,*,#11006,.T.);
#15088=ORIENTED_EDGE('',*,*,#11002,.F.);
#15089=ORIENTED_EDGE('',*,*,#11007,.F.);
#15090=ORIENTED_EDGE('',*,*,#11008,.T.);
#15091=ORIENTED_EDGE('',*,*,#11009,.T.);
#15092=ORIENTED_EDGE('',*,*,#11005,.F.);
#15093=ORIENTED_EDGE('',*,*,#11010,.T.);
#15094=ORIENTED_EDGE('',*,*,#11011,.T.);
#15095=ORIENTED_EDGE('',*,*,#11012,.F.);
#15096=ORIENTED_EDGE('',*,*,#11013,.F.);
#15097=ORIENTED_EDGE('',*,*,#11014,.T.);
#15098=ORIENTED_EDGE('',*,*,#11015,.T.);
#15099=ORIENTED_EDGE('',*,*,#11016,.F.);
#15100=ORIENTED_EDGE('',*,*,#11011,.F.);
#15101=ORIENTED_EDGE('',*,*,#11017,.T.);
#15102=ORIENTED_EDGE('',*,*,#11018,.T.);
#15103=ORIENTED_EDGE('',*,*,#11019,.F.);
#15104=ORIENTED_EDGE('',*,*,#11015,.F.);
#15105=ORIENTED_EDGE('',*,*,#11020,.T.);
#15106=ORIENTED_EDGE('',*,*,#11021,.T.);
#15107=ORIENTED_EDGE('',*,*,#11022,.F.);
#15108=ORIENTED_EDGE('',*,*,#11018,.F.);
#15109=ORIENTED_EDGE('',*,*,#11023,.T.);
#15110=ORIENTED_EDGE('',*,*,#11024,.T.);
#15111=ORIENTED_EDGE('',*,*,#11025,.F.);
#15112=ORIENTED_EDGE('',*,*,#11026,.F.);
#15113=ORIENTED_EDGE('',*,*,#11027,.T.);
#15114=ORIENTED_EDGE('',*,*,#11028,.T.);
#15115=ORIENTED_EDGE('',*,*,#11029,.F.);
#15116=ORIENTED_EDGE('',*,*,#11024,.F.);
#15117=ORIENTED_EDGE('',*,*,#11030,.T.);
#15118=ORIENTED_EDGE('',*,*,#11031,.T.);
#15119=ORIENTED_EDGE('',*,*,#11032,.F.);
#15120=ORIENTED_EDGE('',*,*,#11028,.F.);
#15121=ORIENTED_EDGE('',*,*,#11033,.T.);
#15122=ORIENTED_EDGE('',*,*,#11034,.T.);
#15123=ORIENTED_EDGE('',*,*,#11035,.F.);
#15124=ORIENTED_EDGE('',*,*,#11031,.F.);
#15125=ORIENTED_EDGE('',*,*,#11036,.T.);
#15126=ORIENTED_EDGE('',*,*,#11037,.T.);
#15127=ORIENTED_EDGE('',*,*,#11038,.F.);
#15128=ORIENTED_EDGE('',*,*,#11034,.F.);
#15129=ORIENTED_EDGE('',*,*,#11039,.T.);
#15130=ORIENTED_EDGE('',*,*,#11040,.T.);
#15131=ORIENTED_EDGE('',*,*,#11041,.F.);
#15132=ORIENTED_EDGE('',*,*,#11037,.F.);
#15133=ORIENTED_EDGE('',*,*,#11042,.F.);
#15134=ORIENTED_EDGE('',*,*,#10823,.T.);
#15135=ORIENTED_EDGE('',*,*,#11043,.F.);
#15136=ORIENTED_EDGE('',*,*,#11040,.F.);
#15137=ORIENTED_EDGE('',*,*,#11044,.T.);
#15138=ORIENTED_EDGE('',*,*,#11045,.T.);
#15139=ORIENTED_EDGE('',*,*,#11046,.T.);
#15140=ORIENTED_EDGE('',*,*,#10808,.F.);
#15141=ORIENTED_EDGE('',*,*,#11047,.T.);
#15142=ORIENTED_EDGE('',*,*,#11048,.T.);
#15143=ORIENTED_EDGE('',*,*,#11049,.F.);
#15144=ORIENTED_EDGE('',*,*,#11045,.F.);
#15145=ORIENTED_EDGE('',*,*,#11050,.T.);
#15146=ORIENTED_EDGE('',*,*,#11051,.T.);
#15147=ORIENTED_EDGE('',*,*,#11052,.F.);
#15148=ORIENTED_EDGE('',*,*,#11048,.F.);
#15149=ORIENTED_EDGE('',*,*,#11053,.T.);
#15150=ORIENTED_EDGE('',*,*,#11054,.T.);
#15151=ORIENTED_EDGE('',*,*,#11055,.F.);
#15152=ORIENTED_EDGE('',*,*,#11051,.F.);
#15153=ORIENTED_EDGE('',*,*,#11056,.F.);
#15154=ORIENTED_EDGE('',*,*,#10950,.T.);
#15155=ORIENTED_EDGE('',*,*,#11057,.F.);
#15156=ORIENTED_EDGE('',*,*,#11054,.F.);
#15157=ORIENTED_EDGE('',*,*,#11058,.F.);
#15158=ORIENTED_EDGE('',*,*,#11059,.T.);
#15159=ORIENTED_EDGE('',*,*,#11060,.F.);
#15160=ORIENTED_EDGE('',*,*,#11059,.F.);
#15161=ORIENTED_EDGE('',*,*,#11061,.T.);
#15162=ORIENTED_EDGE('',*,*,#11062,.T.);
#15163=ORIENTED_EDGE('',*,*,#11063,.T.);
#15164=ORIENTED_EDGE('',*,*,#11008,.F.);
#15165=ORIENTED_EDGE('',*,*,#11064,.T.);
#15166=ORIENTED_EDGE('',*,*,#11013,.T.);
#15167=ORIENTED_EDGE('',*,*,#11065,.F.);
#15168=ORIENTED_EDGE('',*,*,#11066,.F.);
#15169=ORIENTED_EDGE('',*,*,#11067,.T.);
#15170=ORIENTED_EDGE('',*,*,#11066,.T.);
#15171=ORIENTED_EDGE('',*,*,#11068,.F.);
#15172=ORIENTED_EDGE('',*,*,#11069,.F.);
#15173=ORIENTED_EDGE('',*,*,#11070,.T.);
#15174=ORIENTED_EDGE('',*,*,#11069,.T.);
#15175=ORIENTED_EDGE('',*,*,#11071,.F.);
#15176=ORIENTED_EDGE('',*,*,#11072,.F.);
#15177=ORIENTED_EDGE('',*,*,#11073,.T.);
#15178=ORIENTED_EDGE('',*,*,#11072,.T.);
#15179=ORIENTED_EDGE('',*,*,#11074,.F.);
#15180=ORIENTED_EDGE('',*,*,#11021,.F.);
#15181=ORIENTED_EDGE('',*,*,#11075,.T.);
#15182=ORIENTED_EDGE('',*,*,#11026,.T.);
#15183=ORIENTED_EDGE('',*,*,#11076,.F.);
#15184=ORIENTED_EDGE('',*,*,#11077,.F.);
#15185=ORIENTED_EDGE('',*,*,#11078,.T.);
#15186=ORIENTED_EDGE('',*,*,#11077,.T.);
#15187=ORIENTED_EDGE('',*,*,#11079,.F.);
#15188=ORIENTED_EDGE('',*,*,#11080,.F.);
#15189=ORIENTED_EDGE('',*,*,#11081,.T.);
#15190=ORIENTED_EDGE('',*,*,#11080,.T.);
#15191=ORIENTED_EDGE('',*,*,#11082,.F.);
#15192=ORIENTED_EDGE('',*,*,#11083,.F.);
#15193=ORIENTED_EDGE('',*,*,#11084,.T.);
#15194=ORIENTED_EDGE('',*,*,#11083,.T.);
#15195=ORIENTED_EDGE('',*,*,#11085,.F.);
#15196=ORIENTED_EDGE('',*,*,#11086,.F.);
#15197=ORIENTED_EDGE('',*,*,#11087,.T.);
#15198=ORIENTED_EDGE('',*,*,#11086,.T.);
#15199=ORIENTED_EDGE('',*,*,#11088,.F.);
#15200=ORIENTED_EDGE('',*,*,#11089,.F.);
#15201=ORIENTED_EDGE('',*,*,#11090,.T.);
#15202=ORIENTED_EDGE('',*,*,#11089,.T.);
#15203=ORIENTED_EDGE('',*,*,#11091,.F.);
#15204=ORIENTED_EDGE('',*,*,#11092,.F.);
#15205=ORIENTED_EDGE('',*,*,#11093,.T.);
#15206=ORIENTED_EDGE('',*,*,#11092,.T.);
#15207=ORIENTED_EDGE('',*,*,#11094,.F.);
#15208=ORIENTED_EDGE('',*,*,#11095,.F.);
#15209=ORIENTED_EDGE('',*,*,#11096,.T.);
#15210=ORIENTED_EDGE('',*,*,#11095,.T.);
#15211=ORIENTED_EDGE('',*,*,#11097,.F.);
#15212=ORIENTED_EDGE('',*,*,#11098,.F.);
#15213=ORIENTED_EDGE('',*,*,#11099,.T.);
#15214=ORIENTED_EDGE('',*,*,#11098,.T.);
#15215=ORIENTED_EDGE('',*,*,#11100,.F.);
#15216=ORIENTED_EDGE('',*,*,#11101,.F.);
#15217=ORIENTED_EDGE('',*,*,#11102,.T.);
#15218=ORIENTED_EDGE('',*,*,#11101,.T.);
#15219=ORIENTED_EDGE('',*,*,#11103,.F.);
#15220=ORIENTED_EDGE('',*,*,#11104,.F.);
#15221=ORIENTED_EDGE('',*,*,#11105,.T.);
#15222=ORIENTED_EDGE('',*,*,#11104,.T.);
#15223=ORIENTED_EDGE('',*,*,#11106,.F.);
#15224=ORIENTED_EDGE('',*,*,#11107,.F.);
#15225=ORIENTED_EDGE('',*,*,#11108,.T.);
#15226=ORIENTED_EDGE('',*,*,#11107,.T.);
#15227=ORIENTED_EDGE('',*,*,#11109,.F.);
#15228=ORIENTED_EDGE('',*,*,#11110,.F.);
#15229=ORIENTED_EDGE('',*,*,#11111,.T.);
#15230=ORIENTED_EDGE('',*,*,#11110,.T.);
#15231=ORIENTED_EDGE('',*,*,#11112,.F.);
#15232=ORIENTED_EDGE('',*,*,#11113,.F.);
#15233=ORIENTED_EDGE('',*,*,#11114,.T.);
#15234=ORIENTED_EDGE('',*,*,#11113,.T.);
#15235=ORIENTED_EDGE('',*,*,#11115,.F.);
#15236=ORIENTED_EDGE('',*,*,#11116,.F.);
#15237=ORIENTED_EDGE('',*,*,#11117,.T.);
#15238=ORIENTED_EDGE('',*,*,#11116,.T.);
#15239=ORIENTED_EDGE('',*,*,#11118,.F.);
#15240=ORIENTED_EDGE('',*,*,#11119,.F.);
#15241=ORIENTED_EDGE('',*,*,#11120,.T.);
#15242=ORIENTED_EDGE('',*,*,#11119,.T.);
#15243=ORIENTED_EDGE('',*,*,#11121,.F.);
#15244=ORIENTED_EDGE('',*,*,#11062,.F.);
#15245=ORIENTED_EDGE('',*,*,#11122,.T.);
#15246=ORIENTED_EDGE('',*,*,#11123,.T.);
#15247=ORIENTED_EDGE('',*,*,#11124,.F.);
#15248=ORIENTED_EDGE('',*,*,#11125,.F.);
#15249=ORIENTED_EDGE('',*,*,#11126,.T.);
#15250=ORIENTED_EDGE('',*,*,#11127,.T.);
#15251=ORIENTED_EDGE('',*,*,#11128,.F.);
#15252=ORIENTED_EDGE('',*,*,#11123,.F.);
#15253=ORIENTED_EDGE('',*,*,#11129,.T.);
#15254=ORIENTED_EDGE('',*,*,#11130,.T.);
#15255=ORIENTED_EDGE('',*,*,#11131,.F.);
#15256=ORIENTED_EDGE('',*,*,#11127,.F.);
#15257=ORIENTED_EDGE('',*,*,#11132,.T.);
#15258=ORIENTED_EDGE('',*,*,#11133,.T.);
#15259=ORIENTED_EDGE('',*,*,#11134,.F.);
#15260=ORIENTED_EDGE('',*,*,#11135,.F.);
#15261=ORIENTED_EDGE('',*,*,#11136,.T.);
#15262=ORIENTED_EDGE('',*,*,#11135,.T.);
#15263=ORIENTED_EDGE('',*,*,#11137,.F.);
#15264=ORIENTED_EDGE('',*,*,#11138,.F.);
#15265=ORIENTED_EDGE('',*,*,#11139,.T.);
#15266=ORIENTED_EDGE('',*,*,#11138,.T.);
#15267=ORIENTED_EDGE('',*,*,#11140,.F.);
#15268=ORIENTED_EDGE('',*,*,#11141,.F.);
#15269=ORIENTED_EDGE('',*,*,#11142,.T.);
#15270=ORIENTED_EDGE('',*,*,#11141,.T.);
#15271=ORIENTED_EDGE('',*,*,#11143,.F.);
#15272=ORIENTED_EDGE('',*,*,#11144,.F.);
#15273=ORIENTED_EDGE('',*,*,#11145,.T.);
#15274=ORIENTED_EDGE('',*,*,#11144,.T.);
#15275=ORIENTED_EDGE('',*,*,#11146,.F.);
#15276=ORIENTED_EDGE('',*,*,#11147,.F.);
#15277=ORIENTED_EDGE('',*,*,#11148,.T.);
#15278=ORIENTED_EDGE('',*,*,#11147,.T.);
#15279=ORIENTED_EDGE('',*,*,#11149,.F.);
#15280=ORIENTED_EDGE('',*,*,#11150,.F.);
#15281=ORIENTED_EDGE('',*,*,#11151,.F.);
#15282=ORIENTED_EDGE('',*,*,#10781,.T.);
#15283=ORIENTED_EDGE('',*,*,#11152,.T.);
#15284=ORIENTED_EDGE('',*,*,#11153,.F.);
#15285=ORIENTED_EDGE('',*,*,#11154,.F.);
#15286=ORIENTED_EDGE('',*,*,#11153,.T.);
#15287=ORIENTED_EDGE('',*,*,#11155,.T.);
#15288=ORIENTED_EDGE('',*,*,#11156,.F.);
#15289=ORIENTED_EDGE('',*,*,#11157,.F.);
#15290=ORIENTED_EDGE('',*,*,#11156,.T.);
#15291=ORIENTED_EDGE('',*,*,#11158,.T.);
#15292=ORIENTED_EDGE('',*,*,#11159,.F.);
#15293=ORIENTED_EDGE('',*,*,#11160,.F.);
#15294=ORIENTED_EDGE('',*,*,#11159,.T.);
#15295=ORIENTED_EDGE('',*,*,#11161,.T.);
#15296=ORIENTED_EDGE('',*,*,#11162,.F.);
#15297=ORIENTED_EDGE('',*,*,#11163,.F.);
#15298=ORIENTED_EDGE('',*,*,#11150,.T.);
#15299=ORIENTED_EDGE('',*,*,#11164,.F.);
#15300=ORIENTED_EDGE('',*,*,#11165,.F.);
#15301=ORIENTED_EDGE('',*,*,#11166,.T.);
#15302=ORIENTED_EDGE('',*,*,#11167,.T.);
#15303=ORIENTED_EDGE('',*,*,#11168,.T.);
#15304=ORIENTED_EDGE('',*,*,#10789,.F.);
#15305=ORIENTED_EDGE('',*,*,#11169,.F.);
#15306=ORIENTED_EDGE('',*,*,#11170,.T.);
#15307=ORIENTED_EDGE('',*,*,#11171,.T.);
#15308=ORIENTED_EDGE('',*,*,#11167,.F.);
#15309=ORIENTED_EDGE('',*,*,#11172,.F.);
#15310=ORIENTED_EDGE('',*,*,#11173,.T.);
#15311=ORIENTED_EDGE('',*,*,#11174,.T.);
#15312=ORIENTED_EDGE('',*,*,#11170,.F.);
#15313=ORIENTED_EDGE('',*,*,#11175,.F.);
#15314=ORIENTED_EDGE('',*,*,#11176,.T.);
#15315=ORIENTED_EDGE('',*,*,#11177,.T.);
#15316=ORIENTED_EDGE('',*,*,#11173,.F.);
#15317=ORIENTED_EDGE('',*,*,#11178,.F.);
#15318=ORIENTED_EDGE('',*,*,#11179,.T.);
#15319=ORIENTED_EDGE('',*,*,#11180,.T.);
#15320=ORIENTED_EDGE('',*,*,#11176,.F.);
#15321=ORIENTED_EDGE('',*,*,#11181,.F.);
#15322=ORIENTED_EDGE('',*,*,#11182,.T.);
#15323=ORIENTED_EDGE('',*,*,#11183,.T.);
#15324=ORIENTED_EDGE('',*,*,#11179,.F.);
#15325=ORIENTED_EDGE('',*,*,#11184,.F.);
#15326=ORIENTED_EDGE('',*,*,#11165,.T.);
#15327=ORIENTED_EDGE('',*,*,#11185,.T.);
#15328=ORIENTED_EDGE('',*,*,#11182,.F.);
#15329=ORIENTED_EDGE('',*,*,#11186,.F.);
#15330=ORIENTED_EDGE('',*,*,#11187,.T.);
#15331=ORIENTED_EDGE('',*,*,#11188,.T.);
#15332=ORIENTED_EDGE('',*,*,#11189,.F.);
#15333=ORIENTED_EDGE('',*,*,#11190,.F.);
#15334=ORIENTED_EDGE('',*,*,#11189,.T.);
#15335=ORIENTED_EDGE('',*,*,#11191,.T.);
#15336=ORIENTED_EDGE('',*,*,#11192,.F.);
#15337=ORIENTED_EDGE('',*,*,#11193,.F.);
#15338=ORIENTED_EDGE('',*,*,#11192,.T.);
#15339=ORIENTED_EDGE('',*,*,#11194,.T.);
#15340=ORIENTED_EDGE('',*,*,#11195,.F.);
#15341=ORIENTED_EDGE('',*,*,#11196,.T.);
#15342=ORIENTED_EDGE('',*,*,#11195,.T.);
#15343=ORIENTED_EDGE('',*,*,#11197,.T.);
#15344=ORIENTED_EDGE('',*,*,#11130,.F.);
#15345=ORIENTED_EDGE('',*,*,#11198,.F.);
#15346=ORIENTED_EDGE('',*,*,#11199,.T.);
#15347=ORIENTED_EDGE('',*,*,#11200,.T.);
#15348=ORIENTED_EDGE('',*,*,#11201,.F.);
#15349=ORIENTED_EDGE('',*,*,#11202,.F.);
#15350=ORIENTED_EDGE('',*,*,#11203,.T.);
#15351=ORIENTED_EDGE('',*,*,#11204,.T.);
#15352=ORIENTED_EDGE('',*,*,#11199,.F.);
#15353=ORIENTED_EDGE('',*,*,#11205,.F.);
#15354=ORIENTED_EDGE('',*,*,#11206,.T.);
#15355=ORIENTED_EDGE('',*,*,#11207,.T.);
#15356=ORIENTED_EDGE('',*,*,#11203,.F.);
#15357=ORIENTED_EDGE('',*,*,#11208,.F.);
#15358=ORIENTED_EDGE('',*,*,#11209,.T.);
#15359=ORIENTED_EDGE('',*,*,#11210,.T.);
#15360=ORIENTED_EDGE('',*,*,#11206,.F.);
#15361=ORIENTED_EDGE('',*,*,#11211,.F.);
#15362=ORIENTED_EDGE('',*,*,#11212,.T.);
#15363=ORIENTED_EDGE('',*,*,#11213,.T.);
#15364=ORIENTED_EDGE('',*,*,#11209,.F.);
#15365=ORIENTED_EDGE('',*,*,#11214,.F.);
#15366=ORIENTED_EDGE('',*,*,#11215,.T.);
#15367=ORIENTED_EDGE('',*,*,#11216,.T.);
#15368=ORIENTED_EDGE('',*,*,#11212,.F.);
#15369=ORIENTED_EDGE('',*,*,#11217,.T.);
#15370=ORIENTED_EDGE('',*,*,#11218,.T.);
#15371=ORIENTED_EDGE('',*,*,#11219,.T.);
#15372=ORIENTED_EDGE('',*,*,#10839,.F.);
#15373=ORIENTED_EDGE('',*,*,#11220,.T.);
#15374=ORIENTED_EDGE('',*,*,#11221,.T.);
#15375=ORIENTED_EDGE('',*,*,#11222,.F.);
#15376=ORIENTED_EDGE('',*,*,#11218,.F.);
#15377=ORIENTED_EDGE('',*,*,#11223,.T.);
#15378=ORIENTED_EDGE('',*,*,#11224,.T.);
#15379=ORIENTED_EDGE('',*,*,#11225,.F.);
#15380=ORIENTED_EDGE('',*,*,#11221,.F.);
#15381=ORIENTED_EDGE('',*,*,#11226,.T.);
#15382=ORIENTED_EDGE('',*,*,#11227,.T.);
#15383=ORIENTED_EDGE('',*,*,#11228,.F.);
#15384=ORIENTED_EDGE('',*,*,#11224,.F.);
#15385=ORIENTED_EDGE('',*,*,#11229,.F.);
#15386=ORIENTED_EDGE('',*,*,#11162,.T.);
#15387=ORIENTED_EDGE('',*,*,#11230,.F.);
#15388=ORIENTED_EDGE('',*,*,#11227,.F.);
#15389=ORIENTED_EDGE('',*,*,#11231,.T.);
#15390=ORIENTED_EDGE('',*,*,#11232,.T.);
#15391=ORIENTED_EDGE('',*,*,#11233,.F.);
#15392=ORIENTED_EDGE('',*,*,#11232,.F.);
#15393=ORIENTED_EDGE('',*,*,#11234,.T.);
#15394=ORIENTED_EDGE('',*,*,#11235,.T.);
#15395=ORIENTED_EDGE('',*,*,#11236,.T.);
#15396=ORIENTED_EDGE('',*,*,#11215,.F.);
#15397=ORIENTED_EDGE('',*,*,#11237,.F.);
#15398=ORIENTED_EDGE('',*,*,#10853,.T.);
#15399=ORIENTED_EDGE('',*,*,#11238,.F.);
#15400=ORIENTED_EDGE('',*,*,#11239,.F.);
#15401=ORIENTED_EDGE('',*,*,#11240,.T.);
#15402=ORIENTED_EDGE('',*,*,#11239,.T.);
#15403=ORIENTED_EDGE('',*,*,#11241,.F.);
#15404=ORIENTED_EDGE('',*,*,#11242,.F.);
#15405=ORIENTED_EDGE('',*,*,#11243,.T.);
#15406=ORIENTED_EDGE('',*,*,#11242,.T.);
#15407=ORIENTED_EDGE('',*,*,#11244,.F.);
#15408=ORIENTED_EDGE('',*,*,#11245,.F.);
#15409=ORIENTED_EDGE('',*,*,#11246,.T.);
#15410=ORIENTED_EDGE('',*,*,#11245,.T.);
#15411=ORIENTED_EDGE('',*,*,#11247,.F.);
#15412=ORIENTED_EDGE('',*,*,#11248,.F.);
#15413=ORIENTED_EDGE('',*,*,#11249,.T.);
#15414=ORIENTED_EDGE('',*,*,#11248,.T.);
#15415=ORIENTED_EDGE('',*,*,#11250,.F.);
#15416=ORIENTED_EDGE('',*,*,#11251,.F.);
#15417=ORIENTED_EDGE('',*,*,#11252,.T.);
#15418=ORIENTED_EDGE('',*,*,#11251,.T.);
#15419=ORIENTED_EDGE('',*,*,#11253,.F.);
#15420=ORIENTED_EDGE('',*,*,#11254,.F.);
#15421=ORIENTED_EDGE('',*,*,#11255,.T.);
#15422=ORIENTED_EDGE('',*,*,#11254,.T.);
#15423=ORIENTED_EDGE('',*,*,#11256,.F.);
#15424=ORIENTED_EDGE('',*,*,#11235,.F.);
#15425=ORIENTED_EDGE('',*,*,#11257,.T.);
#15426=ORIENTED_EDGE('',*,*,#11258,.T.);
#15427=ORIENTED_EDGE('',*,*,#11259,.F.);
#15428=ORIENTED_EDGE('',*,*,#11260,.F.);
#15429=ORIENTED_EDGE('',*,*,#11261,.T.);
#15430=ORIENTED_EDGE('',*,*,#11262,.T.);
#15431=ORIENTED_EDGE('',*,*,#11263,.F.);
#15432=ORIENTED_EDGE('',*,*,#11258,.F.);
#15433=ORIENTED_EDGE('',*,*,#11264,.T.);
#15434=ORIENTED_EDGE('',*,*,#11265,.T.);
#15435=ORIENTED_EDGE('',*,*,#11266,.F.);
#15436=ORIENTED_EDGE('',*,*,#11262,.F.);
#15437=ORIENTED_EDGE('',*,*,#11267,.T.);
#15438=ORIENTED_EDGE('',*,*,#11268,.T.);
#15439=ORIENTED_EDGE('',*,*,#11269,.F.);
#15440=ORIENTED_EDGE('',*,*,#11270,.F.);
#15441=ORIENTED_EDGE('',*,*,#11271,.T.);
#15442=ORIENTED_EDGE('',*,*,#11270,.T.);
#15443=ORIENTED_EDGE('',*,*,#11272,.F.);
#15444=ORIENTED_EDGE('',*,*,#11273,.F.);
#15445=ORIENTED_EDGE('',*,*,#11274,.T.);
#15446=ORIENTED_EDGE('',*,*,#11273,.T.);
#15447=ORIENTED_EDGE('',*,*,#11275,.F.);
#15448=ORIENTED_EDGE('',*,*,#11276,.F.);
#15449=ORIENTED_EDGE('',*,*,#11277,.T.);
#15450=ORIENTED_EDGE('',*,*,#11276,.T.);
#15451=ORIENTED_EDGE('',*,*,#11278,.F.);
#15452=ORIENTED_EDGE('',*,*,#11279,.F.);
#15453=ORIENTED_EDGE('',*,*,#11280,.T.);
#15454=ORIENTED_EDGE('',*,*,#11279,.T.);
#15455=ORIENTED_EDGE('',*,*,#11281,.F.);
#15456=ORIENTED_EDGE('',*,*,#11282,.F.);
#15457=ORIENTED_EDGE('',*,*,#11283,.T.);
#15458=ORIENTED_EDGE('',*,*,#11282,.T.);
#15459=ORIENTED_EDGE('',*,*,#11284,.F.);
#15460=ORIENTED_EDGE('',*,*,#11285,.F.);
#15461=ORIENTED_EDGE('',*,*,#11286,.F.);
#15462=ORIENTED_EDGE('',*,*,#11125,.T.);
#15463=ORIENTED_EDGE('',*,*,#11287,.T.);
#15464=ORIENTED_EDGE('',*,*,#11288,.F.);
#15465=ORIENTED_EDGE('',*,*,#11289,.F.);
#15466=ORIENTED_EDGE('',*,*,#11288,.T.);
#15467=ORIENTED_EDGE('',*,*,#11290,.T.);
#15468=ORIENTED_EDGE('',*,*,#11291,.F.);
#15469=ORIENTED_EDGE('',*,*,#11292,.F.);
#15470=ORIENTED_EDGE('',*,*,#11291,.T.);
#15471=ORIENTED_EDGE('',*,*,#11293,.T.);
#15472=ORIENTED_EDGE('',*,*,#11294,.F.);
#15473=ORIENTED_EDGE('',*,*,#11295,.F.);
#15474=ORIENTED_EDGE('',*,*,#11294,.T.);
#15475=ORIENTED_EDGE('',*,*,#11296,.T.);
#15476=ORIENTED_EDGE('',*,*,#11297,.F.);
#15477=ORIENTED_EDGE('',*,*,#11298,.F.);
#15478=ORIENTED_EDGE('',*,*,#11285,.T.);
#15479=ORIENTED_EDGE('',*,*,#11299,.F.);
#15480=ORIENTED_EDGE('',*,*,#11300,.F.);
#15481=ORIENTED_EDGE('',*,*,#11301,.T.);
#15482=ORIENTED_EDGE('',*,*,#11302,.T.);
#15483=ORIENTED_EDGE('',*,*,#11303,.T.);
#15484=ORIENTED_EDGE('',*,*,#11133,.F.);
#15485=ORIENTED_EDGE('',*,*,#11304,.F.);
#15486=ORIENTED_EDGE('',*,*,#11305,.T.);
#15487=ORIENTED_EDGE('',*,*,#11306,.T.);
#15488=ORIENTED_EDGE('',*,*,#11302,.F.);
#15489=ORIENTED_EDGE('',*,*,#11307,.F.);
#15490=ORIENTED_EDGE('',*,*,#11308,.T.);
#15491=ORIENTED_EDGE('',*,*,#11309,.T.);
#15492=ORIENTED_EDGE('',*,*,#11305,.F.);
#15493=ORIENTED_EDGE('',*,*,#11310,.F.);
#15494=ORIENTED_EDGE('',*,*,#11311,.T.);
#15495=ORIENTED_EDGE('',*,*,#11312,.T.);
#15496=ORIENTED_EDGE('',*,*,#11308,.F.);
#15497=ORIENTED_EDGE('',*,*,#11313,.F.);
#15498=ORIENTED_EDGE('',*,*,#11314,.T.);
#15499=ORIENTED_EDGE('',*,*,#11315,.T.);
#15500=ORIENTED_EDGE('',*,*,#11311,.F.);
#15501=ORIENTED_EDGE('',*,*,#11316,.F.);
#15502=ORIENTED_EDGE('',*,*,#11317,.T.);
#15503=ORIENTED_EDGE('',*,*,#11318,.T.);
#15504=ORIENTED_EDGE('',*,*,#11314,.F.);
#15505=ORIENTED_EDGE('',*,*,#11319,.F.);
#15506=ORIENTED_EDGE('',*,*,#11300,.T.);
#15507=ORIENTED_EDGE('',*,*,#11320,.T.);
#15508=ORIENTED_EDGE('',*,*,#11317,.F.);
#15509=ORIENTED_EDGE('',*,*,#11321,.F.);
#15510=ORIENTED_EDGE('',*,*,#11322,.T.);
#15511=ORIENTED_EDGE('',*,*,#11323,.T.);
#15512=ORIENTED_EDGE('',*,*,#11324,.F.);
#15513=ORIENTED_EDGE('',*,*,#11325,.F.);
#15514=ORIENTED_EDGE('',*,*,#11324,.T.);
#15515=ORIENTED_EDGE('',*,*,#11326,.T.);
#15516=ORIENTED_EDGE('',*,*,#11327,.F.);
#15517=ORIENTED_EDGE('',*,*,#11328,.F.);
#15518=ORIENTED_EDGE('',*,*,#11327,.T.);
#15519=ORIENTED_EDGE('',*,*,#11329,.T.);
#15520=ORIENTED_EDGE('',*,*,#11330,.F.);
#15521=ORIENTED_EDGE('',*,*,#11331,.T.);
#15522=ORIENTED_EDGE('',*,*,#11330,.T.);
#15523=ORIENTED_EDGE('',*,*,#11332,.T.);
#15524=ORIENTED_EDGE('',*,*,#11265,.F.);
#15525=ORIENTED_EDGE('',*,*,#11333,.F.);
#15526=ORIENTED_EDGE('',*,*,#11334,.T.);
#15527=ORIENTED_EDGE('',*,*,#11335,.T.);
#15528=ORIENTED_EDGE('',*,*,#11336,.F.);
#15529=ORIENTED_EDGE('',*,*,#11337,.F.);
#15530=ORIENTED_EDGE('',*,*,#11338,.T.);
#15531=ORIENTED_EDGE('',*,*,#11339,.T.);
#15532=ORIENTED_EDGE('',*,*,#11334,.F.);
#15533=ORIENTED_EDGE('',*,*,#11340,.F.);
#15534=ORIENTED_EDGE('',*,*,#11341,.T.);
#15535=ORIENTED_EDGE('',*,*,#11342,.T.);
#15536=ORIENTED_EDGE('',*,*,#11338,.F.);
#15537=ORIENTED_EDGE('',*,*,#11343,.F.);
#15538=ORIENTED_EDGE('',*,*,#11344,.T.);
#15539=ORIENTED_EDGE('',*,*,#11345,.T.);
#15540=ORIENTED_EDGE('',*,*,#11341,.F.);
#15541=ORIENTED_EDGE('',*,*,#11346,.F.);
#15542=ORIENTED_EDGE('',*,*,#11347,.T.);
#15543=ORIENTED_EDGE('',*,*,#11348,.T.);
#15544=ORIENTED_EDGE('',*,*,#11344,.F.);
#15545=ORIENTED_EDGE('',*,*,#11349,.F.);
#15546=ORIENTED_EDGE('',*,*,#11350,.T.);
#15547=ORIENTED_EDGE('',*,*,#11351,.T.);
#15548=ORIENTED_EDGE('',*,*,#11347,.F.);
#15549=ORIENTED_EDGE('',*,*,#11352,.T.);
#15550=ORIENTED_EDGE('',*,*,#11353,.T.);
#15551=ORIENTED_EDGE('',*,*,#11354,.T.);
#15552=ORIENTED_EDGE('',*,*,#11187,.F.);
#15553=ORIENTED_EDGE('',*,*,#11355,.T.);
#15554=ORIENTED_EDGE('',*,*,#11356,.T.);
#15555=ORIENTED_EDGE('',*,*,#11357,.F.);
#15556=ORIENTED_EDGE('',*,*,#11353,.F.);
#15557=ORIENTED_EDGE('',*,*,#11358,.T.);
#15558=ORIENTED_EDGE('',*,*,#11359,.T.);
#15559=ORIENTED_EDGE('',*,*,#11360,.F.);
#15560=ORIENTED_EDGE('',*,*,#11356,.F.);
#15561=ORIENTED_EDGE('',*,*,#11361,.T.);
#15562=ORIENTED_EDGE('',*,*,#11362,.T.);
#15563=ORIENTED_EDGE('',*,*,#11363,.F.);
#15564=ORIENTED_EDGE('',*,*,#11359,.F.);
#15565=ORIENTED_EDGE('',*,*,#11364,.F.);
#15566=ORIENTED_EDGE('',*,*,#11297,.T.);
#15567=ORIENTED_EDGE('',*,*,#11365,.F.);
#15568=ORIENTED_EDGE('',*,*,#11362,.F.);
#15569=ORIENTED_EDGE('',*,*,#11366,.T.);
#15570=ORIENTED_EDGE('',*,*,#11367,.T.);
#15571=ORIENTED_EDGE('',*,*,#11368,.F.);
#15572=ORIENTED_EDGE('',*,*,#11367,.F.);
#15573=ORIENTED_EDGE('',*,*,#11369,.T.);
#15574=ORIENTED_EDGE('',*,*,#11370,.T.);
#15575=ORIENTED_EDGE('',*,*,#11371,.T.);
#15576=ORIENTED_EDGE('',*,*,#11350,.F.);
#15577=ORIENTED_EDGE('',*,*,#11372,.F.);
#15578=ORIENTED_EDGE('',*,*,#11201,.T.);
#15579=ORIENTED_EDGE('',*,*,#11373,.F.);
#15580=ORIENTED_EDGE('',*,*,#11374,.F.);
#15581=ORIENTED_EDGE('',*,*,#11375,.T.);
#15582=ORIENTED_EDGE('',*,*,#11374,.T.);
#15583=ORIENTED_EDGE('',*,*,#11376,.F.);
#15584=ORIENTED_EDGE('',*,*,#11377,.F.);
#15585=ORIENTED_EDGE('',*,*,#11378,.T.);
#15586=ORIENTED_EDGE('',*,*,#11377,.T.);
#15587=ORIENTED_EDGE('',*,*,#11379,.F.);
#15588=ORIENTED_EDGE('',*,*,#11380,.F.);
#15589=ORIENTED_EDGE('',*,*,#11381,.T.);
#15590=ORIENTED_EDGE('',*,*,#11380,.T.);
#15591=ORIENTED_EDGE('',*,*,#11382,.F.);
#15592=ORIENTED_EDGE('',*,*,#11383,.F.);
#15593=ORIENTED_EDGE('',*,*,#11384,.T.);
#15594=ORIENTED_EDGE('',*,*,#11383,.T.);
#15595=ORIENTED_EDGE('',*,*,#11385,.F.);
#15596=ORIENTED_EDGE('',*,*,#11386,.F.);
#15597=ORIENTED_EDGE('',*,*,#11387,.T.);
#15598=ORIENTED_EDGE('',*,*,#11386,.T.);
#15599=ORIENTED_EDGE('',*,*,#11388,.F.);
#15600=ORIENTED_EDGE('',*,*,#11389,.F.);
#15601=ORIENTED_EDGE('',*,*,#11390,.T.);
#15602=ORIENTED_EDGE('',*,*,#11389,.T.);
#15603=ORIENTED_EDGE('',*,*,#11391,.F.);
#15604=ORIENTED_EDGE('',*,*,#11370,.F.);
#15605=ORIENTED_EDGE('',*,*,#11392,.F.);
#15606=ORIENTED_EDGE('',*,*,#11393,.T.);
#15607=ORIENTED_EDGE('',*,*,#11394,.T.);
#15608=ORIENTED_EDGE('',*,*,#11395,.F.);
#15609=ORIENTED_EDGE('',*,*,#11396,.F.);
#15610=ORIENTED_EDGE('',*,*,#11395,.T.);
#15611=ORIENTED_EDGE('',*,*,#11397,.T.);
#15612=ORIENTED_EDGE('',*,*,#11398,.F.);
#15613=ORIENTED_EDGE('',*,*,#11399,.F.);
#15614=ORIENTED_EDGE('',*,*,#11398,.T.);
#15615=ORIENTED_EDGE('',*,*,#11400,.T.);
#15616=ORIENTED_EDGE('',*,*,#11401,.F.);
#15617=ORIENTED_EDGE('',*,*,#11402,.F.);
#15618=ORIENTED_EDGE('',*,*,#11401,.T.);
#15619=ORIENTED_EDGE('',*,*,#11403,.T.);
#15620=ORIENTED_EDGE('',*,*,#11404,.F.);
#15621=ORIENTED_EDGE('',*,*,#11405,.F.);
#15622=ORIENTED_EDGE('',*,*,#11406,.T.);
#15623=ORIENTED_EDGE('',*,*,#11407,.T.);
#15624=ORIENTED_EDGE('',*,*,#11408,.F.);
#15625=ORIENTED_EDGE('',*,*,#11409,.F.);
#15626=ORIENTED_EDGE('',*,*,#11408,.T.);
#15627=ORIENTED_EDGE('',*,*,#11410,.T.);
#15628=ORIENTED_EDGE('',*,*,#11411,.F.);
#15629=ORIENTED_EDGE('',*,*,#11412,.F.);
#15630=ORIENTED_EDGE('',*,*,#11411,.T.);
#15631=ORIENTED_EDGE('',*,*,#11413,.T.);
#15632=ORIENTED_EDGE('',*,*,#11414,.F.);
#15633=ORIENTED_EDGE('',*,*,#11415,.F.);
#15634=ORIENTED_EDGE('',*,*,#11414,.T.);
#15635=ORIENTED_EDGE('',*,*,#11416,.T.);
#15636=ORIENTED_EDGE('',*,*,#11417,.F.);
#15637=ORIENTED_EDGE('',*,*,#11418,.F.);
#15638=ORIENTED_EDGE('',*,*,#11417,.T.);
#15639=ORIENTED_EDGE('',*,*,#11419,.T.);
#15640=ORIENTED_EDGE('',*,*,#11420,.F.);
#15641=ORIENTED_EDGE('',*,*,#11421,.F.);
#15642=ORIENTED_EDGE('',*,*,#11420,.T.);
#15643=ORIENTED_EDGE('',*,*,#11422,.T.);
#15644=ORIENTED_EDGE('',*,*,#11423,.F.);
#15645=ORIENTED_EDGE('',*,*,#11424,.T.);
#15646=ORIENTED_EDGE('',*,*,#11423,.T.);
#15647=ORIENTED_EDGE('',*,*,#11425,.T.);
#15648=ORIENTED_EDGE('',*,*,#11268,.F.);
#15649=ORIENTED_EDGE('',*,*,#11426,.F.);
#15650=ORIENTED_EDGE('',*,*,#11260,.T.);
#15651=ORIENTED_EDGE('',*,*,#11427,.F.);
#15652=ORIENTED_EDGE('',*,*,#11428,.F.);
#15653=ORIENTED_EDGE('',*,*,#11429,.F.);
#15654=ORIENTED_EDGE('',*,*,#11428,.T.);
#15655=ORIENTED_EDGE('',*,*,#11430,.T.);
#15656=ORIENTED_EDGE('',*,*,#11431,.F.);
#15657=ORIENTED_EDGE('',*,*,#11432,.F.);
#15658=ORIENTED_EDGE('',*,*,#11431,.T.);
#15659=ORIENTED_EDGE('',*,*,#11433,.T.);
#15660=ORIENTED_EDGE('',*,*,#11434,.F.);
#15661=ORIENTED_EDGE('',*,*,#11435,.F.);
#15662=ORIENTED_EDGE('',*,*,#11434,.T.);
#15663=ORIENTED_EDGE('',*,*,#11436,.T.);
#15664=ORIENTED_EDGE('',*,*,#11437,.F.);
#15665=ORIENTED_EDGE('',*,*,#11438,.F.);
#15666=ORIENTED_EDGE('',*,*,#11439,.T.);
#15667=ORIENTED_EDGE('',*,*,#11440,.T.);
#15668=ORIENTED_EDGE('',*,*,#11393,.F.);
#15669=ORIENTED_EDGE('',*,*,#11441,.F.);
#15670=ORIENTED_EDGE('',*,*,#11442,.T.);
#15671=ORIENTED_EDGE('',*,*,#11443,.T.);
#15672=ORIENTED_EDGE('',*,*,#11439,.F.);
#15673=ORIENTED_EDGE('',*,*,#11444,.F.);
#15674=ORIENTED_EDGE('',*,*,#11445,.T.);
#15675=ORIENTED_EDGE('',*,*,#11446,.T.);
#15676=ORIENTED_EDGE('',*,*,#11442,.F.);
#15677=ORIENTED_EDGE('',*,*,#11447,.F.);
#15678=ORIENTED_EDGE('',*,*,#11404,.T.);
#15679=ORIENTED_EDGE('',*,*,#11448,.T.);
#15680=ORIENTED_EDGE('',*,*,#11445,.F.);
#15681=ORIENTED_EDGE('',*,*,#11449,.F.);
#15682=ORIENTED_EDGE('',*,*,#11450,.T.);
#15683=ORIENTED_EDGE('',*,*,#11451,.T.);
#15684=ORIENTED_EDGE('',*,*,#11406,.F.);
#15685=ORIENTED_EDGE('',*,*,#11452,.F.);
#15686=ORIENTED_EDGE('',*,*,#11453,.T.);
#15687=ORIENTED_EDGE('',*,*,#11454,.T.);
#15688=ORIENTED_EDGE('',*,*,#11450,.F.);
#15689=ORIENTED_EDGE('',*,*,#11455,.F.);
#15690=ORIENTED_EDGE('',*,*,#11456,.T.);
#15691=ORIENTED_EDGE('',*,*,#11457,.T.);
#15692=ORIENTED_EDGE('',*,*,#11453,.F.);
#15693=ORIENTED_EDGE('',*,*,#11458,.F.);
#15694=ORIENTED_EDGE('',*,*,#11459,.T.);
#15695=ORIENTED_EDGE('',*,*,#11460,.T.);
#15696=ORIENTED_EDGE('',*,*,#11456,.F.);
#15697=ORIENTED_EDGE('',*,*,#11461,.F.);
#15698=ORIENTED_EDGE('',*,*,#11462,.T.);
#15699=ORIENTED_EDGE('',*,*,#11463,.T.);
#15700=ORIENTED_EDGE('',*,*,#11459,.F.);
#15701=ORIENTED_EDGE('',*,*,#11464,.F.);
#15702=ORIENTED_EDGE('',*,*,#11465,.T.);
#15703=ORIENTED_EDGE('',*,*,#11466,.T.);
#15704=ORIENTED_EDGE('',*,*,#11462,.F.);
#15705=ORIENTED_EDGE('',*,*,#11467,.F.);
#15706=ORIENTED_EDGE('',*,*,#11468,.T.);
#15707=ORIENTED_EDGE('',*,*,#11469,.T.);
#15708=ORIENTED_EDGE('',*,*,#11465,.F.);
#15709=ORIENTED_EDGE('',*,*,#11470,.F.);
#15710=ORIENTED_EDGE('',*,*,#11471,.T.);
#15711=ORIENTED_EDGE('',*,*,#11472,.T.);
#15712=ORIENTED_EDGE('',*,*,#11468,.F.);
#15713=ORIENTED_EDGE('',*,*,#11473,.F.);
#15714=ORIENTED_EDGE('',*,*,#11474,.T.);
#15715=ORIENTED_EDGE('',*,*,#11475,.T.);
#15716=ORIENTED_EDGE('',*,*,#11471,.F.);
#15717=ORIENTED_EDGE('',*,*,#11476,.F.);
#15718=ORIENTED_EDGE('',*,*,#11477,.T.);
#15719=ORIENTED_EDGE('',*,*,#11478,.T.);
#15720=ORIENTED_EDGE('',*,*,#11474,.F.);
#15721=ORIENTED_EDGE('',*,*,#11479,.F.);
#15722=ORIENTED_EDGE('',*,*,#11480,.T.);
#15723=ORIENTED_EDGE('',*,*,#11481,.T.);
#15724=ORIENTED_EDGE('',*,*,#11477,.F.);
#15725=ORIENTED_EDGE('',*,*,#11482,.F.);
#15726=ORIENTED_EDGE('',*,*,#11483,.T.);
#15727=ORIENTED_EDGE('',*,*,#11484,.T.);
#15728=ORIENTED_EDGE('',*,*,#11480,.F.);
#15729=ORIENTED_EDGE('',*,*,#11485,.F.);
#15730=ORIENTED_EDGE('',*,*,#11486,.T.);
#15731=ORIENTED_EDGE('',*,*,#11487,.T.);
#15732=ORIENTED_EDGE('',*,*,#11483,.F.);
#15733=ORIENTED_EDGE('',*,*,#11488,.F.);
#15734=ORIENTED_EDGE('',*,*,#11489,.T.);
#15735=ORIENTED_EDGE('',*,*,#11490,.T.);
#15736=ORIENTED_EDGE('',*,*,#11486,.F.);
#15737=ORIENTED_EDGE('',*,*,#11491,.F.);
#15738=ORIENTED_EDGE('',*,*,#11492,.T.);
#15739=ORIENTED_EDGE('',*,*,#11493,.T.);
#15740=ORIENTED_EDGE('',*,*,#11489,.F.);
#15741=ORIENTED_EDGE('',*,*,#11494,.F.);
#15742=ORIENTED_EDGE('',*,*,#11495,.T.);
#15743=ORIENTED_EDGE('',*,*,#11496,.T.);
#15744=ORIENTED_EDGE('',*,*,#11492,.F.);
#15745=ORIENTED_EDGE('',*,*,#11166,.F.);
#15746=ORIENTED_EDGE('',*,*,#10788,.F.);
#15747=ORIENTED_EDGE('',*,*,#10792,.F.);
#15748=ORIENTED_EDGE('',*,*,#10795,.F.);
#15749=ORIENTED_EDGE('',*,*,#10798,.F.);
#15750=ORIENTED_EDGE('',*,*,#10801,.F.);
#15751=ORIENTED_EDGE('',*,*,#10804,.F.);
#15752=ORIENTED_EDGE('',*,*,#10817,.T.);
#15753=ORIENTED_EDGE('',*,*,#10836,.T.);
#15754=ORIENTED_EDGE('',*,*,#10833,.T.);
#15755=ORIENTED_EDGE('',*,*,#10830,.T.);
#15756=ORIENTED_EDGE('',*,*,#10827,.T.);
#15757=ORIENTED_EDGE('',*,*,#10824,.T.);
#15758=ORIENTED_EDGE('',*,*,#10820,.T.);
#15759=ORIENTED_EDGE('',*,*,#11042,.T.);
#15760=ORIENTED_EDGE('',*,*,#11039,.F.);
#15761=ORIENTED_EDGE('',*,*,#11036,.F.);
#15762=ORIENTED_EDGE('',*,*,#11033,.F.);
#15763=ORIENTED_EDGE('',*,*,#11030,.F.);
#15764=ORIENTED_EDGE('',*,*,#11027,.F.);
#15765=ORIENTED_EDGE('',*,*,#11023,.F.);
#15766=ORIENTED_EDGE('',*,*,#11075,.F.);
#15767=ORIENTED_EDGE('',*,*,#11078,.F.);
#15768=ORIENTED_EDGE('',*,*,#11081,.F.);
#15769=ORIENTED_EDGE('',*,*,#11084,.F.);
#15770=ORIENTED_EDGE('',*,*,#11087,.F.);
#15771=ORIENTED_EDGE('',*,*,#11090,.F.);
#15772=ORIENTED_EDGE('',*,*,#11093,.F.);
#15773=ORIENTED_EDGE('',*,*,#11096,.F.);
#15774=ORIENTED_EDGE('',*,*,#11099,.F.);
#15775=ORIENTED_EDGE('',*,*,#11102,.F.);
#15776=ORIENTED_EDGE('',*,*,#11105,.F.);
#15777=ORIENTED_EDGE('',*,*,#11108,.F.);
#15778=ORIENTED_EDGE('',*,*,#11111,.F.);
#15779=ORIENTED_EDGE('',*,*,#11114,.F.);
#15780=ORIENTED_EDGE('',*,*,#11117,.F.);
#15781=ORIENTED_EDGE('',*,*,#11120,.F.);
#15782=ORIENTED_EDGE('',*,*,#11061,.F.);
#15783=ORIENTED_EDGE('',*,*,#11007,.T.);
#15784=ORIENTED_EDGE('',*,*,#11004,.T.);
#15785=ORIENTED_EDGE('',*,*,#11001,.T.);
#15786=ORIENTED_EDGE('',*,*,#10998,.T.);
#15787=ORIENTED_EDGE('',*,*,#10995,.T.);
#15788=ORIENTED_EDGE('',*,*,#10992,.T.);
#15789=ORIENTED_EDGE('',*,*,#10989,.T.);
#15790=ORIENTED_EDGE('',*,*,#10986,.T.);
#15791=ORIENTED_EDGE('',*,*,#10983,.T.);
#15792=ORIENTED_EDGE('',*,*,#10980,.T.);
#15793=ORIENTED_EDGE('',*,*,#10977,.T.);
#15794=ORIENTED_EDGE('',*,*,#10974,.T.);
#15795=ORIENTED_EDGE('',*,*,#10971,.T.);
#15796=ORIENTED_EDGE('',*,*,#10968,.T.);
#15797=ORIENTED_EDGE('',*,*,#10965,.T.);
#15798=ORIENTED_EDGE('',*,*,#10962,.T.);
#15799=ORIENTED_EDGE('',*,*,#10918,.T.);
#15800=ORIENTED_EDGE('',*,*,#10922,.T.);
#15801=ORIENTED_EDGE('',*,*,#10925,.T.);
#15802=ORIENTED_EDGE('',*,*,#10928,.T.);
#15803=ORIENTED_EDGE('',*,*,#10931,.T.);
#15804=ORIENTED_EDGE('',*,*,#10934,.T.);
#15805=ORIENTED_EDGE('',*,*,#10937,.F.);
#15806=ORIENTED_EDGE('',*,*,#10887,.F.);
#15807=ORIENTED_EDGE('',*,*,#10891,.F.);
#15808=ORIENTED_EDGE('',*,*,#10894,.F.);
#15809=ORIENTED_EDGE('',*,*,#10897,.F.);
#15810=ORIENTED_EDGE('',*,*,#10900,.F.);
#15811=ORIENTED_EDGE('',*,*,#10903,.F.);
#15812=ORIENTED_EDGE('',*,*,#10884,.F.);
#15813=ORIENTED_EDGE('',*,*,#10866,.T.);
#15814=ORIENTED_EDGE('',*,*,#10863,.T.);
#15815=ORIENTED_EDGE('',*,*,#10860,.T.);
#15816=ORIENTED_EDGE('',*,*,#10857,.T.);
#15817=ORIENTED_EDGE('',*,*,#10854,.T.);
#15818=ORIENTED_EDGE('',*,*,#10850,.T.);
#15819=ORIENTED_EDGE('',*,*,#11237,.T.);
#15820=ORIENTED_EDGE('',*,*,#11240,.F.);
#15821=ORIENTED_EDGE('',*,*,#11243,.F.);
#15822=ORIENTED_EDGE('',*,*,#11246,.F.);
#15823=ORIENTED_EDGE('',*,*,#11249,.F.);
#15824=ORIENTED_EDGE('',*,*,#11252,.F.);
#15825=ORIENTED_EDGE('',*,*,#11255,.F.);
#15826=ORIENTED_EDGE('',*,*,#11234,.F.);
#15827=ORIENTED_EDGE('',*,*,#11214,.T.);
#15828=ORIENTED_EDGE('',*,*,#11211,.T.);
#15829=ORIENTED_EDGE('',*,*,#11208,.T.);
#15830=ORIENTED_EDGE('',*,*,#11205,.T.);
#15831=ORIENTED_EDGE('',*,*,#11202,.T.);
#15832=ORIENTED_EDGE('',*,*,#11198,.T.);
#15833=ORIENTED_EDGE('',*,*,#11372,.T.);
#15834=ORIENTED_EDGE('',*,*,#11375,.F.);
#15835=ORIENTED_EDGE('',*,*,#11378,.F.);
#15836=ORIENTED_EDGE('',*,*,#11381,.F.);
#15837=ORIENTED_EDGE('',*,*,#11384,.F.);
#15838=ORIENTED_EDGE('',*,*,#11387,.F.);
#15839=ORIENTED_EDGE('',*,*,#11390,.F.);
#15840=ORIENTED_EDGE('',*,*,#11369,.F.);
#15841=ORIENTED_EDGE('',*,*,#11349,.T.);
#15842=ORIENTED_EDGE('',*,*,#11346,.T.);
#15843=ORIENTED_EDGE('',*,*,#11343,.T.);
#15844=ORIENTED_EDGE('',*,*,#11340,.T.);
#15845=ORIENTED_EDGE('',*,*,#11337,.T.);
#15846=ORIENTED_EDGE('',*,*,#11333,.T.);
#15847=ORIENTED_EDGE('',*,*,#11497,.T.);
#15848=ORIENTED_EDGE('',*,*,#11498,.F.);
#15849=ORIENTED_EDGE('',*,*,#11499,.F.);
#15850=ORIENTED_EDGE('',*,*,#11500,.F.);
#15851=ORIENTED_EDGE('',*,*,#11501,.F.);
#15852=ORIENTED_EDGE('',*,*,#11502,.F.);
#15853=ORIENTED_EDGE('',*,*,#11503,.F.);
#15854=ORIENTED_EDGE('',*,*,#11504,.F.);
#15855=ORIENTED_EDGE('',*,*,#11505,.F.);
#15856=ORIENTED_EDGE('',*,*,#11506,.F.);
#15857=ORIENTED_EDGE('',*,*,#11507,.F.);
#15858=ORIENTED_EDGE('',*,*,#11508,.F.);
#15859=ORIENTED_EDGE('',*,*,#11509,.F.);
#15860=ORIENTED_EDGE('',*,*,#11510,.F.);
#15861=ORIENTED_EDGE('',*,*,#11511,.F.);
#15862=ORIENTED_EDGE('',*,*,#11512,.F.);
#15863=ORIENTED_EDGE('',*,*,#11513,.F.);
#15864=ORIENTED_EDGE('',*,*,#11514,.F.);
#15865=ORIENTED_EDGE('',*,*,#11515,.F.);
#15866=ORIENTED_EDGE('',*,*,#11516,.F.);
#15867=ORIENTED_EDGE('',*,*,#11517,.F.);
#15868=ORIENTED_EDGE('',*,*,#11518,.F.);
#15869=ORIENTED_EDGE('',*,*,#11519,.F.);
#15870=ORIENTED_EDGE('',*,*,#11520,.F.);
#15871=ORIENTED_EDGE('',*,*,#11494,.T.);
#15872=ORIENTED_EDGE('',*,*,#11491,.T.);
#15873=ORIENTED_EDGE('',*,*,#11488,.T.);
#15874=ORIENTED_EDGE('',*,*,#11485,.T.);
#15875=ORIENTED_EDGE('',*,*,#11482,.T.);
#15876=ORIENTED_EDGE('',*,*,#11479,.T.);
#15877=ORIENTED_EDGE('',*,*,#11476,.T.);
#15878=ORIENTED_EDGE('',*,*,#11473,.T.);
#15879=ORIENTED_EDGE('',*,*,#11470,.T.);
#15880=ORIENTED_EDGE('',*,*,#11467,.T.);
#15881=ORIENTED_EDGE('',*,*,#11464,.T.);
#15882=ORIENTED_EDGE('',*,*,#11461,.T.);
#15883=ORIENTED_EDGE('',*,*,#11458,.T.);
#15884=ORIENTED_EDGE('',*,*,#11455,.T.);
#15885=ORIENTED_EDGE('',*,*,#11452,.T.);
#15886=ORIENTED_EDGE('',*,*,#11449,.T.);
#15887=ORIENTED_EDGE('',*,*,#11405,.T.);
#15888=ORIENTED_EDGE('',*,*,#11409,.T.);
#15889=ORIENTED_EDGE('',*,*,#11412,.T.);
#15890=ORIENTED_EDGE('',*,*,#11415,.T.);
#15891=ORIENTED_EDGE('',*,*,#11418,.T.);
#15892=ORIENTED_EDGE('',*,*,#11421,.T.);
#15893=ORIENTED_EDGE('',*,*,#11424,.F.);
#15894=ORIENTED_EDGE('',*,*,#11267,.F.);
#15895=ORIENTED_EDGE('',*,*,#11271,.F.);
#15896=ORIENTED_EDGE('',*,*,#11274,.F.);
#15897=ORIENTED_EDGE('',*,*,#11277,.F.);
#15898=ORIENTED_EDGE('',*,*,#11280,.F.);
#15899=ORIENTED_EDGE('',*,*,#11283,.F.);
#15900=ORIENTED_EDGE('',*,*,#11298,.T.);
#15901=ORIENTED_EDGE('',*,*,#11319,.T.);
#15902=ORIENTED_EDGE('',*,*,#11316,.T.);
#15903=ORIENTED_EDGE('',*,*,#11313,.T.);
#15904=ORIENTED_EDGE('',*,*,#11310,.T.);
#15905=ORIENTED_EDGE('',*,*,#11307,.T.);
#15906=ORIENTED_EDGE('',*,*,#11304,.T.);
#15907=ORIENTED_EDGE('',*,*,#11301,.F.);
#15908=ORIENTED_EDGE('',*,*,#11132,.F.);
#15909=ORIENTED_EDGE('',*,*,#11136,.F.);
#15910=ORIENTED_EDGE('',*,*,#11139,.F.);
#15911=ORIENTED_EDGE('',*,*,#11142,.F.);
#15912=ORIENTED_EDGE('',*,*,#11145,.F.);
#15913=ORIENTED_EDGE('',*,*,#11148,.F.);
#15914=ORIENTED_EDGE('',*,*,#11163,.T.);
#15915=ORIENTED_EDGE('',*,*,#11184,.T.);
#15916=ORIENTED_EDGE('',*,*,#11181,.T.);
#15917=ORIENTED_EDGE('',*,*,#11178,.T.);
#15918=ORIENTED_EDGE('',*,*,#11175,.T.);
#15919=ORIENTED_EDGE('',*,*,#11172,.T.);
#15920=ORIENTED_EDGE('',*,*,#11169,.T.);
#15921=ORIENTED_EDGE('',*,*,#11151,.T.);
#15922=ORIENTED_EDGE('',*,*,#11154,.T.);
#15923=ORIENTED_EDGE('',*,*,#11157,.T.);
#15924=ORIENTED_EDGE('',*,*,#11160,.T.);
#15925=ORIENTED_EDGE('',*,*,#11229,.T.);
#15926=ORIENTED_EDGE('',*,*,#11226,.F.);
#15927=ORIENTED_EDGE('',*,*,#11223,.F.);
#15928=ORIENTED_EDGE('',*,*,#11220,.F.);
#15929=ORIENTED_EDGE('',*,*,#11217,.F.);
#15930=ORIENTED_EDGE('',*,*,#10838,.T.);
#15931=ORIENTED_EDGE('',*,*,#10842,.T.);
#15932=ORIENTED_EDGE('',*,*,#10845,.T.);
#15933=ORIENTED_EDGE('',*,*,#10848,.F.);
#15934=ORIENTED_EDGE('',*,*,#10785,.F.);
#15935=ORIENTED_EDGE('',*,*,#10782,.F.);
#15936=ORIENTED_EDGE('',*,*,#10778,.F.);
#15937=ORIENTED_EDGE('',*,*,#11060,.T.);
#15938=ORIENTED_EDGE('',*,*,#11020,.F.);
#15939=ORIENTED_EDGE('',*,*,#11017,.F.);
#15940=ORIENTED_EDGE('',*,*,#11014,.F.);
#15941=ORIENTED_EDGE('',*,*,#11010,.F.);
#15942=ORIENTED_EDGE('',*,*,#11064,.F.);
#15943=ORIENTED_EDGE('',*,*,#11067,.F.);
#15944=ORIENTED_EDGE('',*,*,#11070,.F.);
#15945=ORIENTED_EDGE('',*,*,#11073,.F.);
#15946=ORIENTED_EDGE('',*,*,#10915,.T.);
#15947=ORIENTED_EDGE('',*,*,#10960,.T.);
#15948=ORIENTED_EDGE('',*,*,#10957,.T.);
#15949=ORIENTED_EDGE('',*,*,#10954,.T.);
#15950=ORIENTED_EDGE('',*,*,#10951,.T.);
#15951=ORIENTED_EDGE('',*,*,#10905,.T.);
#15952=ORIENTED_EDGE('',*,*,#10909,.T.);
#15953=ORIENTED_EDGE('',*,*,#10912,.T.);
#15954=ORIENTED_EDGE('',*,*,#11044,.F.);
#15955=ORIENTED_EDGE('',*,*,#10807,.T.);
#15956=ORIENTED_EDGE('',*,*,#10811,.T.);
#15957=ORIENTED_EDGE('',*,*,#10814,.T.);
#15958=ORIENTED_EDGE('',*,*,#10879,.T.);
#15959=ORIENTED_EDGE('',*,*,#10876,.F.);
#15960=ORIENTED_EDGE('',*,*,#10873,.F.);
#15961=ORIENTED_EDGE('',*,*,#10869,.F.);
#15962=ORIENTED_EDGE('',*,*,#10939,.T.);
#15963=ORIENTED_EDGE('',*,*,#10942,.T.);
#15964=ORIENTED_EDGE('',*,*,#10945,.T.);
#15965=ORIENTED_EDGE('',*,*,#10948,.T.);
#15966=ORIENTED_EDGE('',*,*,#11056,.T.);
#15967=ORIENTED_EDGE('',*,*,#11053,.F.);
#15968=ORIENTED_EDGE('',*,*,#11050,.F.);
#15969=ORIENTED_EDGE('',*,*,#11047,.F.);
#15970=ORIENTED_EDGE('',*,*,#10883,.T.);
#15971=ORIENTED_EDGE('',*,*,#11286,.T.);
#15972=ORIENTED_EDGE('',*,*,#11289,.T.);
#15973=ORIENTED_EDGE('',*,*,#11292,.T.);
#15974=ORIENTED_EDGE('',*,*,#11295,.T.);
#15975=ORIENTED_EDGE('',*,*,#11364,.T.);
#15976=ORIENTED_EDGE('',*,*,#11361,.F.);
#15977=ORIENTED_EDGE('',*,*,#11358,.F.);
#15978=ORIENTED_EDGE('',*,*,#11355,.F.);
#15979=ORIENTED_EDGE('',*,*,#11352,.F.);
#15980=ORIENTED_EDGE('',*,*,#11186,.T.);
#15981=ORIENTED_EDGE('',*,*,#11190,.T.);
#15982=ORIENTED_EDGE('',*,*,#11193,.T.);
#15983=ORIENTED_EDGE('',*,*,#11196,.F.);
#15984=ORIENTED_EDGE('',*,*,#11129,.F.);
#15985=ORIENTED_EDGE('',*,*,#11126,.F.);
#15986=ORIENTED_EDGE('',*,*,#11122,.F.);
#15987=ORIENTED_EDGE('',*,*,#11233,.T.);
#15988=ORIENTED_EDGE('',*,*,#11426,.T.);
#15989=ORIENTED_EDGE('',*,*,#11429,.T.);
#15990=ORIENTED_EDGE('',*,*,#11432,.T.);
#15991=ORIENTED_EDGE('',*,*,#11435,.T.);
#15992=ORIENTED_EDGE('',*,*,#11521,.T.);
#15993=ORIENTED_EDGE('',*,*,#11522,.F.);
#15994=ORIENTED_EDGE('',*,*,#11523,.F.);
#15995=ORIENTED_EDGE('',*,*,#11524,.F.);
#15996=ORIENTED_EDGE('',*,*,#11525,.F.);
#15997=ORIENTED_EDGE('',*,*,#11321,.T.);
#15998=ORIENTED_EDGE('',*,*,#11325,.T.);
#15999=ORIENTED_EDGE('',*,*,#11328,.T.);
#16000=ORIENTED_EDGE('',*,*,#11331,.F.);
#16001=ORIENTED_EDGE('',*,*,#11264,.F.);
#16002=ORIENTED_EDGE('',*,*,#11261,.F.);
#16003=ORIENTED_EDGE('',*,*,#11257,.F.);
#16004=ORIENTED_EDGE('',*,*,#11368,.T.);
#16005=ORIENTED_EDGE('',*,*,#11402,.T.);
#16006=ORIENTED_EDGE('',*,*,#11447,.T.);
#16007=ORIENTED_EDGE('',*,*,#11444,.T.);
#16008=ORIENTED_EDGE('',*,*,#11441,.T.);
#16009=ORIENTED_EDGE('',*,*,#11438,.T.);
#16010=ORIENTED_EDGE('',*,*,#11392,.T.);
#16011=ORIENTED_EDGE('',*,*,#11396,.T.);
#16012=ORIENTED_EDGE('',*,*,#11399,.T.);
#16013=ORIENTED_EDGE('',*,*,#11526,.F.);
#16014=ORIENTED_EDGE('',*,*,#11527,.F.);
#16015=ORIENTED_EDGE('',*,*,#11528,.F.);
#16016=ORIENTED_EDGE('',*,*,#11529,.F.);
#16017=ORIENTED_EDGE('',*,*,#11530,.F.);
#16018=ORIENTED_EDGE('',*,*,#11531,.F.);
#16019=ORIENTED_EDGE('',*,*,#11532,.F.);
#16020=ORIENTED_EDGE('',*,*,#11533,.F.);
#16021=ORIENTED_EDGE('',*,*,#11534,.T.);
#16022=ORIENTED_EDGE('',*,*,#11529,.T.);
#16023=ORIENTED_EDGE('',*,*,#11535,.T.);
#16024=ORIENTED_EDGE('',*,*,#11536,.F.);
#16025=ORIENTED_EDGE('',*,*,#11537,.F.);
#16026=ORIENTED_EDGE('',*,*,#11528,.T.);
#16027=ORIENTED_EDGE('',*,*,#11538,.T.);
#16028=ORIENTED_EDGE('',*,*,#11539,.F.);
#16029=ORIENTED_EDGE('',*,*,#11535,.F.);
#16030=ORIENTED_EDGE('',*,*,#11527,.T.);
#16031=ORIENTED_EDGE('',*,*,#11540,.T.);
#16032=ORIENTED_EDGE('',*,*,#11541,.F.);
#16033=ORIENTED_EDGE('',*,*,#11538,.F.);
#16034=ORIENTED_EDGE('',*,*,#11526,.T.);
#16035=ORIENTED_EDGE('',*,*,#11542,.T.);
#16036=ORIENTED_EDGE('',*,*,#11543,.F.);
#16037=ORIENTED_EDGE('',*,*,#11540,.F.);
#16038=ORIENTED_EDGE('',*,*,#11503,.T.);
#16039=ORIENTED_EDGE('',*,*,#11544,.T.);
#16040=ORIENTED_EDGE('',*,*,#11545,.F.);
#16041=ORIENTED_EDGE('',*,*,#11546,.F.);
#16042=ORIENTED_EDGE('',*,*,#11502,.T.);
#16043=ORIENTED_EDGE('',*,*,#11547,.T.);
#16044=ORIENTED_EDGE('',*,*,#11548,.F.);
#16045=ORIENTED_EDGE('',*,*,#11544,.F.);
#16046=ORIENTED_EDGE('',*,*,#11501,.T.);
#16047=ORIENTED_EDGE('',*,*,#11549,.T.);
#16048=ORIENTED_EDGE('',*,*,#11550,.F.);
#16049=ORIENTED_EDGE('',*,*,#11547,.F.);
#16050=ORIENTED_EDGE('',*,*,#11500,.T.);
#16051=ORIENTED_EDGE('',*,*,#11551,.T.);
#16052=ORIENTED_EDGE('',*,*,#11552,.F.);
#16053=ORIENTED_EDGE('',*,*,#11549,.F.);
#16054=ORIENTED_EDGE('',*,*,#11499,.T.);
#16055=ORIENTED_EDGE('',*,*,#11553,.T.);
#16056=ORIENTED_EDGE('',*,*,#11554,.F.);
#16057=ORIENTED_EDGE('',*,*,#11551,.F.);
#16058=ORIENTED_EDGE('',*,*,#11498,.T.);
#16059=ORIENTED_EDGE('',*,*,#11555,.T.);
#16060=ORIENTED_EDGE('',*,*,#11556,.F.);
#16061=ORIENTED_EDGE('',*,*,#11553,.F.);
#16062=ORIENTED_EDGE('',*,*,#11497,.F.);
#16063=ORIENTED_EDGE('',*,*,#11336,.T.);
#16064=ORIENTED_EDGE('',*,*,#11557,.F.);
#16065=ORIENTED_EDGE('',*,*,#11555,.F.);
#16066=ORIENTED_EDGE('',*,*,#11525,.T.);
#16067=ORIENTED_EDGE('',*,*,#11558,.T.);
#16068=ORIENTED_EDGE('',*,*,#11559,.T.);
#16069=ORIENTED_EDGE('',*,*,#11322,.F.);
#16070=ORIENTED_EDGE('',*,*,#11524,.T.);
#16071=ORIENTED_EDGE('',*,*,#11560,.T.);
#16072=ORIENTED_EDGE('',*,*,#11561,.F.);
#16073=ORIENTED_EDGE('',*,*,#11558,.F.);
#16074=ORIENTED_EDGE('',*,*,#11523,.T.);
#16075=ORIENTED_EDGE('',*,*,#11562,.T.);
#16076=ORIENTED_EDGE('',*,*,#11563,.F.);
#16077=ORIENTED_EDGE('',*,*,#11560,.F.);
#16078=ORIENTED_EDGE('',*,*,#11522,.T.);
#16079=ORIENTED_EDGE('',*,*,#11564,.T.);
#16080=ORIENTED_EDGE('',*,*,#11565,.F.);
#16081=ORIENTED_EDGE('',*,*,#11562,.F.);
#16082=ORIENTED_EDGE('',*,*,#11521,.F.);
#16083=ORIENTED_EDGE('',*,*,#11437,.T.);
#16084=ORIENTED_EDGE('',*,*,#11566,.F.);
#16085=ORIENTED_EDGE('',*,*,#11564,.F.);
#16086=ORIENTED_EDGE('',*,*,#11567,.F.);
#16087=ORIENTED_EDGE('',*,*,#11568,.T.);
#16088=ORIENTED_EDGE('',*,*,#11534,.F.);
#16089=ORIENTED_EDGE('',*,*,#11568,.F.);
#16090=ORIENTED_EDGE('',*,*,#11520,.T.);
#16091=ORIENTED_EDGE('',*,*,#11569,.T.);
#16092=ORIENTED_EDGE('',*,*,#11570,.T.);
#16093=ORIENTED_EDGE('',*,*,#11495,.F.);
#16094=ORIENTED_EDGE('',*,*,#11530,.T.);
#16095=ORIENTED_EDGE('',*,*,#11537,.T.);
#16096=ORIENTED_EDGE('',*,*,#11571,.F.);
#16097=ORIENTED_EDGE('',*,*,#11572,.F.);
#16098=ORIENTED_EDGE('',*,*,#11531,.T.);
#16099=ORIENTED_EDGE('',*,*,#11572,.T.);
#16100=ORIENTED_EDGE('',*,*,#11573,.F.);
#16101=ORIENTED_EDGE('',*,*,#11574,.F.);
#16102=ORIENTED_EDGE('',*,*,#11532,.T.);
#16103=ORIENTED_EDGE('',*,*,#11574,.T.);
#16104=ORIENTED_EDGE('',*,*,#11575,.F.);
#16105=ORIENTED_EDGE('',*,*,#11576,.F.);
#16106=ORIENTED_EDGE('',*,*,#11533,.T.);
#16107=ORIENTED_EDGE('',*,*,#11576,.T.);
#16108=ORIENTED_EDGE('',*,*,#11577,.F.);
#16109=ORIENTED_EDGE('',*,*,#11542,.F.);
#16110=ORIENTED_EDGE('',*,*,#11504,.T.);
#16111=ORIENTED_EDGE('',*,*,#11546,.T.);
#16112=ORIENTED_EDGE('',*,*,#11578,.F.);
#16113=ORIENTED_EDGE('',*,*,#11579,.F.);
#16114=ORIENTED_EDGE('',*,*,#11505,.T.);
#16115=ORIENTED_EDGE('',*,*,#11579,.T.);
#16116=ORIENTED_EDGE('',*,*,#11580,.F.);
#16117=ORIENTED_EDGE('',*,*,#11581,.F.);
#16118=ORIENTED_EDGE('',*,*,#11506,.T.);
#16119=ORIENTED_EDGE('',*,*,#11581,.T.);
#16120=ORIENTED_EDGE('',*,*,#11582,.F.);
#16121=ORIENTED_EDGE('',*,*,#11583,.F.);
#16122=ORIENTED_EDGE('',*,*,#11507,.T.);
#16123=ORIENTED_EDGE('',*,*,#11583,.T.);
#16124=ORIENTED_EDGE('',*,*,#11584,.F.);
#16125=ORIENTED_EDGE('',*,*,#11585,.F.);
#16126=ORIENTED_EDGE('',*,*,#11508,.T.);
#16127=ORIENTED_EDGE('',*,*,#11585,.T.);
#16128=ORIENTED_EDGE('',*,*,#11586,.F.);
#16129=ORIENTED_EDGE('',*,*,#11587,.F.);
#16130=ORIENTED_EDGE('',*,*,#11509,.T.);
#16131=ORIENTED_EDGE('',*,*,#11587,.T.);
#16132=ORIENTED_EDGE('',*,*,#11588,.F.);
#16133=ORIENTED_EDGE('',*,*,#11589,.F.);
#16134=ORIENTED_EDGE('',*,*,#11510,.T.);
#16135=ORIENTED_EDGE('',*,*,#11589,.T.);
#16136=ORIENTED_EDGE('',*,*,#11590,.F.);
#16137=ORIENTED_EDGE('',*,*,#11591,.F.);
#16138=ORIENTED_EDGE('',*,*,#11511,.T.);
#16139=ORIENTED_EDGE('',*,*,#11591,.T.);
#16140=ORIENTED_EDGE('',*,*,#11592,.F.);
#16141=ORIENTED_EDGE('',*,*,#11593,.F.);
#16142=ORIENTED_EDGE('',*,*,#11512,.T.);
#16143=ORIENTED_EDGE('',*,*,#11593,.T.);
#16144=ORIENTED_EDGE('',*,*,#11594,.F.);
#16145=ORIENTED_EDGE('',*,*,#11595,.F.);
#16146=ORIENTED_EDGE('',*,*,#11513,.T.);
#16147=ORIENTED_EDGE('',*,*,#11595,.T.);
#16148=ORIENTED_EDGE('',*,*,#11596,.F.);
#16149=ORIENTED_EDGE('',*,*,#11597,.F.);
#16150=ORIENTED_EDGE('',*,*,#11514,.T.);
#16151=ORIENTED_EDGE('',*,*,#11597,.T.);
#16152=ORIENTED_EDGE('',*,*,#11598,.F.);
#16153=ORIENTED_EDGE('',*,*,#11599,.F.);
#16154=ORIENTED_EDGE('',*,*,#11515,.T.);
#16155=ORIENTED_EDGE('',*,*,#11599,.T.);
#16156=ORIENTED_EDGE('',*,*,#11600,.F.);
#16157=ORIENTED_EDGE('',*,*,#11601,.F.);
#16158=ORIENTED_EDGE('',*,*,#11516,.T.);
#16159=ORIENTED_EDGE('',*,*,#11601,.T.);
#16160=ORIENTED_EDGE('',*,*,#11602,.F.);
#16161=ORIENTED_EDGE('',*,*,#11603,.F.);
#16162=ORIENTED_EDGE('',*,*,#11517,.T.);
#16163=ORIENTED_EDGE('',*,*,#11603,.T.);
#16164=ORIENTED_EDGE('',*,*,#11604,.F.);
#16165=ORIENTED_EDGE('',*,*,#11605,.F.);
#16166=ORIENTED_EDGE('',*,*,#11518,.T.);
#16167=ORIENTED_EDGE('',*,*,#11605,.T.);
#16168=ORIENTED_EDGE('',*,*,#11606,.F.);
#16169=ORIENTED_EDGE('',*,*,#11607,.F.);
#16170=ORIENTED_EDGE('',*,*,#11519,.T.);
#16171=ORIENTED_EDGE('',*,*,#11607,.T.);
#16172=ORIENTED_EDGE('',*,*,#11608,.F.);
#16173=ORIENTED_EDGE('',*,*,#11569,.F.);
#16174=ORIENTED_EDGE('',*,*,#11168,.F.);
#16175=ORIENTED_EDGE('',*,*,#11171,.F.);
#16176=ORIENTED_EDGE('',*,*,#11174,.F.);
#16177=ORIENTED_EDGE('',*,*,#11177,.F.);
#16178=ORIENTED_EDGE('',*,*,#11180,.F.);
#16179=ORIENTED_EDGE('',*,*,#11183,.F.);
#16180=ORIENTED_EDGE('',*,*,#11185,.F.);
#16181=ORIENTED_EDGE('',*,*,#11164,.T.);
#16182=ORIENTED_EDGE('',*,*,#11149,.T.);
#16183=ORIENTED_EDGE('',*,*,#11146,.T.);
#16184=ORIENTED_EDGE('',*,*,#11143,.T.);
#16185=ORIENTED_EDGE('',*,*,#11140,.T.);
#16186=ORIENTED_EDGE('',*,*,#11137,.T.);
#16187=ORIENTED_EDGE('',*,*,#11134,.T.);
#16188=ORIENTED_EDGE('',*,*,#11303,.F.);
#16189=ORIENTED_EDGE('',*,*,#11306,.F.);
#16190=ORIENTED_EDGE('',*,*,#11309,.F.);
#16191=ORIENTED_EDGE('',*,*,#11312,.F.);
#16192=ORIENTED_EDGE('',*,*,#11315,.F.);
#16193=ORIENTED_EDGE('',*,*,#11318,.F.);
#16194=ORIENTED_EDGE('',*,*,#11320,.F.);
#16195=ORIENTED_EDGE('',*,*,#11299,.T.);
#16196=ORIENTED_EDGE('',*,*,#11284,.T.);
#16197=ORIENTED_EDGE('',*,*,#11281,.T.);
#16198=ORIENTED_EDGE('',*,*,#11278,.T.);
#16199=ORIENTED_EDGE('',*,*,#11275,.T.);
#16200=ORIENTED_EDGE('',*,*,#11272,.T.);
#16201=ORIENTED_EDGE('',*,*,#11269,.T.);
#16202=ORIENTED_EDGE('',*,*,#11425,.F.);
#16203=ORIENTED_EDGE('',*,*,#11422,.F.);
#16204=ORIENTED_EDGE('',*,*,#11419,.F.);
#16205=ORIENTED_EDGE('',*,*,#11416,.F.);
#16206=ORIENTED_EDGE('',*,*,#11413,.F.);
#16207=ORIENTED_EDGE('',*,*,#11410,.F.);
#16208=ORIENTED_EDGE('',*,*,#11407,.F.);
#16209=ORIENTED_EDGE('',*,*,#11451,.F.);
#16210=ORIENTED_EDGE('',*,*,#11454,.F.);
#16211=ORIENTED_EDGE('',*,*,#11457,.F.);
#16212=ORIENTED_EDGE('',*,*,#11460,.F.);
#16213=ORIENTED_EDGE('',*,*,#11463,.F.);
#16214=ORIENTED_EDGE('',*,*,#11466,.F.);
#16215=ORIENTED_EDGE('',*,*,#11469,.F.);
#16216=ORIENTED_EDGE('',*,*,#11472,.F.);
#16217=ORIENTED_EDGE('',*,*,#11475,.F.);
#16218=ORIENTED_EDGE('',*,*,#11478,.F.);
#16219=ORIENTED_EDGE('',*,*,#11481,.F.);
#16220=ORIENTED_EDGE('',*,*,#11484,.F.);
#16221=ORIENTED_EDGE('',*,*,#11487,.F.);
#16222=ORIENTED_EDGE('',*,*,#11490,.F.);
#16223=ORIENTED_EDGE('',*,*,#11493,.F.);
#16224=ORIENTED_EDGE('',*,*,#11496,.F.);
#16225=ORIENTED_EDGE('',*,*,#11570,.F.);
#16226=ORIENTED_EDGE('',*,*,#11608,.T.);
#16227=ORIENTED_EDGE('',*,*,#11606,.T.);
#16228=ORIENTED_EDGE('',*,*,#11604,.T.);
#16229=ORIENTED_EDGE('',*,*,#11602,.T.);
#16230=ORIENTED_EDGE('',*,*,#11600,.T.);
#16231=ORIENTED_EDGE('',*,*,#11598,.T.);
#16232=ORIENTED_EDGE('',*,*,#11596,.T.);
#16233=ORIENTED_EDGE('',*,*,#11594,.T.);
#16234=ORIENTED_EDGE('',*,*,#11592,.T.);
#16235=ORIENTED_EDGE('',*,*,#11590,.T.);
#16236=ORIENTED_EDGE('',*,*,#11588,.T.);
#16237=ORIENTED_EDGE('',*,*,#11586,.T.);
#16238=ORIENTED_EDGE('',*,*,#11584,.T.);
#16239=ORIENTED_EDGE('',*,*,#11582,.T.);
#16240=ORIENTED_EDGE('',*,*,#11580,.T.);
#16241=ORIENTED_EDGE('',*,*,#11578,.T.);
#16242=ORIENTED_EDGE('',*,*,#11545,.T.);
#16243=ORIENTED_EDGE('',*,*,#11548,.T.);
#16244=ORIENTED_EDGE('',*,*,#11550,.T.);
#16245=ORIENTED_EDGE('',*,*,#11552,.T.);
#16246=ORIENTED_EDGE('',*,*,#11554,.T.);
#16247=ORIENTED_EDGE('',*,*,#11556,.T.);
#16248=ORIENTED_EDGE('',*,*,#11557,.T.);
#16249=ORIENTED_EDGE('',*,*,#11335,.F.);
#16250=ORIENTED_EDGE('',*,*,#11339,.F.);
#16251=ORIENTED_EDGE('',*,*,#11342,.F.);
#16252=ORIENTED_EDGE('',*,*,#11345,.F.);
#16253=ORIENTED_EDGE('',*,*,#11348,.F.);
#16254=ORIENTED_EDGE('',*,*,#11351,.F.);
#16255=ORIENTED_EDGE('',*,*,#11371,.F.);
#16256=ORIENTED_EDGE('',*,*,#11391,.T.);
#16257=ORIENTED_EDGE('',*,*,#11388,.T.);
#16258=ORIENTED_EDGE('',*,*,#11385,.T.);
#16259=ORIENTED_EDGE('',*,*,#11382,.T.);
#16260=ORIENTED_EDGE('',*,*,#11379,.T.);
#16261=ORIENTED_EDGE('',*,*,#11376,.T.);
#16262=ORIENTED_EDGE('',*,*,#11373,.T.);
#16263=ORIENTED_EDGE('',*,*,#11200,.F.);
#16264=ORIENTED_EDGE('',*,*,#11204,.F.);
#16265=ORIENTED_EDGE('',*,*,#11207,.F.);
#16266=ORIENTED_EDGE('',*,*,#11210,.F.);
#16267=ORIENTED_EDGE('',*,*,#11213,.F.);
#16268=ORIENTED_EDGE('',*,*,#11216,.F.);
#16269=ORIENTED_EDGE('',*,*,#11236,.F.);
#16270=ORIENTED_EDGE('',*,*,#11256,.T.);
#16271=ORIENTED_EDGE('',*,*,#11253,.T.);
#16272=ORIENTED_EDGE('',*,*,#11250,.T.);
#16273=ORIENTED_EDGE('',*,*,#11247,.T.);
#16274=ORIENTED_EDGE('',*,*,#11244,.T.);
#16275=ORIENTED_EDGE('',*,*,#11241,.T.);
#16276=ORIENTED_EDGE('',*,*,#11238,.T.);
#16277=ORIENTED_EDGE('',*,*,#10852,.F.);
#16278=ORIENTED_EDGE('',*,*,#10856,.F.);
#16279=ORIENTED_EDGE('',*,*,#10859,.F.);
#16280=ORIENTED_EDGE('',*,*,#10862,.F.);
#16281=ORIENTED_EDGE('',*,*,#10865,.F.);
#16282=ORIENTED_EDGE('',*,*,#10868,.F.);
#16283=ORIENTED_EDGE('',*,*,#10886,.F.);
#16284=ORIENTED_EDGE('',*,*,#10904,.T.);
#16285=ORIENTED_EDGE('',*,*,#10901,.T.);
#16286=ORIENTED_EDGE('',*,*,#10898,.T.);
#16287=ORIENTED_EDGE('',*,*,#10895,.T.);
#16288=ORIENTED_EDGE('',*,*,#10892,.T.);
#16289=ORIENTED_EDGE('',*,*,#10889,.T.);
#16290=ORIENTED_EDGE('',*,*,#10938,.F.);
#16291=ORIENTED_EDGE('',*,*,#10935,.F.);
#16292=ORIENTED_EDGE('',*,*,#10932,.F.);
#16293=ORIENTED_EDGE('',*,*,#10929,.F.);
#16294=ORIENTED_EDGE('',*,*,#10926,.F.);
#16295=ORIENTED_EDGE('',*,*,#10923,.F.);
#16296=ORIENTED_EDGE('',*,*,#10920,.F.);
#16297=ORIENTED_EDGE('',*,*,#10964,.F.);
#16298=ORIENTED_EDGE('',*,*,#10967,.F.);
#16299=ORIENTED_EDGE('',*,*,#10970,.F.);
#16300=ORIENTED_EDGE('',*,*,#10973,.F.);
#16301=ORIENTED_EDGE('',*,*,#10976,.F.);
#16302=ORIENTED_EDGE('',*,*,#10979,.F.);
#16303=ORIENTED_EDGE('',*,*,#10982,.F.);
#16304=ORIENTED_EDGE('',*,*,#10985,.F.);
#16305=ORIENTED_EDGE('',*,*,#10988,.F.);
#16306=ORIENTED_EDGE('',*,*,#10991,.F.);
#16307=ORIENTED_EDGE('',*,*,#10994,.F.);
#16308=ORIENTED_EDGE('',*,*,#10997,.F.);
#16309=ORIENTED_EDGE('',*,*,#11000,.F.);
#16310=ORIENTED_EDGE('',*,*,#11003,.F.);
#16311=ORIENTED_EDGE('',*,*,#11006,.F.);
#16312=ORIENTED_EDGE('',*,*,#11009,.F.);
#16313=ORIENTED_EDGE('',*,*,#11063,.F.);
#16314=ORIENTED_EDGE('',*,*,#11121,.T.);
#16315=ORIENTED_EDGE('',*,*,#11118,.T.);
#16316=ORIENTED_EDGE('',*,*,#11115,.T.);
#16317=ORIENTED_EDGE('',*,*,#11112,.T.);
#16318=ORIENTED_EDGE('',*,*,#11109,.T.);
#16319=ORIENTED_EDGE('',*,*,#11106,.T.);
#16320=ORIENTED_EDGE('',*,*,#11103,.T.);
#16321=ORIENTED_EDGE('',*,*,#11100,.T.);
#16322=ORIENTED_EDGE('',*,*,#11097,.T.);
#16323=ORIENTED_EDGE('',*,*,#11094,.T.);
#16324=ORIENTED_EDGE('',*,*,#11091,.T.);
#16325=ORIENTED_EDGE('',*,*,#11088,.T.);
#16326=ORIENTED_EDGE('',*,*,#11085,.T.);
#16327=ORIENTED_EDGE('',*,*,#11082,.T.);
#16328=ORIENTED_EDGE('',*,*,#11079,.T.);
#16329=ORIENTED_EDGE('',*,*,#11076,.T.);
#16330=ORIENTED_EDGE('',*,*,#11025,.T.);
#16331=ORIENTED_EDGE('',*,*,#11029,.T.);
#16332=ORIENTED_EDGE('',*,*,#11032,.T.);
#16333=ORIENTED_EDGE('',*,*,#11035,.T.);
#16334=ORIENTED_EDGE('',*,*,#11038,.T.);
#16335=ORIENTED_EDGE('',*,*,#11041,.T.);
#16336=ORIENTED_EDGE('',*,*,#11043,.T.);
#16337=ORIENTED_EDGE('',*,*,#10822,.F.);
#16338=ORIENTED_EDGE('',*,*,#10826,.F.);
#16339=ORIENTED_EDGE('',*,*,#10829,.F.);
#16340=ORIENTED_EDGE('',*,*,#10832,.F.);
#16341=ORIENTED_EDGE('',*,*,#10835,.F.);
#16342=ORIENTED_EDGE('',*,*,#10837,.F.);
#16343=ORIENTED_EDGE('',*,*,#10818,.T.);
#16344=ORIENTED_EDGE('',*,*,#10805,.T.);
#16345=ORIENTED_EDGE('',*,*,#10802,.T.);
#16346=ORIENTED_EDGE('',*,*,#10799,.T.);
#16347=ORIENTED_EDGE('',*,*,#10796,.T.);
#16348=ORIENTED_EDGE('',*,*,#10793,.T.);
#16349=ORIENTED_EDGE('',*,*,#10790,.T.);
#16350=ORIENTED_EDGE('',*,*,#11022,.T.);
#16351=ORIENTED_EDGE('',*,*,#11074,.T.);
#16352=ORIENTED_EDGE('',*,*,#11071,.T.);
#16353=ORIENTED_EDGE('',*,*,#11068,.T.);
#16354=ORIENTED_EDGE('',*,*,#11065,.T.);
#16355=ORIENTED_EDGE('',*,*,#11012,.T.);
#16356=ORIENTED_EDGE('',*,*,#11016,.T.);
#16357=ORIENTED_EDGE('',*,*,#11019,.T.);
#16358=ORIENTED_EDGE('',*,*,#10916,.F.);
#16359=ORIENTED_EDGE('',*,*,#10913,.F.);
#16360=ORIENTED_EDGE('',*,*,#10910,.F.);
#16361=ORIENTED_EDGE('',*,*,#10907,.F.);
#16362=ORIENTED_EDGE('',*,*,#10953,.F.);
#16363=ORIENTED_EDGE('',*,*,#10956,.F.);
#16364=ORIENTED_EDGE('',*,*,#10959,.F.);
#16365=ORIENTED_EDGE('',*,*,#10961,.F.);
#16366=ORIENTED_EDGE('',*,*,#11058,.T.);
#16367=ORIENTED_EDGE('',*,*,#10881,.F.);
#16368=ORIENTED_EDGE('',*,*,#11046,.F.);
#16369=ORIENTED_EDGE('',*,*,#11049,.T.);
#16370=ORIENTED_EDGE('',*,*,#11052,.T.);
#16371=ORIENTED_EDGE('',*,*,#11055,.T.);
#16372=ORIENTED_EDGE('',*,*,#11057,.T.);
#16373=ORIENTED_EDGE('',*,*,#10949,.F.);
#16374=ORIENTED_EDGE('',*,*,#10946,.F.);
#16375=ORIENTED_EDGE('',*,*,#10943,.F.);
#16376=ORIENTED_EDGE('',*,*,#10940,.T.);
#16377=ORIENTED_EDGE('',*,*,#10871,.T.);
#16378=ORIENTED_EDGE('',*,*,#10875,.T.);
#16379=ORIENTED_EDGE('',*,*,#10878,.T.);
#16380=ORIENTED_EDGE('',*,*,#10880,.T.);
#16381=ORIENTED_EDGE('',*,*,#10815,.F.);
#16382=ORIENTED_EDGE('',*,*,#10812,.F.);
#16383=ORIENTED_EDGE('',*,*,#10809,.F.);
#16384=ORIENTED_EDGE('',*,*,#11152,.F.);
#16385=ORIENTED_EDGE('',*,*,#10780,.T.);
#16386=ORIENTED_EDGE('',*,*,#10784,.T.);
#16387=ORIENTED_EDGE('',*,*,#10787,.T.);
#16388=ORIENTED_EDGE('',*,*,#10849,.F.);
#16389=ORIENTED_EDGE('',*,*,#10846,.F.);
#16390=ORIENTED_EDGE('',*,*,#10843,.F.);
#16391=ORIENTED_EDGE('',*,*,#10840,.F.);
#16392=ORIENTED_EDGE('',*,*,#11219,.F.);
#16393=ORIENTED_EDGE('',*,*,#11222,.T.);
#16394=ORIENTED_EDGE('',*,*,#11225,.T.);
#16395=ORIENTED_EDGE('',*,*,#11228,.T.);
#16396=ORIENTED_EDGE('',*,*,#11230,.T.);
#16397=ORIENTED_EDGE('',*,*,#11161,.F.);
#16398=ORIENTED_EDGE('',*,*,#11158,.F.);
#16399=ORIENTED_EDGE('',*,*,#11155,.F.);
#16400=ORIENTED_EDGE('',*,*,#11231,.F.);
#16401=ORIENTED_EDGE('',*,*,#11287,.F.);
#16402=ORIENTED_EDGE('',*,*,#11124,.T.);
#16403=ORIENTED_EDGE('',*,*,#11128,.T.);
#16404=ORIENTED_EDGE('',*,*,#11131,.T.);
#16405=ORIENTED_EDGE('',*,*,#11197,.F.);
#16406=ORIENTED_EDGE('',*,*,#11194,.F.);
#16407=ORIENTED_EDGE('',*,*,#11191,.F.);
#16408=ORIENTED_EDGE('',*,*,#11188,.F.);
#16409=ORIENTED_EDGE('',*,*,#11354,.F.);
#16410=ORIENTED_EDGE('',*,*,#11357,.T.);
#16411=ORIENTED_EDGE('',*,*,#11360,.T.);
#16412=ORIENTED_EDGE('',*,*,#11363,.T.);
#16413=ORIENTED_EDGE('',*,*,#11365,.T.);
#16414=ORIENTED_EDGE('',*,*,#11296,.F.);
#16415=ORIENTED_EDGE('',*,*,#11293,.F.);
#16416=ORIENTED_EDGE('',*,*,#11290,.F.);
#16417=ORIENTED_EDGE('',*,*,#11366,.F.);
#16418=ORIENTED_EDGE('',*,*,#11567,.T.);
#16419=ORIENTED_EDGE('',*,*,#11403,.F.);
#16420=ORIENTED_EDGE('',*,*,#11400,.F.);
#16421=ORIENTED_EDGE('',*,*,#11397,.F.);
#16422=ORIENTED_EDGE('',*,*,#11394,.F.);
#16423=ORIENTED_EDGE('',*,*,#11440,.F.);
#16424=ORIENTED_EDGE('',*,*,#11443,.F.);
#16425=ORIENTED_EDGE('',*,*,#11446,.F.);
#16426=ORIENTED_EDGE('',*,*,#11448,.F.);
#16427=ORIENTED_EDGE('',*,*,#11543,.T.);
#16428=ORIENTED_EDGE('',*,*,#11577,.T.);
#16429=ORIENTED_EDGE('',*,*,#11575,.T.);
#16430=ORIENTED_EDGE('',*,*,#11573,.T.);
#16431=ORIENTED_EDGE('',*,*,#11571,.T.);
#16432=ORIENTED_EDGE('',*,*,#11536,.T.);
#16433=ORIENTED_EDGE('',*,*,#11539,.T.);
#16434=ORIENTED_EDGE('',*,*,#11541,.T.);
#16435=ORIENTED_EDGE('',*,*,#11427,.T.);
#16436=ORIENTED_EDGE('',*,*,#11259,.T.);
#16437=ORIENTED_EDGE('',*,*,#11263,.T.);
#16438=ORIENTED_EDGE('',*,*,#11266,.T.);
#16439=ORIENTED_EDGE('',*,*,#11332,.F.);
#16440=ORIENTED_EDGE('',*,*,#11329,.F.);
#16441=ORIENTED_EDGE('',*,*,#11326,.F.);
#16442=ORIENTED_EDGE('',*,*,#11323,.F.);
#16443=ORIENTED_EDGE('',*,*,#11559,.F.);
#16444=ORIENTED_EDGE('',*,*,#11561,.T.);
#16445=ORIENTED_EDGE('',*,*,#11563,.T.);
#16446=ORIENTED_EDGE('',*,*,#11565,.T.);
#16447=ORIENTED_EDGE('',*,*,#11566,.T.);
#16448=ORIENTED_EDGE('',*,*,#11436,.F.);
#16449=ORIENTED_EDGE('',*,*,#11433,.F.);
#16450=ORIENTED_EDGE('',*,*,#11430,.F.);
#16451=ORIENTED_EDGE('',*,*,#11609,.F.);
#16452=ORIENTED_EDGE('',*,*,#11610,.T.);
#16453=ORIENTED_EDGE('',*,*,#11611,.F.);
#16454=ORIENTED_EDGE('',*,*,#11612,.T.);
#16455=ORIENTED_EDGE('',*,*,#11613,.F.);
#16456=ORIENTED_EDGE('',*,*,#11614,.T.);
#16457=ORIENTED_EDGE('',*,*,#11609,.T.);
#16458=ORIENTED_EDGE('',*,*,#11615,.T.);
#16459=ORIENTED_EDGE('',*,*,#11616,.F.);
#16460=ORIENTED_EDGE('',*,*,#11617,.T.);
#16461=ORIENTED_EDGE('',*,*,#11613,.T.);
#16462=ORIENTED_EDGE('',*,*,#11618,.T.);
#16463=ORIENTED_EDGE('',*,*,#11619,.F.);
#16464=ORIENTED_EDGE('',*,*,#11620,.T.);
#16465=ORIENTED_EDGE('',*,*,#11616,.T.);
#16466=ORIENTED_EDGE('',*,*,#11621,.T.);
#16467=ORIENTED_EDGE('',*,*,#11622,.F.);
#16468=ORIENTED_EDGE('',*,*,#11623,.T.);
#16469=ORIENTED_EDGE('',*,*,#11619,.T.);
#16470=ORIENTED_EDGE('',*,*,#11624,.T.);
#16471=ORIENTED_EDGE('',*,*,#11625,.F.);
#16472=ORIENTED_EDGE('',*,*,#11626,.T.);
#16473=ORIENTED_EDGE('',*,*,#11622,.T.);
#16474=ORIENTED_EDGE('',*,*,#11627,.T.);
#16475=ORIENTED_EDGE('',*,*,#11628,.F.);
#16476=ORIENTED_EDGE('',*,*,#11629,.T.);
#16477=ORIENTED_EDGE('',*,*,#11625,.T.);
#16478=ORIENTED_EDGE('',*,*,#11630,.T.);
#16479=ORIENTED_EDGE('',*,*,#11631,.F.);
#16480=ORIENTED_EDGE('',*,*,#11632,.T.);
#16481=ORIENTED_EDGE('',*,*,#11628,.T.);
#16482=ORIENTED_EDGE('',*,*,#11633,.T.);
#16483=ORIENTED_EDGE('',*,*,#11634,.F.);
#16484=ORIENTED_EDGE('',*,*,#11635,.T.);
#16485=ORIENTED_EDGE('',*,*,#11631,.T.);
#16486=ORIENTED_EDGE('',*,*,#11636,.T.);
#16487=ORIENTED_EDGE('',*,*,#11637,.F.);
#16488=ORIENTED_EDGE('',*,*,#11638,.T.);
#16489=ORIENTED_EDGE('',*,*,#11634,.T.);
#16490=ORIENTED_EDGE('',*,*,#11639,.T.);
#16491=ORIENTED_EDGE('',*,*,#11640,.F.);
#16492=ORIENTED_EDGE('',*,*,#11641,.T.);
#16493=ORIENTED_EDGE('',*,*,#11637,.T.);
#16494=ORIENTED_EDGE('',*,*,#11642,.T.);
#16495=ORIENTED_EDGE('',*,*,#11643,.F.);
#16496=ORIENTED_EDGE('',*,*,#11644,.T.);
#16497=ORIENTED_EDGE('',*,*,#11640,.T.);
#16498=ORIENTED_EDGE('',*,*,#11645,.T.);
#16499=ORIENTED_EDGE('',*,*,#11646,.F.);
#16500=ORIENTED_EDGE('',*,*,#11647,.T.);
#16501=ORIENTED_EDGE('',*,*,#11643,.T.);
#16502=ORIENTED_EDGE('',*,*,#11648,.T.);
#16503=ORIENTED_EDGE('',*,*,#11649,.F.);
#16504=ORIENTED_EDGE('',*,*,#11650,.T.);
#16505=ORIENTED_EDGE('',*,*,#11646,.T.);
#16506=ORIENTED_EDGE('',*,*,#11651,.T.);
#16507=ORIENTED_EDGE('',*,*,#11652,.F.);
#16508=ORIENTED_EDGE('',*,*,#11653,.T.);
#16509=ORIENTED_EDGE('',*,*,#11649,.T.);
#16510=ORIENTED_EDGE('',*,*,#11654,.T.);
#16511=ORIENTED_EDGE('',*,*,#11655,.F.);
#16512=ORIENTED_EDGE('',*,*,#11656,.T.);
#16513=ORIENTED_EDGE('',*,*,#11652,.T.);
#16514=ORIENTED_EDGE('',*,*,#11657,.T.);
#16515=ORIENTED_EDGE('',*,*,#11658,.F.);
#16516=ORIENTED_EDGE('',*,*,#11659,.T.);
#16517=ORIENTED_EDGE('',*,*,#11655,.T.);
#16518=ORIENTED_EDGE('',*,*,#11660,.T.);
#16519=ORIENTED_EDGE('',*,*,#11661,.F.);
#16520=ORIENTED_EDGE('',*,*,#11662,.T.);
#16521=ORIENTED_EDGE('',*,*,#11658,.T.);
#16522=ORIENTED_EDGE('',*,*,#11663,.T.);
#16523=ORIENTED_EDGE('',*,*,#11664,.F.);
#16524=ORIENTED_EDGE('',*,*,#11665,.T.);
#16525=ORIENTED_EDGE('',*,*,#11661,.T.);
#16526=ORIENTED_EDGE('',*,*,#11666,.T.);
#16527=ORIENTED_EDGE('',*,*,#11667,.F.);
#16528=ORIENTED_EDGE('',*,*,#11668,.T.);
#16529=ORIENTED_EDGE('',*,*,#11664,.T.);
#16530=ORIENTED_EDGE('',*,*,#11669,.T.);
#16531=ORIENTED_EDGE('',*,*,#11670,.F.);
#16532=ORIENTED_EDGE('',*,*,#11671,.T.);
#16533=ORIENTED_EDGE('',*,*,#11667,.T.);
#16534=ORIENTED_EDGE('',*,*,#11672,.T.);
#16535=ORIENTED_EDGE('',*,*,#11673,.F.);
#16536=ORIENTED_EDGE('',*,*,#11674,.T.);
#16537=ORIENTED_EDGE('',*,*,#11670,.T.);
#16538=ORIENTED_EDGE('',*,*,#11675,.T.);
#16539=ORIENTED_EDGE('',*,*,#11676,.F.);
#16540=ORIENTED_EDGE('',*,*,#11677,.T.);
#16541=ORIENTED_EDGE('',*,*,#11673,.T.);
#16542=ORIENTED_EDGE('',*,*,#11678,.T.);
#16543=ORIENTED_EDGE('',*,*,#11679,.F.);
#16544=ORIENTED_EDGE('',*,*,#11680,.T.);
#16545=ORIENTED_EDGE('',*,*,#11676,.T.);
#16546=ORIENTED_EDGE('',*,*,#11681,.T.);
#16547=ORIENTED_EDGE('',*,*,#11682,.F.);
#16548=ORIENTED_EDGE('',*,*,#11683,.T.);
#16549=ORIENTED_EDGE('',*,*,#11679,.T.);
#16550=ORIENTED_EDGE('',*,*,#11684,.T.);
#16551=ORIENTED_EDGE('',*,*,#11685,.F.);
#16552=ORIENTED_EDGE('',*,*,#11686,.T.);
#16553=ORIENTED_EDGE('',*,*,#11682,.T.);
#16554=ORIENTED_EDGE('',*,*,#11687,.T.);
#16555=ORIENTED_EDGE('',*,*,#11688,.F.);
#16556=ORIENTED_EDGE('',*,*,#11689,.T.);
#16557=ORIENTED_EDGE('',*,*,#11685,.T.);
#16558=ORIENTED_EDGE('',*,*,#11690,.T.);
#16559=ORIENTED_EDGE('',*,*,#11691,.F.);
#16560=ORIENTED_EDGE('',*,*,#11692,.T.);
#16561=ORIENTED_EDGE('',*,*,#11688,.T.);
#16562=ORIENTED_EDGE('',*,*,#11693,.T.);
#16563=ORIENTED_EDGE('',*,*,#11694,.F.);
#16564=ORIENTED_EDGE('',*,*,#11695,.T.);
#16565=ORIENTED_EDGE('',*,*,#11691,.T.);
#16566=ORIENTED_EDGE('',*,*,#11696,.T.);
#16567=ORIENTED_EDGE('',*,*,#11697,.F.);
#16568=ORIENTED_EDGE('',*,*,#11698,.T.);
#16569=ORIENTED_EDGE('',*,*,#11694,.T.);
#16570=ORIENTED_EDGE('',*,*,#11699,.T.);
#16571=ORIENTED_EDGE('',*,*,#11700,.F.);
#16572=ORIENTED_EDGE('',*,*,#11701,.T.);
#16573=ORIENTED_EDGE('',*,*,#11697,.T.);
#16574=ORIENTED_EDGE('',*,*,#11702,.T.);
#16575=ORIENTED_EDGE('',*,*,#11703,.F.);
#16576=ORIENTED_EDGE('',*,*,#11704,.T.);
#16577=ORIENTED_EDGE('',*,*,#11700,.T.);
#16578=ORIENTED_EDGE('',*,*,#11705,.T.);
#16579=ORIENTED_EDGE('',*,*,#11706,.F.);
#16580=ORIENTED_EDGE('',*,*,#11707,.T.);
#16581=ORIENTED_EDGE('',*,*,#11703,.T.);
#16582=ORIENTED_EDGE('',*,*,#11708,.T.);
#16583=ORIENTED_EDGE('',*,*,#11709,.F.);
#16584=ORIENTED_EDGE('',*,*,#11710,.T.);
#16585=ORIENTED_EDGE('',*,*,#11706,.T.);
#16586=ORIENTED_EDGE('',*,*,#11711,.T.);
#16587=ORIENTED_EDGE('',*,*,#11712,.F.);
#16588=ORIENTED_EDGE('',*,*,#11713,.T.);
#16589=ORIENTED_EDGE('',*,*,#11709,.T.);
#16590=ORIENTED_EDGE('',*,*,#11714,.T.);
#16591=ORIENTED_EDGE('',*,*,#11715,.F.);
#16592=ORIENTED_EDGE('',*,*,#11716,.T.);
#16593=ORIENTED_EDGE('',*,*,#11712,.T.);
#16594=ORIENTED_EDGE('',*,*,#11717,.T.);
#16595=ORIENTED_EDGE('',*,*,#11718,.F.);
#16596=ORIENTED_EDGE('',*,*,#11719,.T.);
#16597=ORIENTED_EDGE('',*,*,#11715,.T.);
#16598=ORIENTED_EDGE('',*,*,#11720,.T.);
#16599=ORIENTED_EDGE('',*,*,#11721,.F.);
#16600=ORIENTED_EDGE('',*,*,#11722,.T.);
#16601=ORIENTED_EDGE('',*,*,#11718,.T.);
#16602=ORIENTED_EDGE('',*,*,#11723,.T.);
#16603=ORIENTED_EDGE('',*,*,#11724,.F.);
#16604=ORIENTED_EDGE('',*,*,#11725,.T.);
#16605=ORIENTED_EDGE('',*,*,#11721,.T.);
#16606=ORIENTED_EDGE('',*,*,#11726,.T.);
#16607=ORIENTED_EDGE('',*,*,#11727,.F.);
#16608=ORIENTED_EDGE('',*,*,#11728,.T.);
#16609=ORIENTED_EDGE('',*,*,#11724,.T.);
#16610=ORIENTED_EDGE('',*,*,#11729,.T.);
#16611=ORIENTED_EDGE('',*,*,#11730,.F.);
#16612=ORIENTED_EDGE('',*,*,#11731,.T.);
#16613=ORIENTED_EDGE('',*,*,#11727,.T.);
#16614=ORIENTED_EDGE('',*,*,#11732,.T.);
#16615=ORIENTED_EDGE('',*,*,#11733,.F.);
#16616=ORIENTED_EDGE('',*,*,#11734,.T.);
#16617=ORIENTED_EDGE('',*,*,#11730,.T.);
#16618=ORIENTED_EDGE('',*,*,#11735,.T.);
#16619=ORIENTED_EDGE('',*,*,#11736,.F.);
#16620=ORIENTED_EDGE('',*,*,#11737,.T.);
#16621=ORIENTED_EDGE('',*,*,#11733,.T.);
#16622=ORIENTED_EDGE('',*,*,#11738,.T.);
#16623=ORIENTED_EDGE('',*,*,#11739,.F.);
#16624=ORIENTED_EDGE('',*,*,#11740,.T.);
#16625=ORIENTED_EDGE('',*,*,#11736,.T.);
#16626=ORIENTED_EDGE('',*,*,#11741,.T.);
#16627=ORIENTED_EDGE('',*,*,#11742,.F.);
#16628=ORIENTED_EDGE('',*,*,#11743,.T.);
#16629=ORIENTED_EDGE('',*,*,#11739,.T.);
#16630=ORIENTED_EDGE('',*,*,#11744,.T.);
#16631=ORIENTED_EDGE('',*,*,#11745,.F.);
#16632=ORIENTED_EDGE('',*,*,#11746,.T.);
#16633=ORIENTED_EDGE('',*,*,#11742,.T.);
#16634=ORIENTED_EDGE('',*,*,#11747,.T.);
#16635=ORIENTED_EDGE('',*,*,#11748,.F.);
#16636=ORIENTED_EDGE('',*,*,#11749,.T.);
#16637=ORIENTED_EDGE('',*,*,#11745,.T.);
#16638=ORIENTED_EDGE('',*,*,#11750,.T.);
#16639=ORIENTED_EDGE('',*,*,#11751,.F.);
#16640=ORIENTED_EDGE('',*,*,#11752,.T.);
#16641=ORIENTED_EDGE('',*,*,#11748,.T.);
#16642=ORIENTED_EDGE('',*,*,#11753,.T.);
#16643=ORIENTED_EDGE('',*,*,#11754,.F.);
#16644=ORIENTED_EDGE('',*,*,#11755,.T.);
#16645=ORIENTED_EDGE('',*,*,#11751,.T.);
#16646=ORIENTED_EDGE('',*,*,#11756,.T.);
#16647=ORIENTED_EDGE('',*,*,#11757,.F.);
#16648=ORIENTED_EDGE('',*,*,#11758,.T.);
#16649=ORIENTED_EDGE('',*,*,#11754,.T.);
#16650=ORIENTED_EDGE('',*,*,#11759,.T.);
#16651=ORIENTED_EDGE('',*,*,#11760,.F.);
#16652=ORIENTED_EDGE('',*,*,#11761,.T.);
#16653=ORIENTED_EDGE('',*,*,#11757,.T.);
#16654=ORIENTED_EDGE('',*,*,#11762,.T.);
#16655=ORIENTED_EDGE('',*,*,#11763,.F.);
#16656=ORIENTED_EDGE('',*,*,#11764,.T.);
#16657=ORIENTED_EDGE('',*,*,#11760,.T.);
#16658=ORIENTED_EDGE('',*,*,#11765,.T.);
#16659=ORIENTED_EDGE('',*,*,#11766,.F.);
#16660=ORIENTED_EDGE('',*,*,#11767,.T.);
#16661=ORIENTED_EDGE('',*,*,#11763,.T.);
#16662=ORIENTED_EDGE('',*,*,#11768,.T.);
#16663=ORIENTED_EDGE('',*,*,#11769,.F.);
#16664=ORIENTED_EDGE('',*,*,#11770,.T.);
#16665=ORIENTED_EDGE('',*,*,#11766,.T.);
#16666=ORIENTED_EDGE('',*,*,#11771,.T.);
#16667=ORIENTED_EDGE('',*,*,#11772,.F.);
#16668=ORIENTED_EDGE('',*,*,#11773,.T.);
#16669=ORIENTED_EDGE('',*,*,#11769,.T.);
#16670=ORIENTED_EDGE('',*,*,#11774,.T.);
#16671=ORIENTED_EDGE('',*,*,#11775,.F.);
#16672=ORIENTED_EDGE('',*,*,#11776,.T.);
#16673=ORIENTED_EDGE('',*,*,#11772,.T.);
#16674=ORIENTED_EDGE('',*,*,#11777,.T.);
#16675=ORIENTED_EDGE('',*,*,#11778,.F.);
#16676=ORIENTED_EDGE('',*,*,#11779,.T.);
#16677=ORIENTED_EDGE('',*,*,#11775,.T.);
#16678=ORIENTED_EDGE('',*,*,#11780,.T.);
#16679=ORIENTED_EDGE('',*,*,#11781,.F.);
#16680=ORIENTED_EDGE('',*,*,#11782,.T.);
#16681=ORIENTED_EDGE('',*,*,#11778,.T.);
#16682=ORIENTED_EDGE('',*,*,#11783,.T.);
#16683=ORIENTED_EDGE('',*,*,#11784,.F.);
#16684=ORIENTED_EDGE('',*,*,#11785,.T.);
#16685=ORIENTED_EDGE('',*,*,#11781,.T.);
#16686=ORIENTED_EDGE('',*,*,#11786,.T.);
#16687=ORIENTED_EDGE('',*,*,#11787,.F.);
#16688=ORIENTED_EDGE('',*,*,#11788,.T.);
#16689=ORIENTED_EDGE('',*,*,#11784,.T.);
#16690=ORIENTED_EDGE('',*,*,#11789,.T.);
#16691=ORIENTED_EDGE('',*,*,#11790,.F.);
#16692=ORIENTED_EDGE('',*,*,#11791,.T.);
#16693=ORIENTED_EDGE('',*,*,#11787,.T.);
#16694=ORIENTED_EDGE('',*,*,#11792,.T.);
#16695=ORIENTED_EDGE('',*,*,#11793,.F.);
#16696=ORIENTED_EDGE('',*,*,#11794,.T.);
#16697=ORIENTED_EDGE('',*,*,#11790,.T.);
#16698=ORIENTED_EDGE('',*,*,#11795,.T.);
#16699=ORIENTED_EDGE('',*,*,#11796,.F.);
#16700=ORIENTED_EDGE('',*,*,#11797,.T.);
#16701=ORIENTED_EDGE('',*,*,#11793,.T.);
#16702=ORIENTED_EDGE('',*,*,#11798,.T.);
#16703=ORIENTED_EDGE('',*,*,#11799,.F.);
#16704=ORIENTED_EDGE('',*,*,#11800,.T.);
#16705=ORIENTED_EDGE('',*,*,#11796,.T.);
#16706=ORIENTED_EDGE('',*,*,#11801,.T.);
#16707=ORIENTED_EDGE('',*,*,#11802,.F.);
#16708=ORIENTED_EDGE('',*,*,#11803,.T.);
#16709=ORIENTED_EDGE('',*,*,#11799,.T.);
#16710=ORIENTED_EDGE('',*,*,#11804,.T.);
#16711=ORIENTED_EDGE('',*,*,#11805,.F.);
#16712=ORIENTED_EDGE('',*,*,#11806,.T.);
#16713=ORIENTED_EDGE('',*,*,#11802,.T.);
#16714=ORIENTED_EDGE('',*,*,#11807,.T.);
#16715=ORIENTED_EDGE('',*,*,#11808,.F.);
#16716=ORIENTED_EDGE('',*,*,#11809,.T.);
#16717=ORIENTED_EDGE('',*,*,#11805,.T.);
#16718=ORIENTED_EDGE('',*,*,#11810,.T.);
#16719=ORIENTED_EDGE('',*,*,#11811,.F.);
#16720=ORIENTED_EDGE('',*,*,#11812,.T.);
#16721=ORIENTED_EDGE('',*,*,#11808,.T.);
#16722=ORIENTED_EDGE('',*,*,#11813,.T.);
#16723=ORIENTED_EDGE('',*,*,#11814,.F.);
#16724=ORIENTED_EDGE('',*,*,#11815,.T.);
#16725=ORIENTED_EDGE('',*,*,#11811,.T.);
#16726=ORIENTED_EDGE('',*,*,#11816,.T.);
#16727=ORIENTED_EDGE('',*,*,#11817,.F.);
#16728=ORIENTED_EDGE('',*,*,#11818,.T.);
#16729=ORIENTED_EDGE('',*,*,#11814,.T.);
#16730=ORIENTED_EDGE('',*,*,#11819,.T.);
#16731=ORIENTED_EDGE('',*,*,#11820,.F.);
#16732=ORIENTED_EDGE('',*,*,#11821,.T.);
#16733=ORIENTED_EDGE('',*,*,#11817,.T.);
#16734=ORIENTED_EDGE('',*,*,#11822,.T.);
#16735=ORIENTED_EDGE('',*,*,#11823,.F.);
#16736=ORIENTED_EDGE('',*,*,#11824,.T.);
#16737=ORIENTED_EDGE('',*,*,#11820,.T.);
#16738=ORIENTED_EDGE('',*,*,#11825,.T.);
#16739=ORIENTED_EDGE('',*,*,#11826,.F.);
#16740=ORIENTED_EDGE('',*,*,#11827,.T.);
#16741=ORIENTED_EDGE('',*,*,#11823,.T.);
#16742=ORIENTED_EDGE('',*,*,#11828,.T.);
#16743=ORIENTED_EDGE('',*,*,#11829,.F.);
#16744=ORIENTED_EDGE('',*,*,#11830,.T.);
#16745=ORIENTED_EDGE('',*,*,#11826,.T.);
#16746=ORIENTED_EDGE('',*,*,#11831,.T.);
#16747=ORIENTED_EDGE('',*,*,#11832,.F.);
#16748=ORIENTED_EDGE('',*,*,#11833,.T.);
#16749=ORIENTED_EDGE('',*,*,#11829,.T.);
#16750=ORIENTED_EDGE('',*,*,#11834,.T.);
#16751=ORIENTED_EDGE('',*,*,#11835,.F.);
#16752=ORIENTED_EDGE('',*,*,#11836,.T.);
#16753=ORIENTED_EDGE('',*,*,#11832,.T.);
#16754=ORIENTED_EDGE('',*,*,#11837,.T.);
#16755=ORIENTED_EDGE('',*,*,#11838,.F.);
#16756=ORIENTED_EDGE('',*,*,#11839,.T.);
#16757=ORIENTED_EDGE('',*,*,#11835,.T.);
#16758=ORIENTED_EDGE('',*,*,#11840,.T.);
#16759=ORIENTED_EDGE('',*,*,#11841,.F.);
#16760=ORIENTED_EDGE('',*,*,#11842,.T.);
#16761=ORIENTED_EDGE('',*,*,#11838,.T.);
#16762=ORIENTED_EDGE('',*,*,#11843,.T.);
#16763=ORIENTED_EDGE('',*,*,#11844,.F.);
#16764=ORIENTED_EDGE('',*,*,#11845,.T.);
#16765=ORIENTED_EDGE('',*,*,#11841,.T.);
#16766=ORIENTED_EDGE('',*,*,#11846,.T.);
#16767=ORIENTED_EDGE('',*,*,#11847,.F.);
#16768=ORIENTED_EDGE('',*,*,#11848,.T.);
#16769=ORIENTED_EDGE('',*,*,#11844,.T.);
#16770=ORIENTED_EDGE('',*,*,#11849,.T.);
#16771=ORIENTED_EDGE('',*,*,#11850,.F.);
#16772=ORIENTED_EDGE('',*,*,#11851,.T.);
#16773=ORIENTED_EDGE('',*,*,#11847,.T.);
#16774=ORIENTED_EDGE('',*,*,#11852,.T.);
#16775=ORIENTED_EDGE('',*,*,#11853,.F.);
#16776=ORIENTED_EDGE('',*,*,#11854,.T.);
#16777=ORIENTED_EDGE('',*,*,#11850,.T.);
#16778=ORIENTED_EDGE('',*,*,#11855,.T.);
#16779=ORIENTED_EDGE('',*,*,#11856,.F.);
#16780=ORIENTED_EDGE('',*,*,#11857,.T.);
#16781=ORIENTED_EDGE('',*,*,#11853,.T.);
#16782=ORIENTED_EDGE('',*,*,#11858,.T.);
#16783=ORIENTED_EDGE('',*,*,#11859,.F.);
#16784=ORIENTED_EDGE('',*,*,#11860,.T.);
#16785=ORIENTED_EDGE('',*,*,#11856,.T.);
#16786=ORIENTED_EDGE('',*,*,#11861,.T.);
#16787=ORIENTED_EDGE('',*,*,#11862,.F.);
#16788=ORIENTED_EDGE('',*,*,#11863,.T.);
#16789=ORIENTED_EDGE('',*,*,#11859,.T.);
#16790=ORIENTED_EDGE('',*,*,#11864,.T.);
#16791=ORIENTED_EDGE('',*,*,#11865,.F.);
#16792=ORIENTED_EDGE('',*,*,#11866,.T.);
#16793=ORIENTED_EDGE('',*,*,#11862,.T.);
#16794=ORIENTED_EDGE('',*,*,#11867,.T.);
#16795=ORIENTED_EDGE('',*,*,#11868,.F.);
#16796=ORIENTED_EDGE('',*,*,#11869,.T.);
#16797=ORIENTED_EDGE('',*,*,#11865,.T.);
#16798=ORIENTED_EDGE('',*,*,#11870,.T.);
#16799=ORIENTED_EDGE('',*,*,#11871,.F.);
#16800=ORIENTED_EDGE('',*,*,#11872,.T.);
#16801=ORIENTED_EDGE('',*,*,#11868,.T.);
#16802=ORIENTED_EDGE('',*,*,#11873,.T.);
#16803=ORIENTED_EDGE('',*,*,#11874,.F.);
#16804=ORIENTED_EDGE('',*,*,#11875,.T.);
#16805=ORIENTED_EDGE('',*,*,#11871,.T.);
#16806=ORIENTED_EDGE('',*,*,#11876,.T.);
#16807=ORIENTED_EDGE('',*,*,#11877,.F.);
#16808=ORIENTED_EDGE('',*,*,#11878,.T.);
#16809=ORIENTED_EDGE('',*,*,#11874,.T.);
#16810=ORIENTED_EDGE('',*,*,#11879,.T.);
#16811=ORIENTED_EDGE('',*,*,#11880,.F.);
#16812=ORIENTED_EDGE('',*,*,#11881,.T.);
#16813=ORIENTED_EDGE('',*,*,#11877,.T.);
#16814=ORIENTED_EDGE('',*,*,#11882,.T.);
#16815=ORIENTED_EDGE('',*,*,#11883,.F.);
#16816=ORIENTED_EDGE('',*,*,#11884,.T.);
#16817=ORIENTED_EDGE('',*,*,#11880,.T.);
#16818=ORIENTED_EDGE('',*,*,#11885,.T.);
#16819=ORIENTED_EDGE('',*,*,#11886,.F.);
#16820=ORIENTED_EDGE('',*,*,#11887,.T.);
#16821=ORIENTED_EDGE('',*,*,#11883,.T.);
#16822=ORIENTED_EDGE('',*,*,#11888,.T.);
#16823=ORIENTED_EDGE('',*,*,#11889,.F.);
#16824=ORIENTED_EDGE('',*,*,#11890,.T.);
#16825=ORIENTED_EDGE('',*,*,#11886,.T.);
#16826=ORIENTED_EDGE('',*,*,#11891,.T.);
#16827=ORIENTED_EDGE('',*,*,#11892,.F.);
#16828=ORIENTED_EDGE('',*,*,#11893,.T.);
#16829=ORIENTED_EDGE('',*,*,#11889,.T.);
#16830=ORIENTED_EDGE('',*,*,#11894,.T.);
#16831=ORIENTED_EDGE('',*,*,#11895,.F.);
#16832=ORIENTED_EDGE('',*,*,#11896,.T.);
#16833=ORIENTED_EDGE('',*,*,#11892,.T.);
#16834=ORIENTED_EDGE('',*,*,#11897,.T.);
#16835=ORIENTED_EDGE('',*,*,#11898,.F.);
#16836=ORIENTED_EDGE('',*,*,#11899,.T.);
#16837=ORIENTED_EDGE('',*,*,#11895,.T.);
#16838=ORIENTED_EDGE('',*,*,#11900,.T.);
#16839=ORIENTED_EDGE('',*,*,#11901,.F.);
#16840=ORIENTED_EDGE('',*,*,#11902,.T.);
#16841=ORIENTED_EDGE('',*,*,#11898,.T.);
#16842=ORIENTED_EDGE('',*,*,#11903,.T.);
#16843=ORIENTED_EDGE('',*,*,#11904,.F.);
#16844=ORIENTED_EDGE('',*,*,#11905,.T.);
#16845=ORIENTED_EDGE('',*,*,#11901,.T.);
#16846=ORIENTED_EDGE('',*,*,#11906,.T.);
#16847=ORIENTED_EDGE('',*,*,#11907,.F.);
#16848=ORIENTED_EDGE('',*,*,#11908,.T.);
#16849=ORIENTED_EDGE('',*,*,#11904,.T.);
#16850=ORIENTED_EDGE('',*,*,#11909,.T.);
#16851=ORIENTED_EDGE('',*,*,#11910,.F.);
#16852=ORIENTED_EDGE('',*,*,#11911,.T.);
#16853=ORIENTED_EDGE('',*,*,#11912,.T.);
#16854=ORIENTED_EDGE('',*,*,#11907,.T.);
#16855=ORIENTED_EDGE('',*,*,#11913,.T.);
#16856=ORIENTED_EDGE('',*,*,#11914,.F.);
#16857=ORIENTED_EDGE('',*,*,#11915,.T.);
#16858=ORIENTED_EDGE('',*,*,#11916,.T.);
#16859=ORIENTED_EDGE('',*,*,#11917,.F.);
#16860=ORIENTED_EDGE('',*,*,#11916,.F.);
#16861=ORIENTED_EDGE('',*,*,#11918,.T.);
#16862=ORIENTED_EDGE('',*,*,#11919,.T.);
#16863=ORIENTED_EDGE('',*,*,#11920,.T.);
#16864=ORIENTED_EDGE('',*,*,#11921,.F.);
#16865=ORIENTED_EDGE('',*,*,#11922,.T.);
#16866=ORIENTED_EDGE('',*,*,#11914,.T.);
#16867=ORIENTED_EDGE('',*,*,#11923,.T.);
#16868=ORIENTED_EDGE('',*,*,#11924,.F.);
#16869=ORIENTED_EDGE('',*,*,#11925,.T.);
#16870=ORIENTED_EDGE('',*,*,#11921,.T.);
#16871=ORIENTED_EDGE('',*,*,#11926,.T.);
#16872=ORIENTED_EDGE('',*,*,#11927,.F.);
#16873=ORIENTED_EDGE('',*,*,#11928,.T.);
#16874=ORIENTED_EDGE('',*,*,#11924,.T.);
#16875=ORIENTED_EDGE('',*,*,#11929,.T.);
#16876=ORIENTED_EDGE('',*,*,#11930,.F.);
#16877=ORIENTED_EDGE('',*,*,#11931,.T.);
#16878=ORIENTED_EDGE('',*,*,#11927,.T.);
#16879=ORIENTED_EDGE('',*,*,#11932,.T.);
#16880=ORIENTED_EDGE('',*,*,#11933,.F.);
#16881=ORIENTED_EDGE('',*,*,#11934,.T.);
#16882=ORIENTED_EDGE('',*,*,#11930,.T.);
#16883=ORIENTED_EDGE('',*,*,#11935,.T.);
#16884=ORIENTED_EDGE('',*,*,#11936,.F.);
#16885=ORIENTED_EDGE('',*,*,#11937,.T.);
#16886=ORIENTED_EDGE('',*,*,#11933,.T.);
#16887=ORIENTED_EDGE('',*,*,#11938,.T.);
#16888=ORIENTED_EDGE('',*,*,#11939,.F.);
#16889=ORIENTED_EDGE('',*,*,#11940,.T.);
#16890=ORIENTED_EDGE('',*,*,#11936,.T.);
#16891=ORIENTED_EDGE('',*,*,#11941,.T.);
#16892=ORIENTED_EDGE('',*,*,#11942,.F.);
#16893=ORIENTED_EDGE('',*,*,#11943,.T.);
#16894=ORIENTED_EDGE('',*,*,#11939,.T.);
#16895=ORIENTED_EDGE('',*,*,#11944,.T.);
#16896=ORIENTED_EDGE('',*,*,#11945,.F.);
#16897=ORIENTED_EDGE('',*,*,#11946,.F.);
#16898=ORIENTED_EDGE('',*,*,#11947,.T.);
#16899=ORIENTED_EDGE('',*,*,#11942,.T.);
#16900=ORIENTED_EDGE('',*,*,#11948,.T.);
#16901=ORIENTED_EDGE('',*,*,#11949,.F.);
#16902=ORIENTED_EDGE('',*,*,#11950,.T.);
#16903=ORIENTED_EDGE('',*,*,#11951,.F.);
#16904=ORIENTED_EDGE('',*,*,#11952,.F.);
#16905=ORIENTED_EDGE('',*,*,#11953,.F.);
#16906=ORIENTED_EDGE('',*,*,#11954,.T.);
#16907=ORIENTED_EDGE('',*,*,#11949,.T.);
#16908=ORIENTED_EDGE('',*,*,#11955,.F.);
#16909=ORIENTED_EDGE('',*,*,#11956,.F.);
#16910=ORIENTED_EDGE('',*,*,#11957,.T.);
#16911=ORIENTED_EDGE('',*,*,#11953,.T.);
#16912=ORIENTED_EDGE('',*,*,#11958,.F.);
#16913=ORIENTED_EDGE('',*,*,#11959,.F.);
#16914=ORIENTED_EDGE('',*,*,#11960,.T.);
#16915=ORIENTED_EDGE('',*,*,#11956,.T.);
#16916=ORIENTED_EDGE('',*,*,#11961,.F.);
#16917=ORIENTED_EDGE('',*,*,#11962,.F.);
#16918=ORIENTED_EDGE('',*,*,#11963,.T.);
#16919=ORIENTED_EDGE('',*,*,#11959,.T.);
#16920=ORIENTED_EDGE('',*,*,#11964,.F.);
#16921=ORIENTED_EDGE('',*,*,#11965,.F.);
#16922=ORIENTED_EDGE('',*,*,#11966,.T.);
#16923=ORIENTED_EDGE('',*,*,#11962,.T.);
#16924=ORIENTED_EDGE('',*,*,#11967,.F.);
#16925=ORIENTED_EDGE('',*,*,#11968,.F.);
#16926=ORIENTED_EDGE('',*,*,#11969,.T.);
#16927=ORIENTED_EDGE('',*,*,#11965,.T.);
#16928=ORIENTED_EDGE('',*,*,#11970,.F.);
#16929=ORIENTED_EDGE('',*,*,#11971,.F.);
#16930=ORIENTED_EDGE('',*,*,#11972,.T.);
#16931=ORIENTED_EDGE('',*,*,#11968,.T.);
#16932=ORIENTED_EDGE('',*,*,#11973,.F.);
#16933=ORIENTED_EDGE('',*,*,#11974,.F.);
#16934=ORIENTED_EDGE('',*,*,#11975,.T.);
#16935=ORIENTED_EDGE('',*,*,#11971,.T.);
#16936=ORIENTED_EDGE('',*,*,#11976,.F.);
#16937=ORIENTED_EDGE('',*,*,#11977,.F.);
#16938=ORIENTED_EDGE('',*,*,#11978,.T.);
#16939=ORIENTED_EDGE('',*,*,#11974,.T.);
#16940=ORIENTED_EDGE('',*,*,#11979,.F.);
#16941=ORIENTED_EDGE('',*,*,#11980,.F.);
#16942=ORIENTED_EDGE('',*,*,#11981,.T.);
#16943=ORIENTED_EDGE('',*,*,#11982,.T.);
#16944=ORIENTED_EDGE('',*,*,#11983,.F.);
#16945=ORIENTED_EDGE('',*,*,#11984,.F.);
#16946=ORIENTED_EDGE('',*,*,#11985,.T.);
#16947=ORIENTED_EDGE('',*,*,#11980,.T.);
#16948=ORIENTED_EDGE('',*,*,#11986,.F.);
#16949=ORIENTED_EDGE('',*,*,#11987,.F.);
#16950=ORIENTED_EDGE('',*,*,#11988,.T.);
#16951=ORIENTED_EDGE('',*,*,#11984,.T.);
#16952=ORIENTED_EDGE('',*,*,#11989,.F.);
#16953=ORIENTED_EDGE('',*,*,#11990,.F.);
#16954=ORIENTED_EDGE('',*,*,#11991,.T.);
#16955=ORIENTED_EDGE('',*,*,#11987,.T.);
#16956=ORIENTED_EDGE('',*,*,#11992,.F.);
#16957=ORIENTED_EDGE('',*,*,#11993,.F.);
#16958=ORIENTED_EDGE('',*,*,#11994,.T.);
#16959=ORIENTED_EDGE('',*,*,#11990,.T.);
#16960=ORIENTED_EDGE('',*,*,#11995,.F.);
#16961=ORIENTED_EDGE('',*,*,#11996,.F.);
#16962=ORIENTED_EDGE('',*,*,#11997,.T.);
#16963=ORIENTED_EDGE('',*,*,#11993,.T.);
#16964=ORIENTED_EDGE('',*,*,#11998,.F.);
#16965=ORIENTED_EDGE('',*,*,#11999,.F.);
#16966=ORIENTED_EDGE('',*,*,#12000,.T.);
#16967=ORIENTED_EDGE('',*,*,#11996,.T.);
#16968=ORIENTED_EDGE('',*,*,#12001,.F.);
#16969=ORIENTED_EDGE('',*,*,#12002,.F.);
#16970=ORIENTED_EDGE('',*,*,#12003,.T.);
#16971=ORIENTED_EDGE('',*,*,#11999,.T.);
#16972=ORIENTED_EDGE('',*,*,#12004,.F.);
#16973=ORIENTED_EDGE('',*,*,#12005,.F.);
#16974=ORIENTED_EDGE('',*,*,#12006,.T.);
#16975=ORIENTED_EDGE('',*,*,#12002,.T.);
#16976=ORIENTED_EDGE('',*,*,#12007,.F.);
#16977=ORIENTED_EDGE('',*,*,#12008,.F.);
#16978=ORIENTED_EDGE('',*,*,#12009,.T.);
#16979=ORIENTED_EDGE('',*,*,#12005,.T.);
#16980=ORIENTED_EDGE('',*,*,#12010,.F.);
#16981=ORIENTED_EDGE('',*,*,#12011,.F.);
#16982=ORIENTED_EDGE('',*,*,#12012,.T.);
#16983=ORIENTED_EDGE('',*,*,#12008,.T.);
#16984=ORIENTED_EDGE('',*,*,#12013,.F.);
#16985=ORIENTED_EDGE('',*,*,#12014,.F.);
#16986=ORIENTED_EDGE('',*,*,#12015,.T.);
#16987=ORIENTED_EDGE('',*,*,#12011,.T.);
#16988=ORIENTED_EDGE('',*,*,#12016,.F.);
#16989=ORIENTED_EDGE('',*,*,#12017,.F.);
#16990=ORIENTED_EDGE('',*,*,#12018,.T.);
#16991=ORIENTED_EDGE('',*,*,#12014,.T.);
#16992=ORIENTED_EDGE('',*,*,#12019,.F.);
#16993=ORIENTED_EDGE('',*,*,#12020,.F.);
#16994=ORIENTED_EDGE('',*,*,#12021,.T.);
#16995=ORIENTED_EDGE('',*,*,#12017,.T.);
#16996=ORIENTED_EDGE('',*,*,#12022,.F.);
#16997=ORIENTED_EDGE('',*,*,#12023,.F.);
#16998=ORIENTED_EDGE('',*,*,#12024,.T.);
#16999=ORIENTED_EDGE('',*,*,#12020,.T.);
#17000=ORIENTED_EDGE('',*,*,#12025,.F.);
#17001=ORIENTED_EDGE('',*,*,#12026,.F.);
#17002=ORIENTED_EDGE('',*,*,#12027,.T.);
#17003=ORIENTED_EDGE('',*,*,#12023,.T.);
#17004=ORIENTED_EDGE('',*,*,#12028,.F.);
#17005=ORIENTED_EDGE('',*,*,#12029,.F.);
#17006=ORIENTED_EDGE('',*,*,#12030,.T.);
#17007=ORIENTED_EDGE('',*,*,#12026,.T.);
#17008=ORIENTED_EDGE('',*,*,#12031,.F.);
#17009=ORIENTED_EDGE('',*,*,#12032,.F.);
#17010=ORIENTED_EDGE('',*,*,#12033,.T.);
#17011=ORIENTED_EDGE('',*,*,#12029,.T.);
#17012=ORIENTED_EDGE('',*,*,#12034,.F.);
#17013=ORIENTED_EDGE('',*,*,#12035,.F.);
#17014=ORIENTED_EDGE('',*,*,#12036,.T.);
#17015=ORIENTED_EDGE('',*,*,#12032,.T.);
#17016=ORIENTED_EDGE('',*,*,#12037,.F.);
#17017=ORIENTED_EDGE('',*,*,#12038,.F.);
#17018=ORIENTED_EDGE('',*,*,#12039,.T.);
#17019=ORIENTED_EDGE('',*,*,#12035,.T.);
#17020=ORIENTED_EDGE('',*,*,#12040,.F.);
#17021=ORIENTED_EDGE('',*,*,#12041,.F.);
#17022=ORIENTED_EDGE('',*,*,#12042,.T.);
#17023=ORIENTED_EDGE('',*,*,#12038,.T.);
#17024=ORIENTED_EDGE('',*,*,#12043,.F.);
#17025=ORIENTED_EDGE('',*,*,#12044,.F.);
#17026=ORIENTED_EDGE('',*,*,#12045,.T.);
#17027=ORIENTED_EDGE('',*,*,#12041,.T.);
#17028=ORIENTED_EDGE('',*,*,#12046,.F.);
#17029=ORIENTED_EDGE('',*,*,#12047,.F.);
#17030=ORIENTED_EDGE('',*,*,#12048,.T.);
#17031=ORIENTED_EDGE('',*,*,#12044,.T.);
#17032=ORIENTED_EDGE('',*,*,#12049,.F.);
#17033=ORIENTED_EDGE('',*,*,#12050,.F.);
#17034=ORIENTED_EDGE('',*,*,#12051,.T.);
#17035=ORIENTED_EDGE('',*,*,#12047,.T.);
#17036=ORIENTED_EDGE('',*,*,#12052,.F.);
#17037=ORIENTED_EDGE('',*,*,#12053,.F.);
#17038=ORIENTED_EDGE('',*,*,#12054,.T.);
#17039=ORIENTED_EDGE('',*,*,#12050,.T.);
#17040=ORIENTED_EDGE('',*,*,#12055,.F.);
#17041=ORIENTED_EDGE('',*,*,#12056,.F.);
#17042=ORIENTED_EDGE('',*,*,#12057,.T.);
#17043=ORIENTED_EDGE('',*,*,#12053,.T.);
#17044=ORIENTED_EDGE('',*,*,#12058,.F.);
#17045=ORIENTED_EDGE('',*,*,#12059,.F.);
#17046=ORIENTED_EDGE('',*,*,#12060,.T.);
#17047=ORIENTED_EDGE('',*,*,#12056,.T.);
#17048=ORIENTED_EDGE('',*,*,#12061,.F.);
#17049=ORIENTED_EDGE('',*,*,#12062,.F.);
#17050=ORIENTED_EDGE('',*,*,#12063,.T.);
#17051=ORIENTED_EDGE('',*,*,#12059,.T.);
#17052=ORIENTED_EDGE('',*,*,#12064,.F.);
#17053=ORIENTED_EDGE('',*,*,#12065,.F.);
#17054=ORIENTED_EDGE('',*,*,#12066,.T.);
#17055=ORIENTED_EDGE('',*,*,#12062,.T.);
#17056=ORIENTED_EDGE('',*,*,#12067,.F.);
#17057=ORIENTED_EDGE('',*,*,#12068,.F.);
#17058=ORIENTED_EDGE('',*,*,#12069,.T.);
#17059=ORIENTED_EDGE('',*,*,#12065,.T.);
#17060=ORIENTED_EDGE('',*,*,#12070,.F.);
#17061=ORIENTED_EDGE('',*,*,#12071,.F.);
#17062=ORIENTED_EDGE('',*,*,#12072,.T.);
#17063=ORIENTED_EDGE('',*,*,#12068,.T.);
#17064=ORIENTED_EDGE('',*,*,#12073,.F.);
#17065=ORIENTED_EDGE('',*,*,#12074,.F.);
#17066=ORIENTED_EDGE('',*,*,#12075,.T.);
#17067=ORIENTED_EDGE('',*,*,#12071,.T.);
#17068=ORIENTED_EDGE('',*,*,#12076,.F.);
#17069=ORIENTED_EDGE('',*,*,#12077,.F.);
#17070=ORIENTED_EDGE('',*,*,#12078,.T.);
#17071=ORIENTED_EDGE('',*,*,#12074,.T.);
#17072=ORIENTED_EDGE('',*,*,#12079,.F.);
#17073=ORIENTED_EDGE('',*,*,#12080,.F.);
#17074=ORIENTED_EDGE('',*,*,#12081,.T.);
#17075=ORIENTED_EDGE('',*,*,#12077,.T.);
#17076=ORIENTED_EDGE('',*,*,#12082,.F.);
#17077=ORIENTED_EDGE('',*,*,#12083,.F.);
#17078=ORIENTED_EDGE('',*,*,#12084,.T.);
#17079=ORIENTED_EDGE('',*,*,#12080,.T.);
#17080=ORIENTED_EDGE('',*,*,#12085,.F.);
#17081=ORIENTED_EDGE('',*,*,#12086,.F.);
#17082=ORIENTED_EDGE('',*,*,#12087,.T.);
#17083=ORIENTED_EDGE('',*,*,#12083,.T.);
#17084=ORIENTED_EDGE('',*,*,#12088,.F.);
#17085=ORIENTED_EDGE('',*,*,#12089,.F.);
#17086=ORIENTED_EDGE('',*,*,#12090,.T.);
#17087=ORIENTED_EDGE('',*,*,#12086,.T.);
#17088=ORIENTED_EDGE('',*,*,#12091,.F.);
#17089=ORIENTED_EDGE('',*,*,#12092,.F.);
#17090=ORIENTED_EDGE('',*,*,#12093,.T.);
#17091=ORIENTED_EDGE('',*,*,#12089,.T.);
#17092=ORIENTED_EDGE('',*,*,#12094,.F.);
#17093=ORIENTED_EDGE('',*,*,#12095,.F.);
#17094=ORIENTED_EDGE('',*,*,#12096,.T.);
#17095=ORIENTED_EDGE('',*,*,#12092,.T.);
#17096=ORIENTED_EDGE('',*,*,#12097,.F.);
#17097=ORIENTED_EDGE('',*,*,#12098,.F.);
#17098=ORIENTED_EDGE('',*,*,#12099,.T.);
#17099=ORIENTED_EDGE('',*,*,#12095,.T.);
#17100=ORIENTED_EDGE('',*,*,#12100,.F.);
#17101=ORIENTED_EDGE('',*,*,#12101,.F.);
#17102=ORIENTED_EDGE('',*,*,#12102,.T.);
#17103=ORIENTED_EDGE('',*,*,#12098,.T.);
#17104=ORIENTED_EDGE('',*,*,#12103,.F.);
#17105=ORIENTED_EDGE('',*,*,#12104,.F.);
#17106=ORIENTED_EDGE('',*,*,#12105,.T.);
#17107=ORIENTED_EDGE('',*,*,#12101,.T.);
#17108=ORIENTED_EDGE('',*,*,#12106,.F.);
#17109=ORIENTED_EDGE('',*,*,#12107,.F.);
#17110=ORIENTED_EDGE('',*,*,#12108,.T.);
#17111=ORIENTED_EDGE('',*,*,#12104,.T.);
#17112=ORIENTED_EDGE('',*,*,#12109,.F.);
#17113=ORIENTED_EDGE('',*,*,#12110,.F.);
#17114=ORIENTED_EDGE('',*,*,#12111,.T.);
#17115=ORIENTED_EDGE('',*,*,#12107,.T.);
#17116=ORIENTED_EDGE('',*,*,#12112,.F.);
#17117=ORIENTED_EDGE('',*,*,#12113,.F.);
#17118=ORIENTED_EDGE('',*,*,#12114,.T.);
#17119=ORIENTED_EDGE('',*,*,#12110,.T.);
#17120=ORIENTED_EDGE('',*,*,#12115,.F.);
#17121=ORIENTED_EDGE('',*,*,#12116,.F.);
#17122=ORIENTED_EDGE('',*,*,#12117,.T.);
#17123=ORIENTED_EDGE('',*,*,#12113,.T.);
#17124=ORIENTED_EDGE('',*,*,#12118,.F.);
#17125=ORIENTED_EDGE('',*,*,#12119,.F.);
#17126=ORIENTED_EDGE('',*,*,#12120,.T.);
#17127=ORIENTED_EDGE('',*,*,#12116,.T.);
#17128=ORIENTED_EDGE('',*,*,#12121,.F.);
#17129=ORIENTED_EDGE('',*,*,#12122,.F.);
#17130=ORIENTED_EDGE('',*,*,#12123,.T.);
#17131=ORIENTED_EDGE('',*,*,#12119,.T.);
#17132=ORIENTED_EDGE('',*,*,#12124,.F.);
#17133=ORIENTED_EDGE('',*,*,#12125,.F.);
#17134=ORIENTED_EDGE('',*,*,#12126,.T.);
#17135=ORIENTED_EDGE('',*,*,#12122,.T.);
#17136=ORIENTED_EDGE('',*,*,#12127,.F.);
#17137=ORIENTED_EDGE('',*,*,#12128,.F.);
#17138=ORIENTED_EDGE('',*,*,#12129,.T.);
#17139=ORIENTED_EDGE('',*,*,#12125,.T.);
#17140=ORIENTED_EDGE('',*,*,#12130,.F.);
#17141=ORIENTED_EDGE('',*,*,#12131,.F.);
#17142=ORIENTED_EDGE('',*,*,#12132,.T.);
#17143=ORIENTED_EDGE('',*,*,#12128,.T.);
#17144=ORIENTED_EDGE('',*,*,#12133,.F.);
#17145=ORIENTED_EDGE('',*,*,#12134,.F.);
#17146=ORIENTED_EDGE('',*,*,#12135,.T.);
#17147=ORIENTED_EDGE('',*,*,#12131,.T.);
#17148=ORIENTED_EDGE('',*,*,#12136,.F.);
#17149=ORIENTED_EDGE('',*,*,#12137,.F.);
#17150=ORIENTED_EDGE('',*,*,#12138,.T.);
#17151=ORIENTED_EDGE('',*,*,#12134,.T.);
#17152=ORIENTED_EDGE('',*,*,#12139,.F.);
#17153=ORIENTED_EDGE('',*,*,#12140,.F.);
#17154=ORIENTED_EDGE('',*,*,#12141,.T.);
#17155=ORIENTED_EDGE('',*,*,#12137,.T.);
#17156=ORIENTED_EDGE('',*,*,#12142,.F.);
#17157=ORIENTED_EDGE('',*,*,#12143,.F.);
#17158=ORIENTED_EDGE('',*,*,#12144,.T.);
#17159=ORIENTED_EDGE('',*,*,#12140,.T.);
#17160=ORIENTED_EDGE('',*,*,#12145,.F.);
#17161=ORIENTED_EDGE('',*,*,#12146,.F.);
#17162=ORIENTED_EDGE('',*,*,#12147,.T.);
#17163=ORIENTED_EDGE('',*,*,#12143,.T.);
#17164=ORIENTED_EDGE('',*,*,#12148,.F.);
#17165=ORIENTED_EDGE('',*,*,#12149,.F.);
#17166=ORIENTED_EDGE('',*,*,#12150,.T.);
#17167=ORIENTED_EDGE('',*,*,#12146,.T.);
#17168=ORIENTED_EDGE('',*,*,#12151,.F.);
#17169=ORIENTED_EDGE('',*,*,#12152,.F.);
#17170=ORIENTED_EDGE('',*,*,#12153,.T.);
#17171=ORIENTED_EDGE('',*,*,#12149,.T.);
#17172=ORIENTED_EDGE('',*,*,#12154,.F.);
#17173=ORIENTED_EDGE('',*,*,#12155,.F.);
#17174=ORIENTED_EDGE('',*,*,#12156,.T.);
#17175=ORIENTED_EDGE('',*,*,#12152,.T.);
#17176=ORIENTED_EDGE('',*,*,#12157,.F.);
#17177=ORIENTED_EDGE('',*,*,#12158,.F.);
#17178=ORIENTED_EDGE('',*,*,#12159,.T.);
#17179=ORIENTED_EDGE('',*,*,#12155,.T.);
#17180=ORIENTED_EDGE('',*,*,#12160,.F.);
#17181=ORIENTED_EDGE('',*,*,#12161,.F.);
#17182=ORIENTED_EDGE('',*,*,#12162,.T.);
#17183=ORIENTED_EDGE('',*,*,#12158,.T.);
#17184=ORIENTED_EDGE('',*,*,#12163,.F.);
#17185=ORIENTED_EDGE('',*,*,#12164,.F.);
#17186=ORIENTED_EDGE('',*,*,#12165,.T.);
#17187=ORIENTED_EDGE('',*,*,#12161,.T.);
#17188=ORIENTED_EDGE('',*,*,#12166,.F.);
#17189=ORIENTED_EDGE('',*,*,#12167,.F.);
#17190=ORIENTED_EDGE('',*,*,#12168,.T.);
#17191=ORIENTED_EDGE('',*,*,#12164,.T.);
#17192=ORIENTED_EDGE('',*,*,#12169,.F.);
#17193=ORIENTED_EDGE('',*,*,#12170,.F.);
#17194=ORIENTED_EDGE('',*,*,#12171,.T.);
#17195=ORIENTED_EDGE('',*,*,#12167,.T.);
#17196=ORIENTED_EDGE('',*,*,#12172,.F.);
#17197=ORIENTED_EDGE('',*,*,#12173,.F.);
#17198=ORIENTED_EDGE('',*,*,#12174,.T.);
#17199=ORIENTED_EDGE('',*,*,#12170,.T.);
#17200=ORIENTED_EDGE('',*,*,#12175,.F.);
#17201=ORIENTED_EDGE('',*,*,#12176,.F.);
#17202=ORIENTED_EDGE('',*,*,#12177,.T.);
#17203=ORIENTED_EDGE('',*,*,#12173,.T.);
#17204=ORIENTED_EDGE('',*,*,#12178,.F.);
#17205=ORIENTED_EDGE('',*,*,#12179,.F.);
#17206=ORIENTED_EDGE('',*,*,#12180,.T.);
#17207=ORIENTED_EDGE('',*,*,#12176,.T.);
#17208=ORIENTED_EDGE('',*,*,#12181,.F.);
#17209=ORIENTED_EDGE('',*,*,#12182,.F.);
#17210=ORIENTED_EDGE('',*,*,#12183,.T.);
#17211=ORIENTED_EDGE('',*,*,#12179,.T.);
#17212=ORIENTED_EDGE('',*,*,#12184,.F.);
#17213=ORIENTED_EDGE('',*,*,#12185,.F.);
#17214=ORIENTED_EDGE('',*,*,#12186,.T.);
#17215=ORIENTED_EDGE('',*,*,#12182,.T.);
#17216=ORIENTED_EDGE('',*,*,#12187,.F.);
#17217=ORIENTED_EDGE('',*,*,#12188,.F.);
#17218=ORIENTED_EDGE('',*,*,#12189,.T.);
#17219=ORIENTED_EDGE('',*,*,#12185,.T.);
#17220=ORIENTED_EDGE('',*,*,#12190,.F.);
#17221=ORIENTED_EDGE('',*,*,#12191,.F.);
#17222=ORIENTED_EDGE('',*,*,#12192,.T.);
#17223=ORIENTED_EDGE('',*,*,#12188,.T.);
#17224=ORIENTED_EDGE('',*,*,#12193,.F.);
#17225=ORIENTED_EDGE('',*,*,#12194,.F.);
#17226=ORIENTED_EDGE('',*,*,#12195,.T.);
#17227=ORIENTED_EDGE('',*,*,#12191,.T.);
#17228=ORIENTED_EDGE('',*,*,#12196,.F.);
#17229=ORIENTED_EDGE('',*,*,#12197,.F.);
#17230=ORIENTED_EDGE('',*,*,#12198,.T.);
#17231=ORIENTED_EDGE('',*,*,#12194,.T.);
#17232=ORIENTED_EDGE('',*,*,#12199,.F.);
#17233=ORIENTED_EDGE('',*,*,#12200,.F.);
#17234=ORIENTED_EDGE('',*,*,#12201,.T.);
#17235=ORIENTED_EDGE('',*,*,#12197,.T.);
#17236=ORIENTED_EDGE('',*,*,#12202,.F.);
#17237=ORIENTED_EDGE('',*,*,#12203,.F.);
#17238=ORIENTED_EDGE('',*,*,#12204,.T.);
#17239=ORIENTED_EDGE('',*,*,#12200,.T.);
#17240=ORIENTED_EDGE('',*,*,#12205,.F.);
#17241=ORIENTED_EDGE('',*,*,#12206,.F.);
#17242=ORIENTED_EDGE('',*,*,#12207,.T.);
#17243=ORIENTED_EDGE('',*,*,#12203,.T.);
#17244=ORIENTED_EDGE('',*,*,#12208,.F.);
#17245=ORIENTED_EDGE('',*,*,#12209,.F.);
#17246=ORIENTED_EDGE('',*,*,#12210,.T.);
#17247=ORIENTED_EDGE('',*,*,#12206,.T.);
#17248=ORIENTED_EDGE('',*,*,#12211,.F.);
#17249=ORIENTED_EDGE('',*,*,#12212,.F.);
#17250=ORIENTED_EDGE('',*,*,#12213,.T.);
#17251=ORIENTED_EDGE('',*,*,#12209,.T.);
#17252=ORIENTED_EDGE('',*,*,#12214,.F.);
#17253=ORIENTED_EDGE('',*,*,#12215,.F.);
#17254=ORIENTED_EDGE('',*,*,#12216,.T.);
#17255=ORIENTED_EDGE('',*,*,#12212,.T.);
#17256=ORIENTED_EDGE('',*,*,#12217,.F.);
#17257=ORIENTED_EDGE('',*,*,#12218,.F.);
#17258=ORIENTED_EDGE('',*,*,#12219,.T.);
#17259=ORIENTED_EDGE('',*,*,#12215,.T.);
#17260=ORIENTED_EDGE('',*,*,#12220,.F.);
#17261=ORIENTED_EDGE('',*,*,#12221,.F.);
#17262=ORIENTED_EDGE('',*,*,#12222,.T.);
#17263=ORIENTED_EDGE('',*,*,#12218,.T.);
#17264=ORIENTED_EDGE('',*,*,#12223,.F.);
#17265=ORIENTED_EDGE('',*,*,#12224,.F.);
#17266=ORIENTED_EDGE('',*,*,#12225,.T.);
#17267=ORIENTED_EDGE('',*,*,#12221,.T.);
#17268=ORIENTED_EDGE('',*,*,#12226,.F.);
#17269=ORIENTED_EDGE('',*,*,#12227,.F.);
#17270=ORIENTED_EDGE('',*,*,#12228,.T.);
#17271=ORIENTED_EDGE('',*,*,#12224,.T.);
#17272=ORIENTED_EDGE('',*,*,#12229,.F.);
#17273=ORIENTED_EDGE('',*,*,#12230,.F.);
#17274=ORIENTED_EDGE('',*,*,#12231,.T.);
#17275=ORIENTED_EDGE('',*,*,#12227,.T.);
#17276=ORIENTED_EDGE('',*,*,#12232,.F.);
#17277=ORIENTED_EDGE('',*,*,#12233,.F.);
#17278=ORIENTED_EDGE('',*,*,#12234,.T.);
#17279=ORIENTED_EDGE('',*,*,#12230,.T.);
#17280=ORIENTED_EDGE('',*,*,#12235,.F.);
#17281=ORIENTED_EDGE('',*,*,#12236,.F.);
#17282=ORIENTED_EDGE('',*,*,#12237,.T.);
#17283=ORIENTED_EDGE('',*,*,#12233,.T.);
#17284=ORIENTED_EDGE('',*,*,#12238,.F.);
#17285=ORIENTED_EDGE('',*,*,#12239,.F.);
#17286=ORIENTED_EDGE('',*,*,#12240,.T.);
#17287=ORIENTED_EDGE('',*,*,#12236,.T.);
#17288=ORIENTED_EDGE('',*,*,#12241,.F.);
#17289=ORIENTED_EDGE('',*,*,#12242,.F.);
#17290=ORIENTED_EDGE('',*,*,#12243,.T.);
#17291=ORIENTED_EDGE('',*,*,#12239,.T.);
#17292=ORIENTED_EDGE('',*,*,#12244,.F.);
#17293=ORIENTED_EDGE('',*,*,#12245,.F.);
#17294=ORIENTED_EDGE('',*,*,#12246,.T.);
#17295=ORIENTED_EDGE('',*,*,#12242,.T.);
#17296=ORIENTED_EDGE('',*,*,#12247,.F.);
#17297=ORIENTED_EDGE('',*,*,#12248,.F.);
#17298=ORIENTED_EDGE('',*,*,#12249,.T.);
#17299=ORIENTED_EDGE('',*,*,#12245,.T.);
#17300=ORIENTED_EDGE('',*,*,#12250,.F.);
#17301=ORIENTED_EDGE('',*,*,#12251,.F.);
#17302=ORIENTED_EDGE('',*,*,#12252,.T.);
#17303=ORIENTED_EDGE('',*,*,#12248,.T.);
#17304=ORIENTED_EDGE('',*,*,#12253,.F.);
#17305=ORIENTED_EDGE('',*,*,#12254,.F.);
#17306=ORIENTED_EDGE('',*,*,#12255,.T.);
#17307=ORIENTED_EDGE('',*,*,#12251,.T.);
#17308=ORIENTED_EDGE('',*,*,#12256,.F.);
#17309=ORIENTED_EDGE('',*,*,#12257,.F.);
#17310=ORIENTED_EDGE('',*,*,#12258,.T.);
#17311=ORIENTED_EDGE('',*,*,#12254,.T.);
#17312=ORIENTED_EDGE('',*,*,#12259,.F.);
#17313=ORIENTED_EDGE('',*,*,#12260,.F.);
#17314=ORIENTED_EDGE('',*,*,#12261,.T.);
#17315=ORIENTED_EDGE('',*,*,#12257,.T.);
#17316=ORIENTED_EDGE('',*,*,#12262,.F.);
#17317=ORIENTED_EDGE('',*,*,#12263,.F.);
#17318=ORIENTED_EDGE('',*,*,#12264,.T.);
#17319=ORIENTED_EDGE('',*,*,#12260,.T.);
#17320=ORIENTED_EDGE('',*,*,#12265,.F.);
#17321=ORIENTED_EDGE('',*,*,#12266,.F.);
#17322=ORIENTED_EDGE('',*,*,#12267,.T.);
#17323=ORIENTED_EDGE('',*,*,#12263,.T.);
#17324=ORIENTED_EDGE('',*,*,#12268,.F.);
#17325=ORIENTED_EDGE('',*,*,#12269,.F.);
#17326=ORIENTED_EDGE('',*,*,#12270,.T.);
#17327=ORIENTED_EDGE('',*,*,#12266,.T.);
#17328=ORIENTED_EDGE('',*,*,#12271,.F.);
#17329=ORIENTED_EDGE('',*,*,#12272,.F.);
#17330=ORIENTED_EDGE('',*,*,#12273,.T.);
#17331=ORIENTED_EDGE('',*,*,#12269,.T.);
#17332=ORIENTED_EDGE('',*,*,#12274,.F.);
#17333=ORIENTED_EDGE('',*,*,#12275,.F.);
#17334=ORIENTED_EDGE('',*,*,#12276,.T.);
#17335=ORIENTED_EDGE('',*,*,#12272,.T.);
#17336=ORIENTED_EDGE('',*,*,#12277,.F.);
#17337=ORIENTED_EDGE('',*,*,#12278,.F.);
#17338=ORIENTED_EDGE('',*,*,#12279,.T.);
#17339=ORIENTED_EDGE('',*,*,#12275,.T.);
#17340=ORIENTED_EDGE('',*,*,#12280,.F.);
#17341=ORIENTED_EDGE('',*,*,#12281,.T.);
#17342=ORIENTED_EDGE('',*,*,#12282,.T.);
#17343=ORIENTED_EDGE('',*,*,#12283,.T.);
#17344=ORIENTED_EDGE('',*,*,#12282,.F.);
#17345=ORIENTED_EDGE('',*,*,#12281,.F.);
#17346=ORIENTED_EDGE('',*,*,#12284,.T.);
#17347=ORIENTED_EDGE('',*,*,#12285,.T.);
#17348=ORIENTED_EDGE('',*,*,#12284,.F.);
#17349=ORIENTED_EDGE('',*,*,#12283,.F.);
#17350=ORIENTED_EDGE('',*,*,#12286,.T.);
#17351=ORIENTED_EDGE('',*,*,#12287,.T.);
#17352=ORIENTED_EDGE('',*,*,#12288,.T.);
#17353=ORIENTED_EDGE('',*,*,#12287,.F.);
#17354=ORIENTED_EDGE('',*,*,#12288,.F.);
#17355=ORIENTED_EDGE('',*,*,#12289,.T.);
#17356=ORIENTED_EDGE('',*,*,#12290,.T.);
#17357=ORIENTED_EDGE('',*,*,#12289,.F.);
#17358=ORIENTED_EDGE('',*,*,#12286,.F.);
#17359=ORIENTED_EDGE('',*,*,#12291,.F.);
#17360=ORIENTED_EDGE('',*,*,#11982,.F.);
#17361=ORIENTED_EDGE('',*,*,#12292,.F.);
#17362=ORIENTED_EDGE('',*,*,#11911,.F.);
#17363=ORIENTED_EDGE('',*,*,#12293,.F.);
#17364=ORIENTED_EDGE('',*,*,#12290,.F.);
#17365=ORIENTED_EDGE('',*,*,#12294,.F.);
#17366=ORIENTED_EDGE('',*,*,#12295,.F.);
#17367=ORIENTED_EDGE('',*,*,#11610,.F.);
#17368=ORIENTED_EDGE('',*,*,#11614,.F.);
#17369=ORIENTED_EDGE('',*,*,#11617,.F.);
#17370=ORIENTED_EDGE('',*,*,#11620,.F.);
#17371=ORIENTED_EDGE('',*,*,#11623,.F.);
#17372=ORIENTED_EDGE('',*,*,#11626,.F.);
#17373=ORIENTED_EDGE('',*,*,#11629,.F.);
#17374=ORIENTED_EDGE('',*,*,#11632,.F.);
#17375=ORIENTED_EDGE('',*,*,#11635,.F.);
#17376=ORIENTED_EDGE('',*,*,#11638,.F.);
#17377=ORIENTED_EDGE('',*,*,#11641,.F.);
#17378=ORIENTED_EDGE('',*,*,#11644,.F.);
#17379=ORIENTED_EDGE('',*,*,#11647,.F.);
#17380=ORIENTED_EDGE('',*,*,#11650,.F.);
#17381=ORIENTED_EDGE('',*,*,#11653,.F.);
#17382=ORIENTED_EDGE('',*,*,#11656,.F.);
#17383=ORIENTED_EDGE('',*,*,#11659,.F.);
#17384=ORIENTED_EDGE('',*,*,#11662,.F.);
#17385=ORIENTED_EDGE('',*,*,#11665,.F.);
#17386=ORIENTED_EDGE('',*,*,#11668,.F.);
#17387=ORIENTED_EDGE('',*,*,#11671,.F.);
#17388=ORIENTED_EDGE('',*,*,#11674,.F.);
#17389=ORIENTED_EDGE('',*,*,#11677,.F.);
#17390=ORIENTED_EDGE('',*,*,#11680,.F.);
#17391=ORIENTED_EDGE('',*,*,#11683,.F.);
#17392=ORIENTED_EDGE('',*,*,#11686,.F.);
#17393=ORIENTED_EDGE('',*,*,#11689,.F.);
#17394=ORIENTED_EDGE('',*,*,#11692,.F.);
#17395=ORIENTED_EDGE('',*,*,#11695,.F.);
#17396=ORIENTED_EDGE('',*,*,#11698,.F.);
#17397=ORIENTED_EDGE('',*,*,#11701,.F.);
#17398=ORIENTED_EDGE('',*,*,#11704,.F.);
#17399=ORIENTED_EDGE('',*,*,#11707,.F.);
#17400=ORIENTED_EDGE('',*,*,#11710,.F.);
#17401=ORIENTED_EDGE('',*,*,#11713,.F.);
#17402=ORIENTED_EDGE('',*,*,#11716,.F.);
#17403=ORIENTED_EDGE('',*,*,#11719,.F.);
#17404=ORIENTED_EDGE('',*,*,#11722,.F.);
#17405=ORIENTED_EDGE('',*,*,#11725,.F.);
#17406=ORIENTED_EDGE('',*,*,#11728,.F.);
#17407=ORIENTED_EDGE('',*,*,#11731,.F.);
#17408=ORIENTED_EDGE('',*,*,#11734,.F.);
#17409=ORIENTED_EDGE('',*,*,#11737,.F.);
#17410=ORIENTED_EDGE('',*,*,#11740,.F.);
#17411=ORIENTED_EDGE('',*,*,#11743,.F.);
#17412=ORIENTED_EDGE('',*,*,#11746,.F.);
#17413=ORIENTED_EDGE('',*,*,#11749,.F.);
#17414=ORIENTED_EDGE('',*,*,#11752,.F.);
#17415=ORIENTED_EDGE('',*,*,#11755,.F.);
#17416=ORIENTED_EDGE('',*,*,#11758,.F.);
#17417=ORIENTED_EDGE('',*,*,#11761,.F.);
#17418=ORIENTED_EDGE('',*,*,#11764,.F.);
#17419=ORIENTED_EDGE('',*,*,#11767,.F.);
#17420=ORIENTED_EDGE('',*,*,#11770,.F.);
#17421=ORIENTED_EDGE('',*,*,#11773,.F.);
#17422=ORIENTED_EDGE('',*,*,#11776,.F.);
#17423=ORIENTED_EDGE('',*,*,#11779,.F.);
#17424=ORIENTED_EDGE('',*,*,#11782,.F.);
#17425=ORIENTED_EDGE('',*,*,#11785,.F.);
#17426=ORIENTED_EDGE('',*,*,#11788,.F.);
#17427=ORIENTED_EDGE('',*,*,#11791,.F.);
#17428=ORIENTED_EDGE('',*,*,#11794,.F.);
#17429=ORIENTED_EDGE('',*,*,#11797,.F.);
#17430=ORIENTED_EDGE('',*,*,#11800,.F.);
#17431=ORIENTED_EDGE('',*,*,#11803,.F.);
#17432=ORIENTED_EDGE('',*,*,#11806,.F.);
#17433=ORIENTED_EDGE('',*,*,#11809,.F.);
#17434=ORIENTED_EDGE('',*,*,#11812,.F.);
#17435=ORIENTED_EDGE('',*,*,#11815,.F.);
#17436=ORIENTED_EDGE('',*,*,#11818,.F.);
#17437=ORIENTED_EDGE('',*,*,#11821,.F.);
#17438=ORIENTED_EDGE('',*,*,#11824,.F.);
#17439=ORIENTED_EDGE('',*,*,#11827,.F.);
#17440=ORIENTED_EDGE('',*,*,#11830,.F.);
#17441=ORIENTED_EDGE('',*,*,#11833,.F.);
#17442=ORIENTED_EDGE('',*,*,#11836,.F.);
#17443=ORIENTED_EDGE('',*,*,#11839,.F.);
#17444=ORIENTED_EDGE('',*,*,#11842,.F.);
#17445=ORIENTED_EDGE('',*,*,#11845,.F.);
#17446=ORIENTED_EDGE('',*,*,#11848,.F.);
#17447=ORIENTED_EDGE('',*,*,#11851,.F.);
#17448=ORIENTED_EDGE('',*,*,#11854,.F.);
#17449=ORIENTED_EDGE('',*,*,#11857,.F.);
#17450=ORIENTED_EDGE('',*,*,#11860,.F.);
#17451=ORIENTED_EDGE('',*,*,#11863,.F.);
#17452=ORIENTED_EDGE('',*,*,#11866,.F.);
#17453=ORIENTED_EDGE('',*,*,#11869,.F.);
#17454=ORIENTED_EDGE('',*,*,#11872,.F.);
#17455=ORIENTED_EDGE('',*,*,#11875,.F.);
#17456=ORIENTED_EDGE('',*,*,#11878,.F.);
#17457=ORIENTED_EDGE('',*,*,#11881,.F.);
#17458=ORIENTED_EDGE('',*,*,#11884,.F.);
#17459=ORIENTED_EDGE('',*,*,#11887,.F.);
#17460=ORIENTED_EDGE('',*,*,#11890,.F.);
#17461=ORIENTED_EDGE('',*,*,#11893,.F.);
#17462=ORIENTED_EDGE('',*,*,#11896,.F.);
#17463=ORIENTED_EDGE('',*,*,#11899,.F.);
#17464=ORIENTED_EDGE('',*,*,#11902,.F.);
#17465=ORIENTED_EDGE('',*,*,#11905,.F.);
#17466=ORIENTED_EDGE('',*,*,#11908,.F.);
#17467=ORIENTED_EDGE('',*,*,#11912,.F.);
#17468=ORIENTED_EDGE('',*,*,#12292,.T.);
#17469=ORIENTED_EDGE('',*,*,#11981,.F.);
#17470=ORIENTED_EDGE('',*,*,#11985,.F.);
#17471=ORIENTED_EDGE('',*,*,#11988,.F.);
#17472=ORIENTED_EDGE('',*,*,#11991,.F.);
#17473=ORIENTED_EDGE('',*,*,#11994,.F.);
#17474=ORIENTED_EDGE('',*,*,#11997,.F.);
#17475=ORIENTED_EDGE('',*,*,#12000,.F.);
#17476=ORIENTED_EDGE('',*,*,#12003,.F.);
#17477=ORIENTED_EDGE('',*,*,#12006,.F.);
#17478=ORIENTED_EDGE('',*,*,#12009,.F.);
#17479=ORIENTED_EDGE('',*,*,#12012,.F.);
#17480=ORIENTED_EDGE('',*,*,#12015,.F.);
#17481=ORIENTED_EDGE('',*,*,#12018,.F.);
#17482=ORIENTED_EDGE('',*,*,#12021,.F.);
#17483=ORIENTED_EDGE('',*,*,#12024,.F.);
#17484=ORIENTED_EDGE('',*,*,#12027,.F.);
#17485=ORIENTED_EDGE('',*,*,#12030,.F.);
#17486=ORIENTED_EDGE('',*,*,#12033,.F.);
#17487=ORIENTED_EDGE('',*,*,#12036,.F.);
#17488=ORIENTED_EDGE('',*,*,#12039,.F.);
#17489=ORIENTED_EDGE('',*,*,#12042,.F.);
#17490=ORIENTED_EDGE('',*,*,#12045,.F.);
#17491=ORIENTED_EDGE('',*,*,#12048,.F.);
#17492=ORIENTED_EDGE('',*,*,#12051,.F.);
#17493=ORIENTED_EDGE('',*,*,#12054,.F.);
#17494=ORIENTED_EDGE('',*,*,#12057,.F.);
#17495=ORIENTED_EDGE('',*,*,#12060,.F.);
#17496=ORIENTED_EDGE('',*,*,#12063,.F.);
#17497=ORIENTED_EDGE('',*,*,#12066,.F.);
#17498=ORIENTED_EDGE('',*,*,#12069,.F.);
#17499=ORIENTED_EDGE('',*,*,#12072,.F.);
#17500=ORIENTED_EDGE('',*,*,#12075,.F.);
#17501=ORIENTED_EDGE('',*,*,#12078,.F.);
#17502=ORIENTED_EDGE('',*,*,#12081,.F.);
#17503=ORIENTED_EDGE('',*,*,#12084,.F.);
#17504=ORIENTED_EDGE('',*,*,#12087,.F.);
#17505=ORIENTED_EDGE('',*,*,#12090,.F.);
#17506=ORIENTED_EDGE('',*,*,#12093,.F.);
#17507=ORIENTED_EDGE('',*,*,#12096,.F.);
#17508=ORIENTED_EDGE('',*,*,#12099,.F.);
#17509=ORIENTED_EDGE('',*,*,#12102,.F.);
#17510=ORIENTED_EDGE('',*,*,#12105,.F.);
#17511=ORIENTED_EDGE('',*,*,#12108,.F.);
#17512=ORIENTED_EDGE('',*,*,#12111,.F.);
#17513=ORIENTED_EDGE('',*,*,#12114,.F.);
#17514=ORIENTED_EDGE('',*,*,#12117,.F.);
#17515=ORIENTED_EDGE('',*,*,#12120,.F.);
#17516=ORIENTED_EDGE('',*,*,#12123,.F.);
#17517=ORIENTED_EDGE('',*,*,#12126,.F.);
#17518=ORIENTED_EDGE('',*,*,#12129,.F.);
#17519=ORIENTED_EDGE('',*,*,#12132,.F.);
#17520=ORIENTED_EDGE('',*,*,#12135,.F.);
#17521=ORIENTED_EDGE('',*,*,#12138,.F.);
#17522=ORIENTED_EDGE('',*,*,#12141,.F.);
#17523=ORIENTED_EDGE('',*,*,#12144,.F.);
#17524=ORIENTED_EDGE('',*,*,#12147,.F.);
#17525=ORIENTED_EDGE('',*,*,#12150,.F.);
#17526=ORIENTED_EDGE('',*,*,#12153,.F.);
#17527=ORIENTED_EDGE('',*,*,#12156,.F.);
#17528=ORIENTED_EDGE('',*,*,#12159,.F.);
#17529=ORIENTED_EDGE('',*,*,#12162,.F.);
#17530=ORIENTED_EDGE('',*,*,#12165,.F.);
#17531=ORIENTED_EDGE('',*,*,#12168,.F.);
#17532=ORIENTED_EDGE('',*,*,#12171,.F.);
#17533=ORIENTED_EDGE('',*,*,#12174,.F.);
#17534=ORIENTED_EDGE('',*,*,#12177,.F.);
#17535=ORIENTED_EDGE('',*,*,#12180,.F.);
#17536=ORIENTED_EDGE('',*,*,#12183,.F.);
#17537=ORIENTED_EDGE('',*,*,#12186,.F.);
#17538=ORIENTED_EDGE('',*,*,#12189,.F.);
#17539=ORIENTED_EDGE('',*,*,#12192,.F.);
#17540=ORIENTED_EDGE('',*,*,#12195,.F.);
#17541=ORIENTED_EDGE('',*,*,#12198,.F.);
#17542=ORIENTED_EDGE('',*,*,#12201,.F.);
#17543=ORIENTED_EDGE('',*,*,#12204,.F.);
#17544=ORIENTED_EDGE('',*,*,#12207,.F.);
#17545=ORIENTED_EDGE('',*,*,#12210,.F.);
#17546=ORIENTED_EDGE('',*,*,#12213,.F.);
#17547=ORIENTED_EDGE('',*,*,#12216,.F.);
#17548=ORIENTED_EDGE('',*,*,#12219,.F.);
#17549=ORIENTED_EDGE('',*,*,#12222,.F.);
#17550=ORIENTED_EDGE('',*,*,#12225,.F.);
#17551=ORIENTED_EDGE('',*,*,#12228,.F.);
#17552=ORIENTED_EDGE('',*,*,#12231,.F.);
#17553=ORIENTED_EDGE('',*,*,#12234,.F.);
#17554=ORIENTED_EDGE('',*,*,#12237,.F.);
#17555=ORIENTED_EDGE('',*,*,#12240,.F.);
#17556=ORIENTED_EDGE('',*,*,#12243,.F.);
#17557=ORIENTED_EDGE('',*,*,#12246,.F.);
#17558=ORIENTED_EDGE('',*,*,#12249,.F.);
#17559=ORIENTED_EDGE('',*,*,#12252,.F.);
#17560=ORIENTED_EDGE('',*,*,#12255,.F.);
#17561=ORIENTED_EDGE('',*,*,#12258,.F.);
#17562=ORIENTED_EDGE('',*,*,#12261,.F.);
#17563=ORIENTED_EDGE('',*,*,#12264,.F.);
#17564=ORIENTED_EDGE('',*,*,#12267,.F.);
#17565=ORIENTED_EDGE('',*,*,#12270,.F.);
#17566=ORIENTED_EDGE('',*,*,#12273,.F.);
#17567=ORIENTED_EDGE('',*,*,#12276,.F.);
#17568=ORIENTED_EDGE('',*,*,#12279,.F.);
#17569=ORIENTED_EDGE('',*,*,#12278,.T.);
#17570=ORIENTED_EDGE('',*,*,#12296,.F.);
#17571=ORIENTED_EDGE('',*,*,#12297,.F.);
#17572=ORIENTED_EDGE('',*,*,#12294,.T.);
#17573=ORIENTED_EDGE('',*,*,#12285,.F.);
#17574=ORIENTED_EDGE('',*,*,#11951,.T.);
#17575=ORIENTED_EDGE('',*,*,#12298,.T.);
#17576=ORIENTED_EDGE('',*,*,#11946,.T.);
#17577=ORIENTED_EDGE('',*,*,#12299,.T.);
#17578=ORIENTED_EDGE('',*,*,#12300,.T.);
#17579=ORIENTED_EDGE('',*,*,#12301,.T.);
#17580=ORIENTED_EDGE('',*,*,#11979,.T.);
#17581=ORIENTED_EDGE('',*,*,#11976,.T.);
#17582=ORIENTED_EDGE('',*,*,#11973,.T.);
#17583=ORIENTED_EDGE('',*,*,#11970,.T.);
#17584=ORIENTED_EDGE('',*,*,#11967,.T.);
#17585=ORIENTED_EDGE('',*,*,#11964,.T.);
#17586=ORIENTED_EDGE('',*,*,#11961,.T.);
#17587=ORIENTED_EDGE('',*,*,#11958,.T.);
#17588=ORIENTED_EDGE('',*,*,#11955,.T.);
#17589=ORIENTED_EDGE('',*,*,#11952,.T.);
#17590=ORIENTED_EDGE('',*,*,#12300,.F.);
#17591=ORIENTED_EDGE('',*,*,#12302,.F.);
#17592=ORIENTED_EDGE('',*,*,#11948,.F.);
#17593=ORIENTED_EDGE('',*,*,#11944,.F.);
#17594=ORIENTED_EDGE('',*,*,#11941,.F.);
#17595=ORIENTED_EDGE('',*,*,#11938,.F.);
#17596=ORIENTED_EDGE('',*,*,#11935,.F.);
#17597=ORIENTED_EDGE('',*,*,#11932,.F.);
#17598=ORIENTED_EDGE('',*,*,#11929,.F.);
#17599=ORIENTED_EDGE('',*,*,#11926,.F.);
#17600=ORIENTED_EDGE('',*,*,#11923,.F.);
#17601=ORIENTED_EDGE('',*,*,#11920,.F.);
#17602=ORIENTED_EDGE('',*,*,#12303,.F.);
#17603=ORIENTED_EDGE('',*,*,#11919,.F.);
#17604=ORIENTED_EDGE('',*,*,#12304,.T.);
#17605=ORIENTED_EDGE('',*,*,#12305,.T.);
#17606=ORIENTED_EDGE('',*,*,#12303,.T.);
#17607=ORIENTED_EDGE('',*,*,#11977,.T.);
#17608=ORIENTED_EDGE('',*,*,#12301,.F.);
#17609=ORIENTED_EDGE('',*,*,#12305,.F.);
#17610=ORIENTED_EDGE('',*,*,#12306,.T.);
#17611=ORIENTED_EDGE('',*,*,#12298,.F.);
#17612=ORIENTED_EDGE('',*,*,#11950,.F.);
#17613=ORIENTED_EDGE('',*,*,#11954,.F.);
#17614=ORIENTED_EDGE('',*,*,#11957,.F.);
#17615=ORIENTED_EDGE('',*,*,#11960,.F.);
#17616=ORIENTED_EDGE('',*,*,#11963,.F.);
#17617=ORIENTED_EDGE('',*,*,#11966,.F.);
#17618=ORIENTED_EDGE('',*,*,#11969,.F.);
#17619=ORIENTED_EDGE('',*,*,#11972,.F.);
#17620=ORIENTED_EDGE('',*,*,#11975,.F.);
#17621=ORIENTED_EDGE('',*,*,#11978,.F.);
#17622=ORIENTED_EDGE('',*,*,#12306,.F.);
#17623=ORIENTED_EDGE('',*,*,#12304,.F.);
#17624=ORIENTED_EDGE('',*,*,#11918,.F.);
#17625=ORIENTED_EDGE('',*,*,#11915,.F.);
#17626=ORIENTED_EDGE('',*,*,#11922,.F.);
#17627=ORIENTED_EDGE('',*,*,#11925,.F.);
#17628=ORIENTED_EDGE('',*,*,#11928,.F.);
#17629=ORIENTED_EDGE('',*,*,#11931,.F.);
#17630=ORIENTED_EDGE('',*,*,#11934,.F.);
#17631=ORIENTED_EDGE('',*,*,#11937,.F.);
#17632=ORIENTED_EDGE('',*,*,#11940,.F.);
#17633=ORIENTED_EDGE('',*,*,#11943,.F.);
#17634=ORIENTED_EDGE('',*,*,#11947,.F.);
#17635=ORIENTED_EDGE('',*,*,#11945,.T.);
#17636=ORIENTED_EDGE('',*,*,#12302,.T.);
#17637=ORIENTED_EDGE('',*,*,#12299,.F.);
#17638=ORIENTED_EDGE('',*,*,#12297,.T.);
#17639=ORIENTED_EDGE('',*,*,#12307,.T.);
#17640=ORIENTED_EDGE('',*,*,#11611,.T.);
#17641=ORIENTED_EDGE('',*,*,#12295,.T.);
#17642=ORIENTED_EDGE('',*,*,#11917,.T.);
#17643=ORIENTED_EDGE('',*,*,#12307,.F.);
#17644=ORIENTED_EDGE('',*,*,#12296,.T.);
#17645=ORIENTED_EDGE('',*,*,#12280,.T.);
#17646=ORIENTED_EDGE('',*,*,#12277,.T.);
#17647=ORIENTED_EDGE('',*,*,#12274,.T.);
#17648=ORIENTED_EDGE('',*,*,#12271,.T.);
#17649=ORIENTED_EDGE('',*,*,#12268,.T.);
#17650=ORIENTED_EDGE('',*,*,#12265,.T.);
#17651=ORIENTED_EDGE('',*,*,#12262,.T.);
#17652=ORIENTED_EDGE('',*,*,#12259,.T.);
#17653=ORIENTED_EDGE('',*,*,#12256,.T.);
#17654=ORIENTED_EDGE('',*,*,#12253,.T.);
#17655=ORIENTED_EDGE('',*,*,#12250,.T.);
#17656=ORIENTED_EDGE('',*,*,#12247,.T.);
#17657=ORIENTED_EDGE('',*,*,#12244,.T.);
#17658=ORIENTED_EDGE('',*,*,#12241,.T.);
#17659=ORIENTED_EDGE('',*,*,#12238,.T.);
#17660=ORIENTED_EDGE('',*,*,#12235,.T.);
#17661=ORIENTED_EDGE('',*,*,#12232,.T.);
#17662=ORIENTED_EDGE('',*,*,#12229,.T.);
#17663=ORIENTED_EDGE('',*,*,#12226,.T.);
#17664=ORIENTED_EDGE('',*,*,#12223,.T.);
#17665=ORIENTED_EDGE('',*,*,#12220,.T.);
#17666=ORIENTED_EDGE('',*,*,#12217,.T.);
#17667=ORIENTED_EDGE('',*,*,#12214,.T.);
#17668=ORIENTED_EDGE('',*,*,#12211,.T.);
#17669=ORIENTED_EDGE('',*,*,#12208,.T.);
#17670=ORIENTED_EDGE('',*,*,#12205,.T.);
#17671=ORIENTED_EDGE('',*,*,#12202,.T.);
#17672=ORIENTED_EDGE('',*,*,#12199,.T.);
#17673=ORIENTED_EDGE('',*,*,#12196,.T.);
#17674=ORIENTED_EDGE('',*,*,#12193,.T.);
#17675=ORIENTED_EDGE('',*,*,#12190,.T.);
#17676=ORIENTED_EDGE('',*,*,#12187,.T.);
#17677=ORIENTED_EDGE('',*,*,#12184,.T.);
#17678=ORIENTED_EDGE('',*,*,#12181,.T.);
#17679=ORIENTED_EDGE('',*,*,#12178,.T.);
#17680=ORIENTED_EDGE('',*,*,#12175,.T.);
#17681=ORIENTED_EDGE('',*,*,#12172,.T.);
#17682=ORIENTED_EDGE('',*,*,#12169,.T.);
#17683=ORIENTED_EDGE('',*,*,#12166,.T.);
#17684=ORIENTED_EDGE('',*,*,#12163,.T.);
#17685=ORIENTED_EDGE('',*,*,#12160,.T.);
#17686=ORIENTED_EDGE('',*,*,#12157,.T.);
#17687=ORIENTED_EDGE('',*,*,#12154,.T.);
#17688=ORIENTED_EDGE('',*,*,#12151,.T.);
#17689=ORIENTED_EDGE('',*,*,#12148,.T.);
#17690=ORIENTED_EDGE('',*,*,#12145,.T.);
#17691=ORIENTED_EDGE('',*,*,#12142,.T.);
#17692=ORIENTED_EDGE('',*,*,#12139,.T.);
#17693=ORIENTED_EDGE('',*,*,#12136,.T.);
#17694=ORIENTED_EDGE('',*,*,#12133,.T.);
#17695=ORIENTED_EDGE('',*,*,#12130,.T.);
#17696=ORIENTED_EDGE('',*,*,#12127,.T.);
#17697=ORIENTED_EDGE('',*,*,#12124,.T.);
#17698=ORIENTED_EDGE('',*,*,#12121,.T.);
#17699=ORIENTED_EDGE('',*,*,#12118,.T.);
#17700=ORIENTED_EDGE('',*,*,#12115,.T.);
#17701=ORIENTED_EDGE('',*,*,#12112,.T.);
#17702=ORIENTED_EDGE('',*,*,#12109,.T.);
#17703=ORIENTED_EDGE('',*,*,#12106,.T.);
#17704=ORIENTED_EDGE('',*,*,#12103,.T.);
#17705=ORIENTED_EDGE('',*,*,#12100,.T.);
#17706=ORIENTED_EDGE('',*,*,#12097,.T.);
#17707=ORIENTED_EDGE('',*,*,#12094,.T.);
#17708=ORIENTED_EDGE('',*,*,#12091,.T.);
#17709=ORIENTED_EDGE('',*,*,#12088,.T.);
#17710=ORIENTED_EDGE('',*,*,#12085,.T.);
#17711=ORIENTED_EDGE('',*,*,#12082,.T.);
#17712=ORIENTED_EDGE('',*,*,#12079,.T.);
#17713=ORIENTED_EDGE('',*,*,#12076,.T.);
#17714=ORIENTED_EDGE('',*,*,#12073,.T.);
#17715=ORIENTED_EDGE('',*,*,#12070,.T.);
#17716=ORIENTED_EDGE('',*,*,#12067,.T.);
#17717=ORIENTED_EDGE('',*,*,#12064,.T.);
#17718=ORIENTED_EDGE('',*,*,#12061,.T.);
#17719=ORIENTED_EDGE('',*,*,#12058,.T.);
#17720=ORIENTED_EDGE('',*,*,#12055,.T.);
#17721=ORIENTED_EDGE('',*,*,#12052,.T.);
#17722=ORIENTED_EDGE('',*,*,#12049,.T.);
#17723=ORIENTED_EDGE('',*,*,#12046,.T.);
#17724=ORIENTED_EDGE('',*,*,#12043,.T.);
#17725=ORIENTED_EDGE('',*,*,#12040,.T.);
#17726=ORIENTED_EDGE('',*,*,#12037,.T.);
#17727=ORIENTED_EDGE('',*,*,#12034,.T.);
#17728=ORIENTED_EDGE('',*,*,#12031,.T.);
#17729=ORIENTED_EDGE('',*,*,#12028,.T.);
#17730=ORIENTED_EDGE('',*,*,#12025,.T.);
#17731=ORIENTED_EDGE('',*,*,#12022,.T.);
#17732=ORIENTED_EDGE('',*,*,#12019,.T.);
#17733=ORIENTED_EDGE('',*,*,#12016,.T.);
#17734=ORIENTED_EDGE('',*,*,#12013,.T.);
#17735=ORIENTED_EDGE('',*,*,#12010,.T.);
#17736=ORIENTED_EDGE('',*,*,#12007,.T.);
#17737=ORIENTED_EDGE('',*,*,#12004,.T.);
#17738=ORIENTED_EDGE('',*,*,#12001,.T.);
#17739=ORIENTED_EDGE('',*,*,#11998,.T.);
#17740=ORIENTED_EDGE('',*,*,#11995,.T.);
#17741=ORIENTED_EDGE('',*,*,#11992,.T.);
#17742=ORIENTED_EDGE('',*,*,#11989,.T.);
#17743=ORIENTED_EDGE('',*,*,#11986,.T.);
#17744=ORIENTED_EDGE('',*,*,#11983,.T.);
#17745=ORIENTED_EDGE('',*,*,#12291,.T.);
#17746=ORIENTED_EDGE('',*,*,#12308,.F.);
#17747=ORIENTED_EDGE('',*,*,#11913,.F.);
#17748=ORIENTED_EDGE('',*,*,#11909,.F.);
#17749=ORIENTED_EDGE('',*,*,#11906,.F.);
#17750=ORIENTED_EDGE('',*,*,#11903,.F.);
#17751=ORIENTED_EDGE('',*,*,#11900,.F.);
#17752=ORIENTED_EDGE('',*,*,#11897,.F.);
#17753=ORIENTED_EDGE('',*,*,#11894,.F.);
#17754=ORIENTED_EDGE('',*,*,#11891,.F.);
#17755=ORIENTED_EDGE('',*,*,#11888,.F.);
#17756=ORIENTED_EDGE('',*,*,#11885,.F.);
#17757=ORIENTED_EDGE('',*,*,#11882,.F.);
#17758=ORIENTED_EDGE('',*,*,#11879,.F.);
#17759=ORIENTED_EDGE('',*,*,#11876,.F.);
#17760=ORIENTED_EDGE('',*,*,#11873,.F.);
#17761=ORIENTED_EDGE('',*,*,#11870,.F.);
#17762=ORIENTED_EDGE('',*,*,#11867,.F.);
#17763=ORIENTED_EDGE('',*,*,#11864,.F.);
#17764=ORIENTED_EDGE('',*,*,#11861,.F.);
#17765=ORIENTED_EDGE('',*,*,#11858,.F.);
#17766=ORIENTED_EDGE('',*,*,#11855,.F.);
#17767=ORIENTED_EDGE('',*,*,#11852,.F.);
#17768=ORIENTED_EDGE('',*,*,#11849,.F.);
#17769=ORIENTED_EDGE('',*,*,#11846,.F.);
#17770=ORIENTED_EDGE('',*,*,#11843,.F.);
#17771=ORIENTED_EDGE('',*,*,#11840,.F.);
#17772=ORIENTED_EDGE('',*,*,#11837,.F.);
#17773=ORIENTED_EDGE('',*,*,#11834,.F.);
#17774=ORIENTED_EDGE('',*,*,#11831,.F.);
#17775=ORIENTED_EDGE('',*,*,#11828,.F.);
#17776=ORIENTED_EDGE('',*,*,#11825,.F.);
#17777=ORIENTED_EDGE('',*,*,#11822,.F.);
#17778=ORIENTED_EDGE('',*,*,#11819,.F.);
#17779=ORIENTED_EDGE('',*,*,#11816,.F.);
#17780=ORIENTED_EDGE('',*,*,#11813,.F.);
#17781=ORIENTED_EDGE('',*,*,#11810,.F.);
#17782=ORIENTED_EDGE('',*,*,#11807,.F.);
#17783=ORIENTED_EDGE('',*,*,#11804,.F.);
#17784=ORIENTED_EDGE('',*,*,#11801,.F.);
#17785=ORIENTED_EDGE('',*,*,#11798,.F.);
#17786=ORIENTED_EDGE('',*,*,#11795,.F.);
#17787=ORIENTED_EDGE('',*,*,#11792,.F.);
#17788=ORIENTED_EDGE('',*,*,#11789,.F.);
#17789=ORIENTED_EDGE('',*,*,#11786,.F.);
#17790=ORIENTED_EDGE('',*,*,#11783,.F.);
#17791=ORIENTED_EDGE('',*,*,#11780,.F.);
#17792=ORIENTED_EDGE('',*,*,#11777,.F.);
#17793=ORIENTED_EDGE('',*,*,#11774,.F.);
#17794=ORIENTED_EDGE('',*,*,#11771,.F.);
#17795=ORIENTED_EDGE('',*,*,#11768,.F.);
#17796=ORIENTED_EDGE('',*,*,#11765,.F.);
#17797=ORIENTED_EDGE('',*,*,#11762,.F.);
#17798=ORIENTED_EDGE('',*,*,#11759,.F.);
#17799=ORIENTED_EDGE('',*,*,#11756,.F.);
#17800=ORIENTED_EDGE('',*,*,#11753,.F.);
#17801=ORIENTED_EDGE('',*,*,#11750,.F.);
#17802=ORIENTED_EDGE('',*,*,#11747,.F.);
#17803=ORIENTED_EDGE('',*,*,#11744,.F.);
#17804=ORIENTED_EDGE('',*,*,#11741,.F.);
#17805=ORIENTED_EDGE('',*,*,#11738,.F.);
#17806=ORIENTED_EDGE('',*,*,#11735,.F.);
#17807=ORIENTED_EDGE('',*,*,#11732,.F.);
#17808=ORIENTED_EDGE('',*,*,#11729,.F.);
#17809=ORIENTED_EDGE('',*,*,#11726,.F.);
#17810=ORIENTED_EDGE('',*,*,#11723,.F.);
#17811=ORIENTED_EDGE('',*,*,#11720,.F.);
#17812=ORIENTED_EDGE('',*,*,#11717,.F.);
#17813=ORIENTED_EDGE('',*,*,#11714,.F.);
#17814=ORIENTED_EDGE('',*,*,#11711,.F.);
#17815=ORIENTED_EDGE('',*,*,#11708,.F.);
#17816=ORIENTED_EDGE('',*,*,#11705,.F.);
#17817=ORIENTED_EDGE('',*,*,#11702,.F.);
#17818=ORIENTED_EDGE('',*,*,#11699,.F.);
#17819=ORIENTED_EDGE('',*,*,#11696,.F.);
#17820=ORIENTED_EDGE('',*,*,#11693,.F.);
#17821=ORIENTED_EDGE('',*,*,#11690,.F.);
#17822=ORIENTED_EDGE('',*,*,#11687,.F.);
#17823=ORIENTED_EDGE('',*,*,#11684,.F.);
#17824=ORIENTED_EDGE('',*,*,#11681,.F.);
#17825=ORIENTED_EDGE('',*,*,#11678,.F.);
#17826=ORIENTED_EDGE('',*,*,#11675,.F.);
#17827=ORIENTED_EDGE('',*,*,#11672,.F.);
#17828=ORIENTED_EDGE('',*,*,#11669,.F.);
#17829=ORIENTED_EDGE('',*,*,#11666,.F.);
#17830=ORIENTED_EDGE('',*,*,#11663,.F.);
#17831=ORIENTED_EDGE('',*,*,#11660,.F.);
#17832=ORIENTED_EDGE('',*,*,#11657,.F.);
#17833=ORIENTED_EDGE('',*,*,#11654,.F.);
#17834=ORIENTED_EDGE('',*,*,#11651,.F.);
#17835=ORIENTED_EDGE('',*,*,#11648,.F.);
#17836=ORIENTED_EDGE('',*,*,#11645,.F.);
#17837=ORIENTED_EDGE('',*,*,#11642,.F.);
#17838=ORIENTED_EDGE('',*,*,#11639,.F.);
#17839=ORIENTED_EDGE('',*,*,#11636,.F.);
#17840=ORIENTED_EDGE('',*,*,#11633,.F.);
#17841=ORIENTED_EDGE('',*,*,#11630,.F.);
#17842=ORIENTED_EDGE('',*,*,#11627,.F.);
#17843=ORIENTED_EDGE('',*,*,#11624,.F.);
#17844=ORIENTED_EDGE('',*,*,#11621,.F.);
#17845=ORIENTED_EDGE('',*,*,#11618,.F.);
#17846=ORIENTED_EDGE('',*,*,#11615,.F.);
#17847=ORIENTED_EDGE('',*,*,#11612,.F.);
#17848=ORIENTED_EDGE('',*,*,#11910,.T.);
#17849=ORIENTED_EDGE('',*,*,#12308,.T.);
#17850=ORIENTED_EDGE('',*,*,#12293,.T.);
#17851=ORIENTED_EDGE('',*,*,#12309,.F.);
#17852=ORIENTED_EDGE('',*,*,#12310,.F.);
#17853=ORIENTED_EDGE('',*,*,#12311,.F.);
#17854=ORIENTED_EDGE('',*,*,#12312,.F.);
#17855=ORIENTED_EDGE('',*,*,#12313,.F.);
#17856=ORIENTED_EDGE('',*,*,#12314,.T.);
#17857=ORIENTED_EDGE('',*,*,#12315,.T.);
#17858=ORIENTED_EDGE('',*,*,#12316,.F.);
#17859=ORIENTED_EDGE('',*,*,#12317,.T.);
#17860=ORIENTED_EDGE('',*,*,#12318,.F.);
#17861=ORIENTED_EDGE('',*,*,#12317,.F.);
#17862=ORIENTED_EDGE('',*,*,#12319,.F.);
#17863=ORIENTED_EDGE('',*,*,#12320,.T.);
#17864=ORIENTED_EDGE('',*,*,#12321,.F.);
#17865=ORIENTED_EDGE('',*,*,#12320,.F.);
#17866=ORIENTED_EDGE('',*,*,#12322,.F.);
#17867=ORIENTED_EDGE('',*,*,#12323,.T.);
#17868=ORIENTED_EDGE('',*,*,#12324,.F.);
#17869=ORIENTED_EDGE('',*,*,#12323,.F.);
#17870=ORIENTED_EDGE('',*,*,#12325,.F.);
#17871=ORIENTED_EDGE('',*,*,#12326,.T.);
#17872=ORIENTED_EDGE('',*,*,#12327,.F.);
#17873=ORIENTED_EDGE('',*,*,#12326,.F.);
#17874=ORIENTED_EDGE('',*,*,#12328,.F.);
#17875=ORIENTED_EDGE('',*,*,#12329,.T.);
#17876=ORIENTED_EDGE('',*,*,#12330,.F.);
#17877=ORIENTED_EDGE('',*,*,#12329,.F.);
#17878=ORIENTED_EDGE('',*,*,#12331,.F.);
#17879=ORIENTED_EDGE('',*,*,#12332,.T.);
#17880=ORIENTED_EDGE('',*,*,#12333,.F.);
#17881=ORIENTED_EDGE('',*,*,#12332,.F.);
#17882=ORIENTED_EDGE('',*,*,#12334,.F.);
#17883=ORIENTED_EDGE('',*,*,#12335,.T.);
#17884=ORIENTED_EDGE('',*,*,#12336,.F.);
#17885=ORIENTED_EDGE('',*,*,#12335,.F.);
#17886=ORIENTED_EDGE('',*,*,#12337,.F.);
#17887=ORIENTED_EDGE('',*,*,#12338,.T.);
#17888=ORIENTED_EDGE('',*,*,#12339,.F.);
#17889=ORIENTED_EDGE('',*,*,#12338,.F.);
#17890=ORIENTED_EDGE('',*,*,#12340,.F.);
#17891=ORIENTED_EDGE('',*,*,#12341,.T.);
#17892=ORIENTED_EDGE('',*,*,#12342,.F.);
#17893=ORIENTED_EDGE('',*,*,#12341,.F.);
#17894=ORIENTED_EDGE('',*,*,#12343,.F.);
#17895=ORIENTED_EDGE('',*,*,#12344,.T.);
#17896=ORIENTED_EDGE('',*,*,#12345,.F.);
#17897=ORIENTED_EDGE('',*,*,#12344,.F.);
#17898=ORIENTED_EDGE('',*,*,#12346,.F.);
#17899=ORIENTED_EDGE('',*,*,#12347,.T.);
#17900=ORIENTED_EDGE('',*,*,#12348,.F.);
#17901=ORIENTED_EDGE('',*,*,#12347,.F.);
#17902=ORIENTED_EDGE('',*,*,#12349,.F.);
#17903=ORIENTED_EDGE('',*,*,#12350,.T.);
#17904=ORIENTED_EDGE('',*,*,#12351,.F.);
#17905=ORIENTED_EDGE('',*,*,#12350,.F.);
#17906=ORIENTED_EDGE('',*,*,#12352,.F.);
#17907=ORIENTED_EDGE('',*,*,#12353,.T.);
#17908=ORIENTED_EDGE('',*,*,#12354,.F.);
#17909=ORIENTED_EDGE('',*,*,#12353,.F.);
#17910=ORIENTED_EDGE('',*,*,#12355,.F.);
#17911=ORIENTED_EDGE('',*,*,#12356,.T.);
#17912=ORIENTED_EDGE('',*,*,#12357,.F.);
#17913=ORIENTED_EDGE('',*,*,#12356,.F.);
#17914=ORIENTED_EDGE('',*,*,#12358,.F.);
#17915=ORIENTED_EDGE('',*,*,#12359,.T.);
#17916=ORIENTED_EDGE('',*,*,#12360,.F.);
#17917=ORIENTED_EDGE('',*,*,#12359,.F.);
#17918=ORIENTED_EDGE('',*,*,#12361,.F.);
#17919=ORIENTED_EDGE('',*,*,#12362,.T.);
#17920=ORIENTED_EDGE('',*,*,#12363,.F.);
#17921=ORIENTED_EDGE('',*,*,#12362,.F.);
#17922=ORIENTED_EDGE('',*,*,#12364,.F.);
#17923=ORIENTED_EDGE('',*,*,#12365,.T.);
#17924=ORIENTED_EDGE('',*,*,#12315,.F.);
#17925=ORIENTED_EDGE('',*,*,#12365,.F.);
#17926=ORIENTED_EDGE('',*,*,#12366,.T.);
#17927=ORIENTED_EDGE('',*,*,#12367,.T.);
#17928=ORIENTED_EDGE('',*,*,#12309,.T.);
#17929=ORIENTED_EDGE('',*,*,#12368,.T.);
#17930=ORIENTED_EDGE('',*,*,#12367,.F.);
#17931=ORIENTED_EDGE('',*,*,#12369,.T.);
#17932=ORIENTED_EDGE('',*,*,#12370,.F.);
#17933=ORIENTED_EDGE('',*,*,#12310,.T.);
#17934=ORIENTED_EDGE('',*,*,#12311,.T.);
#17935=ORIENTED_EDGE('',*,*,#12370,.T.);
#17936=ORIENTED_EDGE('',*,*,#12371,.T.);
#17937=ORIENTED_EDGE('',*,*,#12372,.T.);
#17938=ORIENTED_EDGE('',*,*,#12372,.F.);
#17939=ORIENTED_EDGE('',*,*,#12373,.F.);
#17940=ORIENTED_EDGE('',*,*,#12374,.F.);
#17941=ORIENTED_EDGE('',*,*,#12312,.T.);
#17942=ORIENTED_EDGE('',*,*,#12366,.F.);
#17943=ORIENTED_EDGE('',*,*,#12375,.F.);
#17944=ORIENTED_EDGE('',*,*,#12376,.F.);
#17945=ORIENTED_EDGE('',*,*,#12373,.T.);
#17946=ORIENTED_EDGE('',*,*,#12371,.F.);
#17947=ORIENTED_EDGE('',*,*,#12369,.F.);
#17948=ORIENTED_EDGE('',*,*,#12364,.T.);
#17949=ORIENTED_EDGE('',*,*,#12368,.F.);
#17950=ORIENTED_EDGE('',*,*,#12314,.F.);
#17951=ORIENTED_EDGE('',*,*,#12377,.F.);
#17952=ORIENTED_EDGE('',*,*,#12375,.T.);
#17953=ORIENTED_EDGE('',*,*,#12378,.F.);
#17954=ORIENTED_EDGE('',*,*,#12379,.T.);
#17955=ORIENTED_EDGE('',*,*,#12380,.F.);
#17956=ORIENTED_EDGE('',*,*,#12381,.F.);
#17957=ORIENTED_EDGE('',*,*,#12382,.F.);
#17958=ORIENTED_EDGE('',*,*,#12383,.T.);
#17959=ORIENTED_EDGE('',*,*,#12384,.F.);
#17960=ORIENTED_EDGE('',*,*,#12379,.F.);
#17961=ORIENTED_EDGE('',*,*,#12313,.T.);
#17962=ORIENTED_EDGE('',*,*,#12374,.T.);
#17963=ORIENTED_EDGE('',*,*,#12376,.T.);
#17964=ORIENTED_EDGE('',*,*,#12377,.T.);
#17965=ORIENTED_EDGE('',*,*,#12385,.F.);
#17966=ORIENTED_EDGE('',*,*,#12386,.F.);
#17967=ORIENTED_EDGE('',*,*,#12387,.F.);
#17968=ORIENTED_EDGE('',*,*,#12383,.F.);
#17969=ORIENTED_EDGE('',*,*,#12381,.T.);
#17970=ORIENTED_EDGE('',*,*,#12388,.F.);
#17971=ORIENTED_EDGE('',*,*,#12389,.F.);
#17972=ORIENTED_EDGE('',*,*,#12390,.F.);
#17973=ORIENTED_EDGE('',*,*,#12363,.T.);
#17974=ORIENTED_EDGE('',*,*,#12360,.T.);
#17975=ORIENTED_EDGE('',*,*,#12345,.T.);
#17976=ORIENTED_EDGE('',*,*,#12342,.T.);
#17977=ORIENTED_EDGE('',*,*,#12339,.T.);
#17978=ORIENTED_EDGE('',*,*,#12336,.T.);
#17979=ORIENTED_EDGE('',*,*,#12321,.T.);
#17980=ORIENTED_EDGE('',*,*,#12318,.T.);
#17981=ORIENTED_EDGE('',*,*,#12386,.T.);
#17982=ORIENTED_EDGE('',*,*,#12391,.F.);
#17983=ORIENTED_EDGE('',*,*,#12392,.F.);
#17984=ORIENTED_EDGE('',*,*,#12393,.F.);
#17985=ORIENTED_EDGE('',*,*,#12357,.T.);
#17986=ORIENTED_EDGE('',*,*,#12354,.T.);
#17987=ORIENTED_EDGE('',*,*,#12351,.T.);
#17988=ORIENTED_EDGE('',*,*,#12348,.T.);
#17989=ORIENTED_EDGE('',*,*,#12333,.T.);
#17990=ORIENTED_EDGE('',*,*,#12330,.T.);
#17991=ORIENTED_EDGE('',*,*,#12327,.T.);
#17992=ORIENTED_EDGE('',*,*,#12324,.T.);
#17993=ORIENTED_EDGE('',*,*,#12385,.T.);
#17994=ORIENTED_EDGE('',*,*,#12382,.T.);
#17995=ORIENTED_EDGE('',*,*,#12378,.T.);
#17996=ORIENTED_EDGE('',*,*,#12390,.T.);
#17997=ORIENTED_EDGE('',*,*,#12394,.T.);
#17998=ORIENTED_EDGE('',*,*,#12395,.F.);
#17999=ORIENTED_EDGE('',*,*,#12396,.F.);
#18000=ORIENTED_EDGE('',*,*,#12391,.T.);
#18001=ORIENTED_EDGE('',*,*,#12387,.T.);
#18002=ORIENTED_EDGE('',*,*,#12393,.T.);
#18003=ORIENTED_EDGE('',*,*,#12397,.T.);
#18004=ORIENTED_EDGE('',*,*,#12398,.F.);
#18005=ORIENTED_EDGE('',*,*,#12399,.F.);
#18006=ORIENTED_EDGE('',*,*,#12388,.T.);
#18007=ORIENTED_EDGE('',*,*,#12380,.T.);
#18008=ORIENTED_EDGE('',*,*,#12384,.T.);
#18009=ORIENTED_EDGE('',*,*,#12389,.T.);
#18010=ORIENTED_EDGE('',*,*,#12399,.T.);
#18011=ORIENTED_EDGE('',*,*,#12400,.F.);
#18012=ORIENTED_EDGE('',*,*,#12394,.F.);
#18013=ORIENTED_EDGE('',*,*,#12392,.T.);
#18014=ORIENTED_EDGE('',*,*,#12396,.T.);
#18015=ORIENTED_EDGE('',*,*,#12401,.F.);
#18016=ORIENTED_EDGE('',*,*,#12397,.F.);
#18017=ORIENTED_EDGE('',*,*,#12401,.T.);
#18018=ORIENTED_EDGE('',*,*,#12395,.T.);
#18019=ORIENTED_EDGE('',*,*,#12400,.T.);
#18020=ORIENTED_EDGE('',*,*,#12398,.T.);
#18021=ORIENTED_EDGE('',*,*,#12361,.T.);
#18022=ORIENTED_EDGE('',*,*,#12358,.T.);
#18023=ORIENTED_EDGE('',*,*,#12355,.T.);
#18024=ORIENTED_EDGE('',*,*,#12352,.T.);
#18025=ORIENTED_EDGE('',*,*,#12349,.T.);
#18026=ORIENTED_EDGE('',*,*,#12346,.T.);
#18027=ORIENTED_EDGE('',*,*,#12343,.T.);
#18028=ORIENTED_EDGE('',*,*,#12340,.T.);
#18029=ORIENTED_EDGE('',*,*,#12337,.T.);
#18030=ORIENTED_EDGE('',*,*,#12334,.T.);
#18031=ORIENTED_EDGE('',*,*,#12331,.T.);
#18032=ORIENTED_EDGE('',*,*,#12328,.T.);
#18033=ORIENTED_EDGE('',*,*,#12325,.T.);
#18034=ORIENTED_EDGE('',*,*,#12322,.T.);
#18035=ORIENTED_EDGE('',*,*,#12319,.T.);
#18036=ORIENTED_EDGE('',*,*,#12316,.T.);
#18037=ORIENTED_EDGE('',*,*,#12402,.F.);
#18038=ORIENTED_EDGE('',*,*,#12403,.F.);
#18039=ORIENTED_EDGE('',*,*,#12404,.F.);
#18040=ORIENTED_EDGE('',*,*,#12405,.F.);
#18041=ORIENTED_EDGE('',*,*,#12404,.T.);
#18042=ORIENTED_EDGE('',*,*,#12406,.F.);
#18043=ORIENTED_EDGE('',*,*,#12407,.F.);
#18044=ORIENTED_EDGE('',*,*,#12408,.F.);
#18045=ORIENTED_EDGE('',*,*,#12407,.T.);
#18046=ORIENTED_EDGE('',*,*,#12409,.F.);
#18047=ORIENTED_EDGE('',*,*,#12410,.F.);
#18048=ORIENTED_EDGE('',*,*,#12411,.F.);
#18049=ORIENTED_EDGE('',*,*,#12410,.T.);
#18050=ORIENTED_EDGE('',*,*,#12412,.F.);
#18051=ORIENTED_EDGE('',*,*,#12413,.F.);
#18052=ORIENTED_EDGE('',*,*,#12414,.F.);
#18053=ORIENTED_EDGE('',*,*,#12413,.T.);
#18054=ORIENTED_EDGE('',*,*,#12415,.F.);
#18055=ORIENTED_EDGE('',*,*,#12416,.F.);
#18056=ORIENTED_EDGE('',*,*,#12417,.F.);
#18057=ORIENTED_EDGE('',*,*,#12416,.T.);
#18058=ORIENTED_EDGE('',*,*,#12418,.F.);
#18059=ORIENTED_EDGE('',*,*,#12419,.F.);
#18060=ORIENTED_EDGE('',*,*,#12420,.F.);
#18061=ORIENTED_EDGE('',*,*,#12419,.T.);
#18062=ORIENTED_EDGE('',*,*,#12421,.F.);
#18063=ORIENTED_EDGE('',*,*,#12422,.F.);
#18064=ORIENTED_EDGE('',*,*,#12423,.F.);
#18065=ORIENTED_EDGE('',*,*,#12422,.T.);
#18066=ORIENTED_EDGE('',*,*,#12424,.F.);
#18067=ORIENTED_EDGE('',*,*,#12425,.F.);
#18068=ORIENTED_EDGE('',*,*,#12426,.F.);
#18069=ORIENTED_EDGE('',*,*,#12425,.T.);
#18070=ORIENTED_EDGE('',*,*,#12427,.F.);
#18071=ORIENTED_EDGE('',*,*,#12428,.F.);
#18072=ORIENTED_EDGE('',*,*,#12429,.F.);
#18073=ORIENTED_EDGE('',*,*,#12428,.T.);
#18074=ORIENTED_EDGE('',*,*,#12430,.F.);
#18075=ORIENTED_EDGE('',*,*,#12431,.F.);
#18076=ORIENTED_EDGE('',*,*,#12432,.F.);
#18077=ORIENTED_EDGE('',*,*,#12431,.T.);
#18078=ORIENTED_EDGE('',*,*,#12433,.F.);
#18079=ORIENTED_EDGE('',*,*,#12434,.F.);
#18080=ORIENTED_EDGE('',*,*,#12435,.F.);
#18081=ORIENTED_EDGE('',*,*,#12434,.T.);
#18082=ORIENTED_EDGE('',*,*,#12436,.F.);
#18083=ORIENTED_EDGE('',*,*,#12437,.F.);
#18084=ORIENTED_EDGE('',*,*,#12438,.F.);
#18085=ORIENTED_EDGE('',*,*,#12437,.T.);
#18086=ORIENTED_EDGE('',*,*,#12439,.F.);
#18087=ORIENTED_EDGE('',*,*,#12440,.F.);
#18088=ORIENTED_EDGE('',*,*,#12441,.F.);
#18089=ORIENTED_EDGE('',*,*,#12440,.T.);
#18090=ORIENTED_EDGE('',*,*,#12442,.F.);
#18091=ORIENTED_EDGE('',*,*,#12443,.F.);
#18092=ORIENTED_EDGE('',*,*,#12444,.F.);
#18093=ORIENTED_EDGE('',*,*,#12443,.T.);
#18094=ORIENTED_EDGE('',*,*,#12445,.F.);
#18095=ORIENTED_EDGE('',*,*,#12446,.F.);
#18096=ORIENTED_EDGE('',*,*,#12447,.F.);
#18097=ORIENTED_EDGE('',*,*,#12446,.T.);
#18098=ORIENTED_EDGE('',*,*,#12448,.F.);
#18099=ORIENTED_EDGE('',*,*,#12449,.F.);
#18100=ORIENTED_EDGE('',*,*,#12450,.F.);
#18101=ORIENTED_EDGE('',*,*,#12451,.T.);
#18102=ORIENTED_EDGE('',*,*,#12405,.T.);
#18103=ORIENTED_EDGE('',*,*,#12408,.T.);
#18104=ORIENTED_EDGE('',*,*,#12411,.T.);
#18105=ORIENTED_EDGE('',*,*,#12414,.T.);
#18106=ORIENTED_EDGE('',*,*,#12417,.T.);
#18107=ORIENTED_EDGE('',*,*,#12420,.T.);
#18108=ORIENTED_EDGE('',*,*,#12423,.T.);
#18109=ORIENTED_EDGE('',*,*,#12426,.T.);
#18110=ORIENTED_EDGE('',*,*,#12429,.T.);
#18111=ORIENTED_EDGE('',*,*,#12432,.T.);
#18112=ORIENTED_EDGE('',*,*,#12435,.T.);
#18113=ORIENTED_EDGE('',*,*,#12438,.T.);
#18114=ORIENTED_EDGE('',*,*,#12441,.T.);
#18115=ORIENTED_EDGE('',*,*,#12444,.T.);
#18116=ORIENTED_EDGE('',*,*,#12447,.T.);
#18117=ORIENTED_EDGE('',*,*,#12450,.T.);
#18118=ORIENTED_EDGE('',*,*,#12452,.F.);
#18119=ORIENTED_EDGE('',*,*,#12453,.F.);
#18120=ORIENTED_EDGE('',*,*,#12454,.F.);
#18121=ORIENTED_EDGE('',*,*,#12455,.F.);
#18122=ORIENTED_EDGE('',*,*,#12456,.F.);
#18123=ORIENTED_EDGE('',*,*,#12457,.F.);
#18124=ORIENTED_EDGE('',*,*,#12458,.F.);
#18125=ORIENTED_EDGE('',*,*,#12459,.F.);
#18126=ORIENTED_EDGE('',*,*,#12460,.F.);
#18127=ORIENTED_EDGE('',*,*,#12461,.F.);
#18128=ORIENTED_EDGE('',*,*,#12462,.F.);
#18129=ORIENTED_EDGE('',*,*,#12463,.F.);
#18130=ORIENTED_EDGE('',*,*,#12464,.F.);
#18131=ORIENTED_EDGE('',*,*,#12465,.F.);
#18132=ORIENTED_EDGE('',*,*,#12466,.F.);
#18133=ORIENTED_EDGE('',*,*,#12467,.F.);
#18134=ORIENTED_EDGE('',*,*,#12468,.F.);
#18135=ORIENTED_EDGE('',*,*,#12469,.T.);
#18136=ORIENTED_EDGE('',*,*,#12468,.T.);
#18137=ORIENTED_EDGE('',*,*,#12470,.T.);
#18138=ORIENTED_EDGE('',*,*,#12471,.T.);
#18139=ORIENTED_EDGE('',*,*,#12470,.F.);
#18140=ORIENTED_EDGE('',*,*,#12467,.T.);
#18141=ORIENTED_EDGE('',*,*,#12472,.T.);
#18142=ORIENTED_EDGE('',*,*,#12473,.T.);
#18143=ORIENTED_EDGE('',*,*,#12472,.F.);
#18144=ORIENTED_EDGE('',*,*,#12466,.T.);
#18145=ORIENTED_EDGE('',*,*,#12474,.T.);
#18146=ORIENTED_EDGE('',*,*,#12475,.T.);
#18147=ORIENTED_EDGE('',*,*,#12474,.F.);
#18148=ORIENTED_EDGE('',*,*,#12465,.T.);
#18149=ORIENTED_EDGE('',*,*,#12476,.T.);
#18150=ORIENTED_EDGE('',*,*,#12477,.T.);
#18151=ORIENTED_EDGE('',*,*,#12476,.F.);
#18152=ORIENTED_EDGE('',*,*,#12464,.T.);
#18153=ORIENTED_EDGE('',*,*,#12478,.T.);
#18154=ORIENTED_EDGE('',*,*,#12479,.T.);
#18155=ORIENTED_EDGE('',*,*,#12478,.F.);
#18156=ORIENTED_EDGE('',*,*,#12463,.T.);
#18157=ORIENTED_EDGE('',*,*,#12480,.T.);
#18158=ORIENTED_EDGE('',*,*,#12481,.T.);
#18159=ORIENTED_EDGE('',*,*,#12480,.F.);
#18160=ORIENTED_EDGE('',*,*,#12462,.T.);
#18161=ORIENTED_EDGE('',*,*,#12482,.T.);
#18162=ORIENTED_EDGE('',*,*,#12483,.T.);
#18163=ORIENTED_EDGE('',*,*,#12482,.F.);
#18164=ORIENTED_EDGE('',*,*,#12461,.T.);
#18165=ORIENTED_EDGE('',*,*,#12484,.T.);
#18166=ORIENTED_EDGE('',*,*,#12485,.T.);
#18167=ORIENTED_EDGE('',*,*,#12484,.F.);
#18168=ORIENTED_EDGE('',*,*,#12460,.T.);
#18169=ORIENTED_EDGE('',*,*,#12486,.T.);
#18170=ORIENTED_EDGE('',*,*,#12487,.T.);
#18171=ORIENTED_EDGE('',*,*,#12486,.F.);
#18172=ORIENTED_EDGE('',*,*,#12459,.T.);
#18173=ORIENTED_EDGE('',*,*,#12488,.T.);
#18174=ORIENTED_EDGE('',*,*,#12489,.T.);
#18175=ORIENTED_EDGE('',*,*,#12488,.F.);
#18176=ORIENTED_EDGE('',*,*,#12458,.T.);
#18177=ORIENTED_EDGE('',*,*,#12490,.T.);
#18178=ORIENTED_EDGE('',*,*,#12491,.T.);
#18179=ORIENTED_EDGE('',*,*,#12490,.F.);
#18180=ORIENTED_EDGE('',*,*,#12457,.T.);
#18181=ORIENTED_EDGE('',*,*,#12492,.T.);
#18182=ORIENTED_EDGE('',*,*,#12493,.T.);
#18183=ORIENTED_EDGE('',*,*,#12492,.F.);
#18184=ORIENTED_EDGE('',*,*,#12456,.T.);
#18185=ORIENTED_EDGE('',*,*,#12494,.T.);
#18186=ORIENTED_EDGE('',*,*,#12495,.T.);
#18187=ORIENTED_EDGE('',*,*,#12494,.F.);
#18188=ORIENTED_EDGE('',*,*,#12455,.T.);
#18189=ORIENTED_EDGE('',*,*,#12496,.T.);
#18190=ORIENTED_EDGE('',*,*,#12497,.T.);
#18191=ORIENTED_EDGE('',*,*,#12496,.F.);
#18192=ORIENTED_EDGE('',*,*,#12454,.T.);
#18193=ORIENTED_EDGE('',*,*,#12498,.T.);
#18194=ORIENTED_EDGE('',*,*,#12499,.T.);
#18195=ORIENTED_EDGE('',*,*,#12498,.F.);
#18196=ORIENTED_EDGE('',*,*,#12453,.T.);
#18197=ORIENTED_EDGE('',*,*,#12500,.T.);
#18198=ORIENTED_EDGE('',*,*,#12501,.T.);
#18199=ORIENTED_EDGE('',*,*,#12500,.F.);
#18200=ORIENTED_EDGE('',*,*,#12452,.T.);
#18201=ORIENTED_EDGE('',*,*,#12449,.T.);
#18202=ORIENTED_EDGE('',*,*,#12502,.F.);
#18203=ORIENTED_EDGE('',*,*,#12503,.T.);
#18204=ORIENTED_EDGE('',*,*,#12402,.T.);
#18205=ORIENTED_EDGE('',*,*,#12451,.F.);
#18206=ORIENTED_EDGE('',*,*,#12469,.F.);
#18207=ORIENTED_EDGE('',*,*,#12503,.F.);
#18208=ORIENTED_EDGE('',*,*,#12471,.F.);
#18209=ORIENTED_EDGE('',*,*,#12473,.F.);
#18210=ORIENTED_EDGE('',*,*,#12475,.F.);
#18211=ORIENTED_EDGE('',*,*,#12477,.F.);
#18212=ORIENTED_EDGE('',*,*,#12479,.F.);
#18213=ORIENTED_EDGE('',*,*,#12481,.F.);
#18214=ORIENTED_EDGE('',*,*,#12483,.F.);
#18215=ORIENTED_EDGE('',*,*,#12485,.F.);
#18216=ORIENTED_EDGE('',*,*,#12487,.F.);
#18217=ORIENTED_EDGE('',*,*,#12489,.F.);
#18218=ORIENTED_EDGE('',*,*,#12491,.F.);
#18219=ORIENTED_EDGE('',*,*,#12493,.F.);
#18220=ORIENTED_EDGE('',*,*,#12495,.F.);
#18221=ORIENTED_EDGE('',*,*,#12497,.F.);
#18222=ORIENTED_EDGE('',*,*,#12499,.F.);
#18223=ORIENTED_EDGE('',*,*,#12501,.F.);
#18224=ORIENTED_EDGE('',*,*,#12502,.T.);
#18225=ORIENTED_EDGE('',*,*,#12448,.T.);
#18226=ORIENTED_EDGE('',*,*,#12445,.T.);
#18227=ORIENTED_EDGE('',*,*,#12442,.T.);
#18228=ORIENTED_EDGE('',*,*,#12439,.T.);
#18229=ORIENTED_EDGE('',*,*,#12436,.T.);
#18230=ORIENTED_EDGE('',*,*,#12433,.T.);
#18231=ORIENTED_EDGE('',*,*,#12430,.T.);
#18232=ORIENTED_EDGE('',*,*,#12427,.T.);
#18233=ORIENTED_EDGE('',*,*,#12424,.T.);
#18234=ORIENTED_EDGE('',*,*,#12421,.T.);
#18235=ORIENTED_EDGE('',*,*,#12418,.T.);
#18236=ORIENTED_EDGE('',*,*,#12415,.T.);
#18237=ORIENTED_EDGE('',*,*,#12412,.T.);
#18238=ORIENTED_EDGE('',*,*,#12409,.T.);
#18239=ORIENTED_EDGE('',*,*,#12406,.T.);
#18240=ORIENTED_EDGE('',*,*,#12403,.T.);
#18241=ORIENTED_EDGE('',*,*,#12504,.F.);
#18242=ORIENTED_EDGE('',*,*,#12505,.T.);
#18243=ORIENTED_EDGE('',*,*,#12506,.F.);
#18244=ORIENTED_EDGE('',*,*,#12505,.F.);
#18245=ORIENTED_EDGE('',*,*,#12507,.F.);
#18246=ORIENTED_EDGE('',*,*,#12508,.T.);
#18247=ORIENTED_EDGE('',*,*,#12509,.F.);
#18248=ORIENTED_EDGE('',*,*,#12510,.F.);
#18249=ORIENTED_EDGE('',*,*,#12511,.F.);
#18250=ORIENTED_EDGE('',*,*,#12510,.T.);
#18251=ORIENTED_EDGE('',*,*,#12512,.F.);
#18252=ORIENTED_EDGE('',*,*,#12513,.F.);
#18253=ORIENTED_EDGE('',*,*,#12514,.F.);
#18254=ORIENTED_EDGE('',*,*,#12513,.T.);
#18255=ORIENTED_EDGE('',*,*,#12515,.F.);
#18256=ORIENTED_EDGE('',*,*,#12516,.F.);
#18257=ORIENTED_EDGE('',*,*,#12517,.F.);
#18258=ORIENTED_EDGE('',*,*,#12516,.T.);
#18259=ORIENTED_EDGE('',*,*,#12518,.F.);
#18260=ORIENTED_EDGE('',*,*,#12508,.F.);
#18261=ORIENTED_EDGE('',*,*,#12518,.T.);
#18262=ORIENTED_EDGE('',*,*,#12515,.T.);
#18263=ORIENTED_EDGE('',*,*,#12512,.T.);
#18264=ORIENTED_EDGE('',*,*,#12509,.T.);
#18265=ORIENTED_EDGE('',*,*,#12506,.T.);
#18266=ORIENTED_EDGE('',*,*,#12517,.T.);
#18267=ORIENTED_EDGE('',*,*,#12507,.T.);
#18268=ORIENTED_EDGE('',*,*,#12511,.T.);
#18269=ORIENTED_EDGE('',*,*,#12514,.T.);
#18270=ORIENTED_EDGE('',*,*,#12504,.T.);
#18271=ORIENTED_EDGE('',*,*,#12519,.F.);
#18272=ORIENTED_EDGE('',*,*,#12520,.T.);
#18273=ORIENTED_EDGE('',*,*,#12521,.F.);
#18274=ORIENTED_EDGE('',*,*,#12520,.F.);
#18275=ORIENTED_EDGE('',*,*,#12522,.F.);
#18276=ORIENTED_EDGE('',*,*,#12523,.T.);
#18277=ORIENTED_EDGE('',*,*,#12524,.F.);
#18278=ORIENTED_EDGE('',*,*,#12525,.F.);
#18279=ORIENTED_EDGE('',*,*,#12526,.F.);
#18280=ORIENTED_EDGE('',*,*,#12525,.T.);
#18281=ORIENTED_EDGE('',*,*,#12527,.F.);
#18282=ORIENTED_EDGE('',*,*,#12528,.F.);
#18283=ORIENTED_EDGE('',*,*,#12529,.F.);
#18284=ORIENTED_EDGE('',*,*,#12528,.T.);
#18285=ORIENTED_EDGE('',*,*,#12530,.F.);
#18286=ORIENTED_EDGE('',*,*,#12531,.F.);
#18287=ORIENTED_EDGE('',*,*,#12532,.F.);
#18288=ORIENTED_EDGE('',*,*,#12531,.T.);
#18289=ORIENTED_EDGE('',*,*,#12533,.F.);
#18290=ORIENTED_EDGE('',*,*,#12523,.F.);
#18291=ORIENTED_EDGE('',*,*,#12533,.T.);
#18292=ORIENTED_EDGE('',*,*,#12530,.T.);
#18293=ORIENTED_EDGE('',*,*,#12527,.T.);
#18294=ORIENTED_EDGE('',*,*,#12524,.T.);
#18295=ORIENTED_EDGE('',*,*,#12519,.T.);
#18296=ORIENTED_EDGE('',*,*,#12532,.T.);
#18297=ORIENTED_EDGE('',*,*,#12522,.T.);
#18298=ORIENTED_EDGE('',*,*,#12526,.T.);
#18299=ORIENTED_EDGE('',*,*,#12529,.T.);
#18300=ORIENTED_EDGE('',*,*,#12521,.T.);
#18301=ORIENTED_EDGE('',*,*,#12534,.F.);
#18302=ORIENTED_EDGE('',*,*,#12535,.T.);
#18303=ORIENTED_EDGE('',*,*,#12536,.F.);
#18304=ORIENTED_EDGE('',*,*,#12535,.F.);
#18305=ORIENTED_EDGE('',*,*,#12537,.T.);
#18306=ORIENTED_EDGE('',*,*,#12538,.T.);
#18307=ORIENTED_EDGE('',*,*,#12539,.F.);
#18308=ORIENTED_EDGE('',*,*,#12540,.F.);
#18309=ORIENTED_EDGE('',*,*,#12541,.T.);
#18310=ORIENTED_EDGE('',*,*,#12540,.T.);
#18311=ORIENTED_EDGE('',*,*,#12542,.F.);
#18312=ORIENTED_EDGE('',*,*,#12543,.F.);
#18313=ORIENTED_EDGE('',*,*,#12544,.T.);
#18314=ORIENTED_EDGE('',*,*,#12543,.T.);
#18315=ORIENTED_EDGE('',*,*,#12545,.F.);
#18316=ORIENTED_EDGE('',*,*,#12546,.F.);
#18317=ORIENTED_EDGE('',*,*,#12547,.T.);
#18318=ORIENTED_EDGE('',*,*,#12546,.T.);
#18319=ORIENTED_EDGE('',*,*,#12548,.F.);
#18320=ORIENTED_EDGE('',*,*,#12538,.F.);
#18321=ORIENTED_EDGE('',*,*,#12547,.F.);
#18322=ORIENTED_EDGE('',*,*,#12537,.F.);
#18323=ORIENTED_EDGE('',*,*,#12541,.F.);
#18324=ORIENTED_EDGE('',*,*,#12544,.F.);
#18325=ORIENTED_EDGE('',*,*,#12536,.T.);
#18326=ORIENTED_EDGE('',*,*,#12548,.T.);
#18327=ORIENTED_EDGE('',*,*,#12545,.T.);
#18328=ORIENTED_EDGE('',*,*,#12542,.T.);
#18329=ORIENTED_EDGE('',*,*,#12539,.T.);
#18330=ORIENTED_EDGE('',*,*,#12534,.T.);
#18331=ORIENTED_EDGE('',*,*,#12549,.T.);
#18332=ORIENTED_EDGE('',*,*,#12550,.T.);
#18333=ORIENTED_EDGE('',*,*,#12551,.T.);
#18334=ORIENTED_EDGE('',*,*,#12552,.T.);
#18335=ORIENTED_EDGE('',*,*,#12551,.F.);
#18336=ORIENTED_EDGE('',*,*,#12553,.T.);
#18337=ORIENTED_EDGE('',*,*,#12554,.T.);
#18338=ORIENTED_EDGE('',*,*,#12555,.T.);
#18339=ORIENTED_EDGE('',*,*,#12554,.F.);
#18340=ORIENTED_EDGE('',*,*,#12556,.T.);
#18341=ORIENTED_EDGE('',*,*,#12557,.T.);
#18342=ORIENTED_EDGE('',*,*,#12558,.T.);
#18343=ORIENTED_EDGE('',*,*,#12557,.F.);
#18344=ORIENTED_EDGE('',*,*,#12559,.T.);
#18345=ORIENTED_EDGE('',*,*,#12560,.T.);
#18346=ORIENTED_EDGE('',*,*,#12561,.T.);
#18347=ORIENTED_EDGE('',*,*,#12560,.F.);
#18348=ORIENTED_EDGE('',*,*,#12562,.T.);
#18349=ORIENTED_EDGE('',*,*,#12563,.T.);
#18350=ORIENTED_EDGE('',*,*,#12564,.T.);
#18351=ORIENTED_EDGE('',*,*,#12563,.F.);
#18352=ORIENTED_EDGE('',*,*,#12565,.T.);
#18353=ORIENTED_EDGE('',*,*,#12566,.T.);
#18354=ORIENTED_EDGE('',*,*,#12567,.T.);
#18355=ORIENTED_EDGE('',*,*,#12566,.F.);
#18356=ORIENTED_EDGE('',*,*,#12568,.T.);
#18357=ORIENTED_EDGE('',*,*,#12569,.T.);
#18358=ORIENTED_EDGE('',*,*,#12570,.T.);
#18359=ORIENTED_EDGE('',*,*,#12569,.F.);
#18360=ORIENTED_EDGE('',*,*,#12571,.T.);
#18361=ORIENTED_EDGE('',*,*,#12572,.T.);
#18362=ORIENTED_EDGE('',*,*,#12573,.T.);
#18363=ORIENTED_EDGE('',*,*,#12572,.F.);
#18364=ORIENTED_EDGE('',*,*,#12574,.T.);
#18365=ORIENTED_EDGE('',*,*,#12575,.T.);
#18366=ORIENTED_EDGE('',*,*,#12576,.T.);
#18367=ORIENTED_EDGE('',*,*,#12575,.F.);
#18368=ORIENTED_EDGE('',*,*,#12577,.T.);
#18369=ORIENTED_EDGE('',*,*,#12578,.T.);
#18370=ORIENTED_EDGE('',*,*,#12579,.T.);
#18371=ORIENTED_EDGE('',*,*,#12578,.F.);
#18372=ORIENTED_EDGE('',*,*,#12580,.T.);
#18373=ORIENTED_EDGE('',*,*,#12581,.T.);
#18374=ORIENTED_EDGE('',*,*,#12582,.T.);
#18375=ORIENTED_EDGE('',*,*,#12581,.F.);
#18376=ORIENTED_EDGE('',*,*,#12583,.T.);
#18377=ORIENTED_EDGE('',*,*,#12584,.T.);
#18378=ORIENTED_EDGE('',*,*,#12585,.T.);
#18379=ORIENTED_EDGE('',*,*,#12584,.F.);
#18380=ORIENTED_EDGE('',*,*,#12586,.T.);
#18381=ORIENTED_EDGE('',*,*,#12587,.T.);
#18382=ORIENTED_EDGE('',*,*,#12588,.T.);
#18383=ORIENTED_EDGE('',*,*,#12587,.F.);
#18384=ORIENTED_EDGE('',*,*,#12589,.T.);
#18385=ORIENTED_EDGE('',*,*,#12590,.T.);
#18386=ORIENTED_EDGE('',*,*,#12591,.T.);
#18387=ORIENTED_EDGE('',*,*,#12590,.F.);
#18388=ORIENTED_EDGE('',*,*,#12592,.T.);
#18389=ORIENTED_EDGE('',*,*,#12593,.T.);
#18390=ORIENTED_EDGE('',*,*,#12594,.T.);
#18391=ORIENTED_EDGE('',*,*,#12593,.F.);
#18392=ORIENTED_EDGE('',*,*,#12595,.T.);
#18393=ORIENTED_EDGE('',*,*,#12596,.T.);
#18394=ORIENTED_EDGE('',*,*,#12597,.T.);
#18395=ORIENTED_EDGE('',*,*,#12598,.F.);
#18396=ORIENTED_EDGE('',*,*,#12599,.T.);
#18397=ORIENTED_EDGE('',*,*,#12600,.T.);
#18398=ORIENTED_EDGE('',*,*,#12601,.T.);
#18399=ORIENTED_EDGE('',*,*,#12602,.T.);
#18400=ORIENTED_EDGE('',*,*,#12603,.T.);
#18401=ORIENTED_EDGE('',*,*,#12604,.T.);
#18402=ORIENTED_EDGE('',*,*,#12605,.T.);
#18403=ORIENTED_EDGE('',*,*,#12606,.T.);
#18404=ORIENTED_EDGE('',*,*,#12607,.T.);
#18405=ORIENTED_EDGE('',*,*,#12608,.T.);
#18406=ORIENTED_EDGE('',*,*,#12609,.T.);
#18407=ORIENTED_EDGE('',*,*,#12610,.T.);
#18408=ORIENTED_EDGE('',*,*,#12611,.T.);
#18409=ORIENTED_EDGE('',*,*,#12612,.T.);
#18410=ORIENTED_EDGE('',*,*,#12613,.T.);
#18411=ORIENTED_EDGE('',*,*,#12614,.T.);
#18412=ORIENTED_EDGE('',*,*,#12615,.T.);
#18413=ORIENTED_EDGE('',*,*,#12595,.F.);
#18414=ORIENTED_EDGE('',*,*,#12592,.F.);
#18415=ORIENTED_EDGE('',*,*,#12589,.F.);
#18416=ORIENTED_EDGE('',*,*,#12586,.F.);
#18417=ORIENTED_EDGE('',*,*,#12583,.F.);
#18418=ORIENTED_EDGE('',*,*,#12580,.F.);
#18419=ORIENTED_EDGE('',*,*,#12577,.F.);
#18420=ORIENTED_EDGE('',*,*,#12574,.F.);
#18421=ORIENTED_EDGE('',*,*,#12571,.F.);
#18422=ORIENTED_EDGE('',*,*,#12568,.F.);
#18423=ORIENTED_EDGE('',*,*,#12565,.F.);
#18424=ORIENTED_EDGE('',*,*,#12562,.F.);
#18425=ORIENTED_EDGE('',*,*,#12559,.F.);
#18426=ORIENTED_EDGE('',*,*,#12556,.F.);
#18427=ORIENTED_EDGE('',*,*,#12553,.F.);
#18428=ORIENTED_EDGE('',*,*,#12550,.F.);
#18429=ORIENTED_EDGE('',*,*,#12616,.F.);
#18430=ORIENTED_EDGE('',*,*,#12617,.F.);
#18431=ORIENTED_EDGE('',*,*,#12618,.F.);
#18432=ORIENTED_EDGE('',*,*,#12599,.F.);
#18433=ORIENTED_EDGE('',*,*,#12618,.T.);
#18434=ORIENTED_EDGE('',*,*,#12619,.F.);
#18435=ORIENTED_EDGE('',*,*,#12620,.F.);
#18436=ORIENTED_EDGE('',*,*,#12600,.F.);
#18437=ORIENTED_EDGE('',*,*,#12620,.T.);
#18438=ORIENTED_EDGE('',*,*,#12621,.F.);
#18439=ORIENTED_EDGE('',*,*,#12622,.F.);
#18440=ORIENTED_EDGE('',*,*,#12601,.F.);
#18441=ORIENTED_EDGE('',*,*,#12622,.T.);
#18442=ORIENTED_EDGE('',*,*,#12623,.F.);
#18443=ORIENTED_EDGE('',*,*,#12624,.F.);
#18444=ORIENTED_EDGE('',*,*,#12602,.F.);
#18445=ORIENTED_EDGE('',*,*,#12624,.T.);
#18446=ORIENTED_EDGE('',*,*,#12625,.F.);
#18447=ORIENTED_EDGE('',*,*,#12626,.F.);
#18448=ORIENTED_EDGE('',*,*,#12603,.F.);
#18449=ORIENTED_EDGE('',*,*,#12626,.T.);
#18450=ORIENTED_EDGE('',*,*,#12627,.F.);
#18451=ORIENTED_EDGE('',*,*,#12628,.F.);
#18452=ORIENTED_EDGE('',*,*,#12604,.F.);
#18453=ORIENTED_EDGE('',*,*,#12628,.T.);
#18454=ORIENTED_EDGE('',*,*,#12629,.F.);
#18455=ORIENTED_EDGE('',*,*,#12630,.F.);
#18456=ORIENTED_EDGE('',*,*,#12605,.F.);
#18457=ORIENTED_EDGE('',*,*,#12630,.T.);
#18458=ORIENTED_EDGE('',*,*,#12631,.F.);
#18459=ORIENTED_EDGE('',*,*,#12632,.F.);
#18460=ORIENTED_EDGE('',*,*,#12606,.F.);
#18461=ORIENTED_EDGE('',*,*,#12632,.T.);
#18462=ORIENTED_EDGE('',*,*,#12633,.F.);
#18463=ORIENTED_EDGE('',*,*,#12634,.F.);
#18464=ORIENTED_EDGE('',*,*,#12607,.F.);
#18465=ORIENTED_EDGE('',*,*,#12634,.T.);
#18466=ORIENTED_EDGE('',*,*,#12635,.F.);
#18467=ORIENTED_EDGE('',*,*,#12636,.F.);
#18468=ORIENTED_EDGE('',*,*,#12608,.F.);
#18469=ORIENTED_EDGE('',*,*,#12636,.T.);
#18470=ORIENTED_EDGE('',*,*,#12637,.F.);
#18471=ORIENTED_EDGE('',*,*,#12638,.F.);
#18472=ORIENTED_EDGE('',*,*,#12609,.F.);
#18473=ORIENTED_EDGE('',*,*,#12638,.T.);
#18474=ORIENTED_EDGE('',*,*,#12639,.F.);
#18475=ORIENTED_EDGE('',*,*,#12640,.F.);
#18476=ORIENTED_EDGE('',*,*,#12610,.F.);
#18477=ORIENTED_EDGE('',*,*,#12640,.T.);
#18478=ORIENTED_EDGE('',*,*,#12641,.F.);
#18479=ORIENTED_EDGE('',*,*,#12642,.F.);
#18480=ORIENTED_EDGE('',*,*,#12611,.F.);
#18481=ORIENTED_EDGE('',*,*,#12642,.T.);
#18482=ORIENTED_EDGE('',*,*,#12643,.F.);
#18483=ORIENTED_EDGE('',*,*,#12644,.F.);
#18484=ORIENTED_EDGE('',*,*,#12612,.F.);
#18485=ORIENTED_EDGE('',*,*,#12644,.T.);
#18486=ORIENTED_EDGE('',*,*,#12645,.F.);
#18487=ORIENTED_EDGE('',*,*,#12646,.F.);
#18488=ORIENTED_EDGE('',*,*,#12613,.F.);
#18489=ORIENTED_EDGE('',*,*,#12646,.T.);
#18490=ORIENTED_EDGE('',*,*,#12647,.F.);
#18491=ORIENTED_EDGE('',*,*,#12648,.F.);
#18492=ORIENTED_EDGE('',*,*,#12614,.F.);
#18493=ORIENTED_EDGE('',*,*,#12648,.T.);
#18494=ORIENTED_EDGE('',*,*,#12649,.T.);
#18495=ORIENTED_EDGE('',*,*,#12596,.F.);
#18496=ORIENTED_EDGE('',*,*,#12615,.F.);
#18497=ORIENTED_EDGE('',*,*,#12650,.F.);
#18498=ORIENTED_EDGE('',*,*,#12616,.T.);
#18499=ORIENTED_EDGE('',*,*,#12598,.T.);
#18500=ORIENTED_EDGE('',*,*,#12549,.F.);
#18501=ORIENTED_EDGE('',*,*,#12650,.T.);
#18502=ORIENTED_EDGE('',*,*,#12552,.F.);
#18503=ORIENTED_EDGE('',*,*,#12555,.F.);
#18504=ORIENTED_EDGE('',*,*,#12558,.F.);
#18505=ORIENTED_EDGE('',*,*,#12561,.F.);
#18506=ORIENTED_EDGE('',*,*,#12564,.F.);
#18507=ORIENTED_EDGE('',*,*,#12567,.F.);
#18508=ORIENTED_EDGE('',*,*,#12570,.F.);
#18509=ORIENTED_EDGE('',*,*,#12573,.F.);
#18510=ORIENTED_EDGE('',*,*,#12576,.F.);
#18511=ORIENTED_EDGE('',*,*,#12579,.F.);
#18512=ORIENTED_EDGE('',*,*,#12582,.F.);
#18513=ORIENTED_EDGE('',*,*,#12585,.F.);
#18514=ORIENTED_EDGE('',*,*,#12588,.F.);
#18515=ORIENTED_EDGE('',*,*,#12591,.F.);
#18516=ORIENTED_EDGE('',*,*,#12594,.F.);
#18517=ORIENTED_EDGE('',*,*,#12597,.F.);
#18518=ORIENTED_EDGE('',*,*,#12649,.F.);
#18519=ORIENTED_EDGE('',*,*,#12647,.T.);
#18520=ORIENTED_EDGE('',*,*,#12645,.T.);
#18521=ORIENTED_EDGE('',*,*,#12643,.T.);
#18522=ORIENTED_EDGE('',*,*,#12641,.T.);
#18523=ORIENTED_EDGE('',*,*,#12639,.T.);
#18524=ORIENTED_EDGE('',*,*,#12637,.T.);
#18525=ORIENTED_EDGE('',*,*,#12635,.T.);
#18526=ORIENTED_EDGE('',*,*,#12633,.T.);
#18527=ORIENTED_EDGE('',*,*,#12631,.T.);
#18528=ORIENTED_EDGE('',*,*,#12629,.T.);
#18529=ORIENTED_EDGE('',*,*,#12627,.T.);
#18530=ORIENTED_EDGE('',*,*,#12625,.T.);
#18531=ORIENTED_EDGE('',*,*,#12623,.T.);
#18532=ORIENTED_EDGE('',*,*,#12621,.T.);
#18533=ORIENTED_EDGE('',*,*,#12619,.T.);
#18534=ORIENTED_EDGE('',*,*,#12617,.T.);
#18535=PLANE('',#20258);
#18536=PLANE('',#20275);
#18537=PLANE('',#20282);
#18538=PLANE('',#20289);
#18539=PLANE('',#20292);
#18540=PLANE('',#20295);
#18541=PLANE('',#20296);
#18542=PLANE('',#20297);
#18543=PLANE('',#20298);
#18544=PLANE('',#20299);
#18545=PLANE('',#20300);
#18546=PLANE('',#20301);
#18547=PLANE('',#20302);
#18548=PLANE('',#20305);
#18549=PLANE('',#20306);
#18550=PLANE('',#20307);
#18551=PLANE('',#20308);
#18552=PLANE('',#20309);
#18553=PLANE('',#20310);
#18554=PLANE('',#20317);
#18555=PLANE('',#20324);
#18556=PLANE('',#20327);
#18557=PLANE('',#20328);
#18558=PLANE('',#20338);
#18559=PLANE('',#20345);
#18560=PLANE('',#20359);
#18561=PLANE('',#20360);
#18562=PLANE('',#20361);
#18563=PLANE('',#20362);
#18564=PLANE('',#20367);
#18565=PLANE('',#20368);
#18566=PLANE('',#20381);
#18567=PLANE('',#20382);
#18568=PLANE('',#20383);
#18569=PLANE('',#20384);
#18570=PLANE('',#20396);
#18571=PLANE('',#20397);
#18572=PLANE('',#20398);
#18573=PLANE('',#20399);
#18574=PLANE('',#20401);
#18575=PLANE('',#20403);
#18576=PLANE('',#20405);
#18577=PLANE('',#20406);
#18578=PLANE('',#20407);
#18579=PLANE('',#20408);
#18580=PLANE('',#20410);
#18581=PLANE('',#20412);
#18582=PLANE('',#20416);
#18583=PLANE('',#20420);
#18584=PLANE('',#20421);
#18585=PLANE('',#20425);
#18586=PLANE('',#20429);
#18587=PLANE('',#20433);
#18588=PLANE('',#20434);
#18589=PLANE('',#20435);
#18590=PLANE('',#20436);
#18591=PLANE('',#20437);
#18592=PLANE('',#20438);
#18593=PLANE('',#20439);
#18594=PLANE('',#20440);
#18595=PLANE('',#20441);
#18596=PLANE('',#20442);
#18597=PLANE('',#20446);
#18598=PLANE('',#20459);
#18599=PLANE('',#20460);
#18600=PLANE('',#20463);
#18601=PLANE('',#20470);
#18602=PLANE('',#20477);
#18603=PLANE('',#20478);
#18604=PLANE('',#20479);
#18605=PLANE('',#20486);
#18606=PLANE('',#20491);
#18607=PLANE('',#20493);
#18608=PLANE('',#20510);
#18609=PLANE('',#20517);
#18610=PLANE('',#20524);
#18611=PLANE('',#20527);
#18612=PLANE('',#20530);
#18613=PLANE('',#20531);
#18614=PLANE('',#20532);
#18615=PLANE('',#20533);
#18616=PLANE('',#20534);
#18617=PLANE('',#20535);
#18618=PLANE('',#20536);
#18619=PLANE('',#20537);
#18620=PLANE('',#20540);
#18621=PLANE('',#20541);
#18622=PLANE('',#20542);
#18623=PLANE('',#20543);
#18624=PLANE('',#20544);
#18625=PLANE('',#20545);
#18626=PLANE('',#20552);
#18627=PLANE('',#20559);
#18628=PLANE('',#20562);
#18629=PLANE('',#20563);
#18630=PLANE('',#20573);
#18631=PLANE('',#20580);
#18632=PLANE('',#20594);
#18633=PLANE('',#20595);
#18634=PLANE('',#20596);
#18635=PLANE('',#20597);
#18636=PLANE('',#20602);
#18637=PLANE('',#20603);
#18638=PLANE('',#20616);
#18639=PLANE('',#20617);
#18640=PLANE('',#20618);
#18641=PLANE('',#20619);
#18642=PLANE('',#20631);
#18643=PLANE('',#20632);
#18644=PLANE('',#20633);
#18645=PLANE('',#20634);
#18646=PLANE('',#20636);
#18647=PLANE('',#20638);
#18648=PLANE('',#20640);
#18649=PLANE('',#20641);
#18650=PLANE('',#20642);
#18651=PLANE('',#20643);
#18652=PLANE('',#20645);
#18653=PLANE('',#20647);
#18654=PLANE('',#20651);
#18655=PLANE('',#20655);
#18656=PLANE('',#20656);
#18657=PLANE('',#20660);
#18658=PLANE('',#20664);
#18659=PLANE('',#20668);
#18660=PLANE('',#20669);
#18661=PLANE('',#20670);
#18662=PLANE('',#20671);
#18663=PLANE('',#20672);
#18664=PLANE('',#20673);
#18665=PLANE('',#20674);
#18666=PLANE('',#20675);
#18667=PLANE('',#20676);
#18668=PLANE('',#20677);
#18669=PLANE('',#20681);
#18670=PLANE('',#20694);
#18671=PLANE('',#20695);
#18672=PLANE('',#20698);
#18673=PLANE('',#20705);
#18674=PLANE('',#20712);
#18675=PLANE('',#20713);
#18676=PLANE('',#20714);
#18677=PLANE('',#20721);
#18678=PLANE('',#20726);
#18679=PLANE('',#20840);
#18680=PLANE('',#20841);
#18681=PLANE('',#20842);
#18682=PLANE('',#20843);
#18683=PLANE('',#20844);
#18684=PLANE('',#20845);
#18685=PLANE('',#20846);
#18686=PLANE('',#20847);
#18687=PLANE('',#20848);
#18688=PLANE('',#20849);
#18689=PLANE('',#20850);
#18690=PLANE('',#20851);
#18691=PLANE('',#20852);
#18692=PLANE('',#20853);
#18693=PLANE('',#20854);
#18694=PLANE('',#20855);
#18695=PLANE('',#20856);
#18696=PLANE('',#20857);
#18697=PLANE('',#20858);
#18698=PLANE('',#20859);
#18699=PLANE('',#20860);
#18700=PLANE('',#20861);
#18701=PLANE('',#20862);
#18702=PLANE('',#20863);
#18703=PLANE('',#20864);
#18704=PLANE('',#20865);
#18705=PLANE('',#20897);
#18706=PLANE('',#20898);
#18707=PLANE('',#20921);
#18708=PLANE('',#20922);
#18709=PLANE('',#21054);
#18710=PLANE('',#21055);
#18711=PLANE('',#21056);
#18712=PLANE('',#21057);
#18713=PLANE('',#21058);
#18714=PLANE('',#21059);
#18715=PLANE('',#21060);
#18716=PLANE('',#21061);
#18717=PLANE('',#21062);
#18718=PLANE('',#21063);
#18719=PLANE('',#21064);
#18720=PLANE('',#21065);
#18721=PLANE('',#21066);
#18722=PLANE('',#21067);
#18723=PLANE('',#21068);
#18724=PLANE('',#21069);
#18725=PLANE('',#21070);
#18726=PLANE('',#21071);
#18727=PLANE('',#21072);
#18728=PLANE('',#21073);
#18729=PLANE('',#21074);
#18730=PLANE('',#21075);
#18731=PLANE('',#21076);
#18732=PLANE('',#21077);
#18733=PLANE('',#21078);
#18734=PLANE('',#21079);
#18735=PLANE('',#21081);
#18736=PLANE('',#21082);
#18737=PLANE('',#21083);
#18738=PLANE('',#21084);
#18739=PLANE('',#21085);
#18740=PLANE('',#21086);
#18741=PLANE('',#21087);
#18742=PLANE('',#21088);
#18743=PLANE('',#21089);
#18744=PLANE('',#21090);
#18745=PLANE('',#21091);
#18746=PLANE('',#21092);
#18747=PLANE('',#21093);
#18748=PLANE('',#21094);
#18749=PLANE('',#21095);
#18750=PLANE('',#21096);
#18751=PLANE('',#21097);
#18752=PLANE('',#21098);
#18753=PLANE('',#21099);
#18754=PLANE('',#21100);
#18755=PLANE('',#21101);
#18756=PLANE('',#21102);
#18757=PLANE('',#21103);
#18758=PLANE('',#21104);
#18759=PLANE('',#21105);
#18760=PLANE('',#21106);
#18761=PLANE('',#21107);
#18762=PLANE('',#21108);
#18763=PLANE('',#21109);
#18764=PLANE('',#21110);
#18765=PLANE('',#21111);
#18766=PLANE('',#21112);
#18767=PLANE('',#21113);
#18768=PLANE('',#21117);
#18769=PLANE('',#21118);
#18770=PLANE('',#21119);
#18771=PLANE('',#21120);
#18772=PLANE('',#21121);
#18773=PLANE('',#21122);
#18774=PLANE('',#21123);
#18775=PLANE('',#21124);
#18776=PLANE('',#21128);
#18777=PLANE('',#21132);
#18778=PLANE('',#21133);
#18779=PLANE('',#21134);
#18780=PLANE('',#21135);
#18781=PLANE('',#21136);
#18782=PLANE('',#21137);
#18783=PLANE('',#21138);
#18784=PLANE('',#21139);
#18785=PLANE('',#21140);
#18786=PLANE('',#21141);
#18787=PLANE('',#21142);
#18788=PLANE('',#21146);
#18789=PLANE('',#21150);
#18790=PLANE('',#21151);
#18791=PLANE('',#21152);
#18792=PLANE('',#21153);
#18793=PLANE('',#21154);
#18794=PLANE('',#21155);
#18795=PLANE('',#21156);
#18796=PLANE('',#21157);
#18797=PLANE('',#21158);
#18798=PLANE('',#21162);
#18799=PLANE('',#21163);
#18800=PLANE('',#21164);
#18801=PLANE('',#21165);
#18802=PLANE('',#21166);
#18803=PLANE('',#21167);
#18804=PLANE('',#21168);
#18805=PLANE('',#21169);
#18806=PLANE('',#21173);
#18807=PLANE('',#21177);
#18808=PLANE('',#21178);
#18809=PLANE('',#21179);
#18810=PLANE('',#21180);
#18811=PLANE('',#21181);
#18812=PLANE('',#21182);
#18813=PLANE('',#21183);
#18814=PLANE('',#21184);
#18815=PLANE('',#21185);
#18816=PLANE('',#21186);
#18817=PLANE('',#21187);
#18818=PLANE('',#21188);
#18819=PLANE('',#21192);
#18820=PLANE('',#21196);
#18821=PLANE('',#21200);
#18822=PLANE('',#21201);
#18823=PLANE('',#21202);
#18824=PLANE('',#21203);
#18825=PLANE('',#21204);
#18826=PLANE('',#21205);
#18827=PLANE('',#21206);
#18828=PLANE('',#21207);
#18829=PLANE('',#21208);
#18830=PLANE('',#21212);
#18831=PLANE('',#21213);
#18832=PLANE('',#21214);
#18833=PLANE('',#21215);
#18834=PLANE('',#21216);
#18835=PLANE('',#21217);
#18836=PLANE('',#21218);
#18837=PLANE('',#21219);
#18838=PLANE('',#21220);
#18839=PLANE('',#21221);
#18840=PLANE('',#21222);
#18841=PLANE('',#21223);
#18842=PLANE('',#21224);
#18843=PLANE('',#21225);
#18844=PLANE('',#21226);
#18845=PLANE('',#21227);
#18846=PLANE('',#21228);
#18847=PLANE('',#21229);
#18848=PLANE('',#21230);
#18849=PLANE('',#21231);
#18850=PLANE('',#21232);
#18851=PLANE('',#21233);
#18852=PLANE('',#21234);
#18853=PLANE('',#21235);
#18854=PLANE('',#21236);
#18855=PLANE('',#21237);
#18856=PLANE('',#21238);
#18857=PLANE('',#21239);
#18858=PLANE('',#21240);
#18859=PLANE('',#21241);
#18860=PLANE('',#21242);
#18861=PLANE('',#21243);
#18862=PLANE('',#21244);
#18863=PLANE('',#21245);
#18864=PLANE('',#21246);
#18865=PLANE('',#21247);
#18866=PLANE('',#21248);
#18867=PLANE('',#21249);
#18868=PLANE('',#21250);
#18869=PLANE('',#21251);
#18870=PLANE('',#21252);
#18871=PLANE('',#21253);
#18872=PLANE('',#21254);
#18873=PLANE('',#21258);
#18874=PLANE('',#21259);
#18875=PLANE('',#21260);
#18876=PLANE('',#21261);
#18877=PLANE('',#21262);
#18878=PLANE('',#21263);
#18879=PLANE('',#21264);
#18880=PLANE('',#21265);
#18881=PLANE('',#21266);
#18882=PLANE('',#21267);
#18883=PLANE('',#21268);
#18884=PLANE('',#21269);
#18885=PLANE('',#21270);
#18886=PLANE('',#21271);
#18887=PLANE('',#21272);
#18888=PLANE('',#21273);
#18889=PLANE('',#21274);
#18890=PLANE('',#21275);
#18891=PLANE('',#21276);
#18892=PLANE('',#21277);
#18893=PLANE('',#21278);
#18894=PLANE('',#21279);
#18895=PLANE('',#21280);
#18896=PLANE('',#21281);
#18897=PLANE('',#21282);
#18898=PLANE('',#21283);
#18899=PLANE('',#21284);
#18900=PLANE('',#21285);
#18901=PLANE('',#21286);
#18902=PLANE('',#21287);
#18903=PLANE('',#21288);
#18904=PLANE('',#21289);
#18905=PLANE('',#21290);
#18906=PLANE('',#21291);
#18907=PLANE('',#21292);
#18908=PLANE('',#21293);
#18909=PLANE('',#21294);
#18910=PLANE('',#21295);
#18911=PLANE('',#21296);
#18912=PLANE('',#21297);
#18913=PLANE('',#21298);
#18914=PLANE('',#21299);
#18915=PLANE('',#21300);
#18916=PLANE('',#21301);
#18917=PLANE('',#21305);
#18918=PLANE('',#21306);
#18919=PLANE('',#21307);
#18920=PLANE('',#21308);
#18921=PLANE('',#21309);
#18922=PLANE('',#21310);
#18923=PLANE('',#21311);
#18924=PLANE('',#21312);
#18925=PLANE('',#21313);
#18926=PLANE('',#21317);
#18927=PLANE('',#21321);
#18928=PLANE('',#21322);
#18929=PLANE('',#21323);
#18930=PLANE('',#21324);
#18931=PLANE('',#21325);
#18932=PLANE('',#21326);
#18933=PLANE('',#21327);
#18934=PLANE('',#21328);
#18935=PLANE('',#21329);
#18936=PLANE('',#21330);
#18937=PLANE('',#21331);
#18938=PLANE('',#21335);
#18939=PLANE('',#21339);
#18940=PLANE('',#21340);
#18941=PLANE('',#21341);
#18942=PLANE('',#21342);
#18943=PLANE('',#21343);
#18944=PLANE('',#21344);
#18945=PLANE('',#21345);
#18946=PLANE('',#21346);
#18947=PLANE('',#21347);
#18948=PLANE('',#21351);
#18949=PLANE('',#21352);
#18950=PLANE('',#21353);
#18951=PLANE('',#21354);
#18952=PLANE('',#21355);
#18953=PLANE('',#21356);
#18954=PLANE('',#21357);
#18955=PLANE('',#21358);
#18956=PLANE('',#21365);
#18957=PLANE('',#21368);
#18958=PLANE('',#21371);
#18959=PLANE('',#21372);
#18960=PLANE('',#21373);
#18961=PLANE('',#21374);
#18962=PLANE('',#21375);
#18963=PLANE('',#21376);
#18964=PLANE('',#21377);
#18965=PLANE('',#21378);
#18966=PLANE('',#21379);
#18967=PLANE('',#21380);
#18968=PLANE('',#21381);
#18969=PLANE('',#21382);
#18970=PLANE('',#21385);
#18971=PLANE('',#21388);
#18972=PLANE('',#21391);
#18973=PLANE('',#21392);
#18974=PLANE('',#21393);
#18975=PLANE('',#21394);
#18976=PLANE('',#21395);
#18977=PLANE('',#21396);
#18978=PLANE('',#21397);
#18979=PLANE('',#21398);
#18980=PLANE('',#21399);
#18981=PLANE('',#21402);
#18982=PLANE('',#21403);
#18983=PLANE('',#21404);
#18984=PLANE('',#21405);
#18985=PLANE('',#21406);
#18986=PLANE('',#21407);
#18987=PLANE('',#21408);
#18988=PLANE('',#21409);
#18989=PLANE('',#21644);
#18990=PLANE('',#21650);
#18991=PLANE('',#21651);
#18992=PLANE('',#21655);
#18993=PLANE('',#21657);
#18994=PLANE('',#21661);
#18995=PLANE('',#21664);
#18996=PLANE('',#21720);
#18997=PLANE('',#21723);
#18998=PLANE('',#21724);
#18999=PLANE('',#21725);
#19000=PLANE('',#21726);
#19001=PLANE('',#21727);
#19002=PLANE('',#21728);
#19003=PLANE('',#21729);
#19004=PLANE('',#21730);
#19005=PLANE('',#21731);
#19006=PLANE('',#21732);
#19007=PLANE('',#21733);
#19008=PLANE('',#21734);
#19009=PLANE('',#21735);
#19010=PLANE('',#21737);
#19011=PLANE('',#21747);
#19012=PLANE('',#21757);
#19013=PLANE('',#21761);
#19014=PLANE('',#21765);
#19015=PLANE('',#21769);
#19016=PLANE('',#21770);
#19017=PLANE('',#21771);
#19018=PLANE('',#21781);
#19019=PLANE('',#21788);
#19020=PLANE('',#21795);
#19021=PLANE('',#21798);
#19022=PLANE('',#21801);
#19023=PLANE('',#21804);
#19024=PLANE('',#21805);
#19025=PLANE('',#21806);
#19026=PLANE('',#21807);
#19027=PLANE('',#21808);
#19028=PLANE('',#21813);
#19029=PLANE('',#21814);
#19030=PLANE('',#21815);
#19031=PLANE('',#21816);
#19032=PLANE('',#21817);
#19033=PLANE('',#21818);
#19034=PLANE('',#21823);
#19035=PLANE('',#21824);
#19036=PLANE('',#21825);
#19037=PLANE('',#21826);
#19038=PLANE('',#21827);
#19039=PLANE('',#21828);
#19040=PLANE('',#21833);
#19041=PLANE('',#21834);
#19042=PLANE('',#21835);
#19043=PLANE('',#21836);
#19044=PLANE('',#21837);
#19045=PLANE('',#21838);
#19046=PLANE('',#21840);
#19047=PLANE('',#21850);
#19048=PLANE('',#21860);
#19049=PLANE('',#21864);
#19050=PLANE('',#21868);
#19051=PLANE('',#21872);
#19052=PLANE('',#21873);
#19053=PLANE('',#21874);
#19054=PLANE('',#21884);
#19055=PLANE('',#21891);
#19056=PLANE('',#21898);
#19057=PLANE('',#21901);
#19058=PLANE('',#21904);
#19059=PLANE('',#21907);
#19060=PLANE('',#21908);
#19061=PLANE('',#21909);
#19062=PLANE('',#21910);
#19063=PLANE('',#21911);
#19064=ADVANCED_FACE('',(#1207),#18535,.T.);
#19065=ADVANCED_FACE('',(#1208),#18536,.F.);
#19066=ADVANCED_FACE('',(#1209),#781,.F.);
#19067=ADVANCED_FACE('',(#1210),#782,.T.);
#19068=ADVANCED_FACE('',(#1211),#783,.F.);
#19069=ADVANCED_FACE('',(#1212),#18537,.F.);
#19070=ADVANCED_FACE('',(#1213),#784,.F.);
#19071=ADVANCED_FACE('',(#1214),#785,.T.);
#19072=ADVANCED_FACE('',(#1215),#786,.F.);
#19073=ADVANCED_FACE('',(#1216),#18538,.F.);
#19074=ADVANCED_FACE('',(#1217),#787,.T.);
#19075=ADVANCED_FACE('',(#1218),#18539,.F.);
#19076=ADVANCED_FACE('',(#1219),#788,.T.);
#19077=ADVANCED_FACE('',(#1220),#18540,.F.);
#19078=ADVANCED_FACE('',(#1221),#18541,.F.);
#19079=ADVANCED_FACE('',(#1222),#18542,.F.);
#19080=ADVANCED_FACE('',(#1223),#18543,.F.);
#19081=ADVANCED_FACE('',(#1224),#18544,.F.);
#19082=ADVANCED_FACE('',(#1225),#18545,.F.);
#19083=ADVANCED_FACE('',(#1226),#18546,.F.);
#19084=ADVANCED_FACE('',(#1227),#18547,.F.);
#19085=ADVANCED_FACE('',(#1228),#789,.T.);
#19086=ADVANCED_FACE('',(#1229),#18548,.F.);
#19087=ADVANCED_FACE('',(#1230),#18549,.F.);
#19088=ADVANCED_FACE('',(#1231),#18550,.F.);
#19089=ADVANCED_FACE('',(#1232),#18551,.F.);
#19090=ADVANCED_FACE('',(#1233),#18552,.F.);
#19091=ADVANCED_FACE('',(#1234),#18553,.F.);
#19092=ADVANCED_FACE('',(#1235),#790,.F.);
#19093=ADVANCED_FACE('',(#1236),#791,.T.);
#19094=ADVANCED_FACE('',(#1237),#792,.F.);
#19095=ADVANCED_FACE('',(#1238),#18554,.F.);
#19096=ADVANCED_FACE('',(#1239),#793,.F.);
#19097=ADVANCED_FACE('',(#1240),#794,.T.);
#19098=ADVANCED_FACE('',(#1241),#795,.F.);
#19099=ADVANCED_FACE('',(#1242),#18555,.F.);
#19100=ADVANCED_FACE('',(#1243),#796,.T.);
#19101=ADVANCED_FACE('',(#1244),#18556,.F.);
#19102=ADVANCED_FACE('',(#1245),#18557,.F.);
#19103=ADVANCED_FACE('',(#1246),#797,.F.);
#19104=ADVANCED_FACE('',(#1247),#798,.T.);
#19105=ADVANCED_FACE('',(#1248),#799,.F.);
#19106=ADVANCED_FACE('',(#1249),#18558,.F.);
#19107=ADVANCED_FACE('',(#1250),#800,.F.);
#19108=ADVANCED_FACE('',(#1251),#801,.T.);
#19109=ADVANCED_FACE('',(#1252),#18559,.F.);
#19110=ADVANCED_FACE('',(#1253),#18560,.F.);
#19111=ADVANCED_FACE('',(#1254),#18561,.F.);
#19112=ADVANCED_FACE('',(#1255),#18562,.F.);
#19113=ADVANCED_FACE('',(#1256,#635,#636),#18563,.F.);
#19114=ADVANCED_FACE('',(#1257),#802,.F.);
#19115=ADVANCED_FACE('',(#1258),#18564,.F.);
#19116=ADVANCED_FACE('',(#1259),#18565,.T.);
#19117=ADVANCED_FACE('',(#1260),#18566,.T.);
#19118=ADVANCED_FACE('',(#1261),#18567,.T.);
#19119=ADVANCED_FACE('',(#1262),#18568,.T.);
#19120=ADVANCED_FACE('',(#1263,#637,#638),#18569,.T.);
#19121=ADVANCED_FACE('',(#1264),#803,.F.);
#19122=ADVANCED_FACE('',(#1265),#804,.F.);
#19123=ADVANCED_FACE('',(#1266),#805,.F.);
#19124=ADVANCED_FACE('',(#1267),#806,.F.);
#19125=ADVANCED_FACE('',(#1268),#807,.F.);
#19126=ADVANCED_FACE('',(#1269),#18570,.F.);
#19127=ADVANCED_FACE('',(#1270),#18571,.F.);
#19128=ADVANCED_FACE('',(#1271,#639,#640),#18572,.F.);
#19129=ADVANCED_FACE('',(#1272),#18573,.F.);
#19130=ADVANCED_FACE('',(#1273),#808,.T.);
#19131=ADVANCED_FACE('',(#1274),#18574,.F.);
#19132=ADVANCED_FACE('',(#1275),#809,.T.);
#19133=ADVANCED_FACE('',(#1276),#18575,.F.);
#19134=ADVANCED_FACE('',(#1277),#810,.F.);
#19135=ADVANCED_FACE('',(#1278),#18576,.F.);
#19136=ADVANCED_FACE('',(#1279),#18577,.F.);
#19137=ADVANCED_FACE('',(#1280,#641,#642),#18578,.F.);
#19138=ADVANCED_FACE('',(#1281),#18579,.F.);
#19139=ADVANCED_FACE('',(#1282),#811,.T.);
#19140=ADVANCED_FACE('',(#1283),#18580,.F.);
#19141=ADVANCED_FACE('',(#1284),#812,.T.);
#19142=ADVANCED_FACE('',(#1285),#18581,.F.);
#19143=ADVANCED_FACE('',(#1286),#813,.F.);
#19144=ADVANCED_FACE('',(#1287),#814,.T.);
#19145=ADVANCED_FACE('',(#1288),#815,.F.);
#19146=ADVANCED_FACE('',(#1289),#18582,.F.);
#19147=ADVANCED_FACE('',(#1290),#816,.F.);
#19148=ADVANCED_FACE('',(#1291),#817,.T.);
#19149=ADVANCED_FACE('',(#1292),#818,.F.);
#19150=ADVANCED_FACE('',(#1293),#18583,.F.);
#19151=ADVANCED_FACE('',(#1294),#18584,.F.);
#19152=ADVANCED_FACE('',(#1295),#819,.F.);
#19153=ADVANCED_FACE('',(#1296),#18585,.F.);
#19154=ADVANCED_FACE('',(#1297),#820,.T.);
#19155=ADVANCED_FACE('',(#1298),#18586,.F.);
#19156=ADVANCED_FACE('',(#1299),#821,.T.);
#19157=ADVANCED_FACE('',(#1300),#18587,.F.);
#19158=ADVANCED_FACE('',(#1301),#18588,.F.);
#19159=ADVANCED_FACE('',(#1302),#18589,.F.);
#19160=ADVANCED_FACE('',(#1303),#18590,.F.);
#19161=ADVANCED_FACE('',(#1304),#18591,.F.);
#19162=ADVANCED_FACE('',(#1305),#18592,.F.);
#19163=ADVANCED_FACE('',(#1306),#18593,.F.);
#19164=ADVANCED_FACE('',(#1307),#18594,.F.);
#19165=ADVANCED_FACE('',(#1308),#18595,.F.);
#19166=ADVANCED_FACE('',(#1309),#18596,.F.);
#19167=ADVANCED_FACE('',(#1310),#822,.T.);
#19168=ADVANCED_FACE('',(#1311),#18597,.T.);
#19169=ADVANCED_FACE('',(#1312),#18598,.F.);
#19170=ADVANCED_FACE('',(#1313),#18599,.F.);
#19171=ADVANCED_FACE('',(#1314),#823,.T.);
#19172=ADVANCED_FACE('',(#1315),#18600,.F.);
#19173=ADVANCED_FACE('',(#1316),#824,.F.);
#19174=ADVANCED_FACE('',(#1317),#825,.T.);
#19175=ADVANCED_FACE('',(#1318),#826,.F.);
#19176=ADVANCED_FACE('',(#1319),#18601,.F.);
#19177=ADVANCED_FACE('',(#1320),#827,.F.);
#19178=ADVANCED_FACE('',(#1321),#828,.T.);
#19179=ADVANCED_FACE('',(#1322),#829,.F.);
#19180=ADVANCED_FACE('',(#1323),#18602,.F.);
#19181=ADVANCED_FACE('',(#1324),#18603,.F.);
#19182=ADVANCED_FACE('',(#1325),#18604,.F.);
#19183=ADVANCED_FACE('',(#1326),#830,.F.);
#19184=ADVANCED_FACE('',(#1327),#831,.T.);
#19185=ADVANCED_FACE('',(#1328),#832,.F.);
#19186=ADVANCED_FACE('',(#1329),#18605,.F.);
#19187=ADVANCED_FACE('',(#1330),#833,.F.);
#19188=ADVANCED_FACE('',(#1331),#834,.T.);
#19189=ADVANCED_FACE('',(#1332),#18606,.F.);
#19190=ADVANCED_FACE('',(#1333),#18607,.F.);
#19191=ADVANCED_FACE('',(#1334),#18608,.T.);
#19192=ADVANCED_FACE('',(#1335),#835,.F.);
#19193=ADVANCED_FACE('',(#1336),#836,.T.);
#19194=ADVANCED_FACE('',(#1337),#837,.F.);
#19195=ADVANCED_FACE('',(#1338),#18609,.T.);
#19196=ADVANCED_FACE('',(#1339),#838,.F.);
#19197=ADVANCED_FACE('',(#1340),#839,.T.);
#19198=ADVANCED_FACE('',(#1341),#840,.F.);
#19199=ADVANCED_FACE('',(#1342),#18610,.T.);
#19200=ADVANCED_FACE('',(#1343),#841,.T.);
#19201=ADVANCED_FACE('',(#1344),#18611,.T.);
#19202=ADVANCED_FACE('',(#1345),#842,.T.);
#19203=ADVANCED_FACE('',(#1346),#18612,.T.);
#19204=ADVANCED_FACE('',(#1347),#18613,.T.);
#19205=ADVANCED_FACE('',(#1348),#18614,.T.);
#19206=ADVANCED_FACE('',(#1349),#18615,.T.);
#19207=ADVANCED_FACE('',(#1350),#18616,.T.);
#19208=ADVANCED_FACE('',(#1351),#18617,.T.);
#19209=ADVANCED_FACE('',(#1352),#18618,.T.);
#19210=ADVANCED_FACE('',(#1353),#18619,.T.);
#19211=ADVANCED_FACE('',(#1354),#843,.T.);
#19212=ADVANCED_FACE('',(#1355),#18620,.T.);
#19213=ADVANCED_FACE('',(#1356),#18621,.T.);
#19214=ADVANCED_FACE('',(#1357),#18622,.T.);
#19215=ADVANCED_FACE('',(#1358),#18623,.T.);
#19216=ADVANCED_FACE('',(#1359),#18624,.T.);
#19217=ADVANCED_FACE('',(#1360),#18625,.T.);
#19218=ADVANCED_FACE('',(#1361),#844,.F.);
#19219=ADVANCED_FACE('',(#1362),#845,.T.);
#19220=ADVANCED_FACE('',(#1363),#846,.F.);
#19221=ADVANCED_FACE('',(#1364),#18626,.T.);
#19222=ADVANCED_FACE('',(#1365),#847,.F.);
#19223=ADVANCED_FACE('',(#1366),#848,.T.);
#19224=ADVANCED_FACE('',(#1367),#849,.F.);
#19225=ADVANCED_FACE('',(#1368),#18627,.T.);
#19226=ADVANCED_FACE('',(#1369),#850,.T.);
#19227=ADVANCED_FACE('',(#1370),#18628,.T.);
#19228=ADVANCED_FACE('',(#1371),#18629,.T.);
#19229=ADVANCED_FACE('',(#1372),#851,.F.);
#19230=ADVANCED_FACE('',(#1373),#852,.T.);
#19231=ADVANCED_FACE('',(#1374),#853,.F.);
#19232=ADVANCED_FACE('',(#1375),#18630,.T.);
#19233=ADVANCED_FACE('',(#1376),#854,.F.);
#19234=ADVANCED_FACE('',(#1377),#855,.T.);
#19235=ADVANCED_FACE('',(#1378),#18631,.T.);
#19236=ADVANCED_FACE('',(#1379),#18632,.T.);
#19237=ADVANCED_FACE('',(#1380),#18633,.T.);
#19238=ADVANCED_FACE('',(#1381),#18634,.T.);
#19239=ADVANCED_FACE('',(#1382,#643,#644),#18635,.T.);
#19240=ADVANCED_FACE('',(#1383),#856,.F.);
#19241=ADVANCED_FACE('',(#1384),#18636,.T.);
#19242=ADVANCED_FACE('',(#1385),#18637,.F.);
#19243=ADVANCED_FACE('',(#1386),#18638,.F.);
#19244=ADVANCED_FACE('',(#1387),#18639,.F.);
#19245=ADVANCED_FACE('',(#1388),#18640,.F.);
#19246=ADVANCED_FACE('',(#1389,#645,#646),#18641,.F.);
#19247=ADVANCED_FACE('',(#1390),#857,.F.);
#19248=ADVANCED_FACE('',(#1391),#858,.F.);
#19249=ADVANCED_FACE('',(#1392),#859,.F.);
#19250=ADVANCED_FACE('',(#1393),#860,.F.);
#19251=ADVANCED_FACE('',(#1394),#861,.F.);
#19252=ADVANCED_FACE('',(#1395),#18642,.T.);
#19253=ADVANCED_FACE('',(#1396),#18643,.T.);
#19254=ADVANCED_FACE('',(#1397,#647,#648),#18644,.T.);
#19255=ADVANCED_FACE('',(#1398),#18645,.T.);
#19256=ADVANCED_FACE('',(#1399),#862,.T.);
#19257=ADVANCED_FACE('',(#1400),#18646,.T.);
#19258=ADVANCED_FACE('',(#1401),#863,.T.);
#19259=ADVANCED_FACE('',(#1402),#18647,.T.);
#19260=ADVANCED_FACE('',(#1403),#864,.F.);
#19261=ADVANCED_FACE('',(#1404),#18648,.T.);
#19262=ADVANCED_FACE('',(#1405),#18649,.T.);
#19263=ADVANCED_FACE('',(#1406,#649,#650),#18650,.T.);
#19264=ADVANCED_FACE('',(#1407),#18651,.T.);
#19265=ADVANCED_FACE('',(#1408),#865,.T.);
#19266=ADVANCED_FACE('',(#1409),#18652,.T.);
#19267=ADVANCED_FACE('',(#1410),#866,.T.);
#19268=ADVANCED_FACE('',(#1411),#18653,.T.);
#19269=ADVANCED_FACE('',(#1412),#867,.F.);
#19270=ADVANCED_FACE('',(#1413),#868,.T.);
#19271=ADVANCED_FACE('',(#1414),#869,.F.);
#19272=ADVANCED_FACE('',(#1415),#18654,.T.);
#19273=ADVANCED_FACE('',(#1416),#870,.F.);
#19274=ADVANCED_FACE('',(#1417),#871,.T.);
#19275=ADVANCED_FACE('',(#1418),#872,.F.);
#19276=ADVANCED_FACE('',(#1419),#18655,.T.);
#19277=ADVANCED_FACE('',(#1420),#18656,.T.);
#19278=ADVANCED_FACE('',(#1421),#873,.F.);
#19279=ADVANCED_FACE('',(#1422),#18657,.T.);
#19280=ADVANCED_FACE('',(#1423),#874,.T.);
#19281=ADVANCED_FACE('',(#1424),#18658,.T.);
#19282=ADVANCED_FACE('',(#1425),#875,.T.);
#19283=ADVANCED_FACE('',(#1426),#18659,.T.);
#19284=ADVANCED_FACE('',(#1427),#18660,.T.);
#19285=ADVANCED_FACE('',(#1428),#18661,.T.);
#19286=ADVANCED_FACE('',(#1429),#18662,.T.);
#19287=ADVANCED_FACE('',(#1430),#18663,.T.);
#19288=ADVANCED_FACE('',(#1431),#18664,.T.);
#19289=ADVANCED_FACE('',(#1432),#18665,.T.);
#19290=ADVANCED_FACE('',(#1433),#18666,.T.);
#19291=ADVANCED_FACE('',(#1434),#18667,.T.);
#19292=ADVANCED_FACE('',(#1435),#18668,.T.);
#19293=ADVANCED_FACE('',(#1436),#876,.T.);
#19294=ADVANCED_FACE('',(#1437),#18669,.F.);
#19295=ADVANCED_FACE('',(#1438),#18670,.T.);
#19296=ADVANCED_FACE('',(#1439),#18671,.T.);
#19297=ADVANCED_FACE('',(#1440),#877,.T.);
#19298=ADVANCED_FACE('',(#1441),#18672,.T.);
#19299=ADVANCED_FACE('',(#1442),#878,.F.);
#19300=ADVANCED_FACE('',(#1443),#879,.T.);
#19301=ADVANCED_FACE('',(#1444),#880,.F.);
#19302=ADVANCED_FACE('',(#1445),#18673,.T.);
#19303=ADVANCED_FACE('',(#1446),#881,.F.);
#19304=ADVANCED_FACE('',(#1447),#882,.T.);
#19305=ADVANCED_FACE('',(#1448),#883,.F.);
#19306=ADVANCED_FACE('',(#1449),#18674,.T.);
#19307=ADVANCED_FACE('',(#1450),#18675,.T.);
#19308=ADVANCED_FACE('',(#1451),#18676,.T.);
#19309=ADVANCED_FACE('',(#1452),#884,.F.);
#19310=ADVANCED_FACE('',(#1453),#885,.T.);
#19311=ADVANCED_FACE('',(#1454),#886,.F.);
#19312=ADVANCED_FACE('',(#1455),#18677,.T.);
#19313=ADVANCED_FACE('',(#1456),#887,.F.);
#19314=ADVANCED_FACE('',(#1457),#888,.T.);
#19315=ADVANCED_FACE('',(#1458),#18678,.T.);
#19316=ADVANCED_FACE('',(#1459),#889,.F.);
#19317=ADVANCED_FACE('',(#1460),#594,.T.);
#19318=ADVANCED_FACE('',(#1461),#595,.T.);
#19319=ADVANCED_FACE('',(#1462),#536,.T.);
#19320=ADVANCED_FACE('',(#1463),#596,.F.);
#19321=ADVANCED_FACE('',(#1464),#537,.F.);
#19322=ADVANCED_FACE('',(#1465),#597,.F.);
#19323=ADVANCED_FACE('',(#1466),#598,.T.);
#19324=ADVANCED_FACE('',(#1467),#538,.T.);
#19325=ADVANCED_FACE('',(#1468),#539,.T.);
#19326=ADVANCED_FACE('',(#1469),#540,.T.);
#19327=ADVANCED_FACE('',(#1470),#541,.T.);
#19328=ADVANCED_FACE('',(#1471),#542,.T.);
#19329=ADVANCED_FACE('',(#1472),#543,.T.);
#19330=ADVANCED_FACE('',(#1473),#544,.T.);
#19331=ADVANCED_FACE('',(#1474),#545,.T.);
#19332=ADVANCED_FACE('',(#1475),#546,.F.);
#19333=ADVANCED_FACE('',(#1476),#547,.F.);
#19334=ADVANCED_FACE('',(#1477),#548,.F.);
#19335=ADVANCED_FACE('',(#1478),#549,.F.);
#19336=ADVANCED_FACE('',(#1479),#550,.F.);
#19337=ADVANCED_FACE('',(#1480),#551,.F.);
#19338=ADVANCED_FACE('',(#1481),#552,.F.);
#19339=ADVANCED_FACE('',(#1482),#553,.F.);
#19340=ADVANCED_FACE('',(#1483),#554,.F.);
#19341=ADVANCED_FACE('',(#1484),#555,.F.);
#19342=ADVANCED_FACE('',(#1485),#556,.F.);
#19343=ADVANCED_FACE('',(#1486),#557,.F.);
#19344=ADVANCED_FACE('',(#1487),#558,.F.);
#19345=ADVANCED_FACE('',(#1488),#559,.F.);
#19346=ADVANCED_FACE('',(#1489),#560,.F.);
#19347=ADVANCED_FACE('',(#1490),#561,.F.);
#19348=ADVANCED_FACE('',(#1491,#651),#18679,.T.);
#19349=ADVANCED_FACE('',(#1492,#652),#18680,.T.);
#19350=ADVANCED_FACE('',(#1493),#18681,.T.);
#19351=ADVANCED_FACE('',(#1494),#18682,.T.);
#19352=ADVANCED_FACE('',(#1495),#18683,.F.);
#19353=ADVANCED_FACE('',(#1496),#18684,.T.);
#19354=ADVANCED_FACE('',(#1497),#18685,.T.);
#19355=ADVANCED_FACE('',(#1498),#18686,.F.);
#19356=ADVANCED_FACE('',(#1499),#18687,.T.);
#19357=ADVANCED_FACE('',(#1500),#18688,.T.);
#19358=ADVANCED_FACE('',(#1501),#18689,.F.);
#19359=ADVANCED_FACE('',(#1502),#18690,.T.);
#19360=ADVANCED_FACE('',(#1503),#18691,.T.);
#19361=ADVANCED_FACE('',(#1504),#18692,.F.);
#19362=ADVANCED_FACE('',(#1505),#18693,.T.);
#19363=ADVANCED_FACE('',(#1506),#18694,.T.);
#19364=ADVANCED_FACE('',(#1507),#18695,.F.);
#19365=ADVANCED_FACE('',(#1508),#18696,.T.);
#19366=ADVANCED_FACE('',(#1509),#18697,.T.);
#19367=ADVANCED_FACE('',(#1510),#18698,.F.);
#19368=ADVANCED_FACE('',(#1511),#18699,.T.);
#19369=ADVANCED_FACE('',(#1512),#18700,.T.);
#19370=ADVANCED_FACE('',(#1513),#18701,.F.);
#19371=ADVANCED_FACE('',(#1514),#18702,.T.);
#19372=ADVANCED_FACE('',(#1515),#18703,.T.);
#19373=ADVANCED_FACE('',(#1516),#18704,.F.);
#19374=ADVANCED_FACE('',(#1517),#528,.T.);
#19375=ADVANCED_FACE('',(#1518),#599,.F.);
#19376=ADVANCED_FACE('',(#1519),#600,.T.);
#19377=ADVANCED_FACE('',(#1520),#562,.F.);
#19378=ADVANCED_FACE('',(#1521),#890,.F.);
#19379=ADVANCED_FACE('',(#1522),#563,.F.);
#19380=ADVANCED_FACE('',(#1523),#601,.T.);
#19381=ADVANCED_FACE('',(#1524),#602,.T.);
#19382=ADVANCED_FACE('',(#1525),#603,.T.);
#19383=ADVANCED_FACE('',(#1526),#891,.T.);
#19384=ADVANCED_FACE('',(#1527),#892,.T.);
#19385=ADVANCED_FACE('',(#1528,#653),#18705,.F.);
#19386=ADVANCED_FACE('',(#1529,#654),#18706,.F.);
#19387=ADVANCED_FACE('',(#1530),#604,.F.);
#19388=ADVANCED_FACE('',(#1531),#893,.T.);
#19389=ADVANCED_FACE('',(#1532),#605,.T.);
#19390=ADVANCED_FACE('',(#1533),#564,.T.);
#19391=ADVANCED_FACE('',(#1534),#565,.T.);
#19392=ADVANCED_FACE('',(#1535),#606,.T.);
#19393=ADVANCED_FACE('',(#1536),#894,.F.);
#19394=ADVANCED_FACE('',(#1537),#895,.F.);
#19395=ADVANCED_FACE('',(#1538,#655),#18707,.F.);
#19396=ADVANCED_FACE('',(#1539,#656),#18708,.F.);
#19397=ADVANCED_FACE('',(#1540),#529,.T.);
#19398=ADVANCED_FACE('',(#1541),#530,.T.);
#19399=ADVANCED_FACE('',(#1542),#531,.T.);
#19400=ADVANCED_FACE('',(#1543),#532,.T.);
#19401=ADVANCED_FACE('',(#1544),#533,.T.);
#19402=ADVANCED_FACE('',(#1545),#534,.T.);
#19403=ADVANCED_FACE('',(#1546),#535,.T.);
#19404=ADVANCED_FACE('',(#1547),#607,.F.);
#19405=ADVANCED_FACE('',(#1548),#896,.F.);
#19406=ADVANCED_FACE('',(#1549),#608,.T.);
#19407=ADVANCED_FACE('',(#1550),#609,.T.);
#19408=ADVANCED_FACE('',(#1551),#566,.T.);
#19409=ADVANCED_FACE('',(#1552),#610,.F.);
#19410=ADVANCED_FACE('',(#1553),#611,.F.);
#19411=ADVANCED_FACE('',(#1554),#567,.F.);
#19412=ADVANCED_FACE('',(#1555),#612,.T.);
#19413=ADVANCED_FACE('',(#1556),#568,.T.);
#19414=ADVANCED_FACE('',(#1557),#569,.T.);
#19415=ADVANCED_FACE('',(#1558),#570,.T.);
#19416=ADVANCED_FACE('',(#1559),#571,.T.);
#19417=ADVANCED_FACE('',(#1560),#572,.T.);
#19418=ADVANCED_FACE('',(#1561),#573,.T.);
#19419=ADVANCED_FACE('',(#1562),#574,.T.);
#19420=ADVANCED_FACE('',(#1563),#575,.T.);
#19421=ADVANCED_FACE('',(#1564),#576,.F.);
#19422=ADVANCED_FACE('',(#1565),#577,.F.);
#19423=ADVANCED_FACE('',(#1566),#578,.F.);
#19424=ADVANCED_FACE('',(#1567),#579,.F.);
#19425=ADVANCED_FACE('',(#1568),#580,.F.);
#19426=ADVANCED_FACE('',(#1569),#581,.F.);
#19427=ADVANCED_FACE('',(#1570),#582,.F.);
#19428=ADVANCED_FACE('',(#1571),#583,.F.);
#19429=ADVANCED_FACE('',(#1572),#584,.F.);
#19430=ADVANCED_FACE('',(#1573),#585,.F.);
#19431=ADVANCED_FACE('',(#1574),#586,.F.);
#19432=ADVANCED_FACE('',(#1575),#587,.F.);
#19433=ADVANCED_FACE('',(#1576),#588,.F.);
#19434=ADVANCED_FACE('',(#1577),#589,.F.);
#19435=ADVANCED_FACE('',(#1578),#590,.F.);
#19436=ADVANCED_FACE('',(#1579),#591,.F.);
#19437=ADVANCED_FACE('',(#1580,#657),#18709,.T.);
#19438=ADVANCED_FACE('',(#1581,#658),#18710,.T.);
#19439=ADVANCED_FACE('',(#1582),#18711,.T.);
#19440=ADVANCED_FACE('',(#1583),#18712,.T.);
#19441=ADVANCED_FACE('',(#1584),#18713,.F.);
#19442=ADVANCED_FACE('',(#1585),#18714,.T.);
#19443=ADVANCED_FACE('',(#1586),#18715,.T.);
#19444=ADVANCED_FACE('',(#1587),#18716,.F.);
#19445=ADVANCED_FACE('',(#1588),#18717,.T.);
#19446=ADVANCED_FACE('',(#1589),#18718,.T.);
#19447=ADVANCED_FACE('',(#1590),#18719,.F.);
#19448=ADVANCED_FACE('',(#1591),#18720,.T.);
#19449=ADVANCED_FACE('',(#1592),#18721,.T.);
#19450=ADVANCED_FACE('',(#1593),#18722,.F.);
#19451=ADVANCED_FACE('',(#1594),#18723,.T.);
#19452=ADVANCED_FACE('',(#1595),#18724,.T.);
#19453=ADVANCED_FACE('',(#1596),#18725,.F.);
#19454=ADVANCED_FACE('',(#1597),#18726,.T.);
#19455=ADVANCED_FACE('',(#1598),#18727,.T.);
#19456=ADVANCED_FACE('',(#1599),#18728,.F.);
#19457=ADVANCED_FACE('',(#1600),#18729,.T.);
#19458=ADVANCED_FACE('',(#1601),#18730,.T.);
#19459=ADVANCED_FACE('',(#1602),#18731,.F.);
#19460=ADVANCED_FACE('',(#1603),#18732,.T.);
#19461=ADVANCED_FACE('',(#1604),#18733,.T.);
#19462=ADVANCED_FACE('',(#1605),#18734,.F.);
#19463=ADVANCED_FACE('',(#1606),#18735,.T.);
#19464=ADVANCED_FACE('',(#1607),#18736,.T.);
#19465=ADVANCED_FACE('',(#1608),#18737,.T.);
#19466=ADVANCED_FACE('',(#1609),#18738,.T.);
#19467=ADVANCED_FACE('',(#1610),#18739,.T.);
#19468=ADVANCED_FACE('',(#1611),#18740,.T.);
#19469=ADVANCED_FACE('',(#1612),#18741,.T.);
#19470=ADVANCED_FACE('',(#1613),#18742,.T.);
#19471=ADVANCED_FACE('',(#1614),#18743,.T.);
#19472=ADVANCED_FACE('',(#1615),#18744,.F.);
#19473=ADVANCED_FACE('',(#1616),#18745,.F.);
#19474=ADVANCED_FACE('',(#1617),#18746,.F.);
#19475=ADVANCED_FACE('',(#1618),#18747,.F.);
#19476=ADVANCED_FACE('',(#1619),#18748,.F.);
#19477=ADVANCED_FACE('',(#1620),#18749,.F.);
#19478=ADVANCED_FACE('',(#1621),#18750,.F.);
#19479=ADVANCED_FACE('',(#1622),#18751,.F.);
#19480=ADVANCED_FACE('',(#1623),#18752,.F.);
#19481=ADVANCED_FACE('',(#1624),#18753,.F.);
#19482=ADVANCED_FACE('',(#1625),#18754,.F.);
#19483=ADVANCED_FACE('',(#1626),#18755,.F.);
#19484=ADVANCED_FACE('',(#1627),#18756,.F.);
#19485=ADVANCED_FACE('',(#1628),#18757,.F.);
#19486=ADVANCED_FACE('',(#1629),#18758,.F.);
#19487=ADVANCED_FACE('',(#1630),#18759,.F.);
#19488=ADVANCED_FACE('',(#1631),#18760,.F.);
#19489=ADVANCED_FACE('',(#1632),#18761,.F.);
#19490=ADVANCED_FACE('',(#1633),#18762,.F.);
#19491=ADVANCED_FACE('',(#1634),#18763,.F.);
#19492=ADVANCED_FACE('',(#1635),#18764,.T.);
#19493=ADVANCED_FACE('',(#1636),#18765,.T.);
#19494=ADVANCED_FACE('',(#1637),#18766,.T.);
#19495=ADVANCED_FACE('',(#1638),#18767,.T.);
#19496=ADVANCED_FACE('',(#1639),#897,.F.);
#19497=ADVANCED_FACE('',(#1640),#18768,.T.);
#19498=ADVANCED_FACE('',(#1641),#18769,.T.);
#19499=ADVANCED_FACE('',(#1642),#18770,.T.);
#19500=ADVANCED_FACE('',(#1643),#18771,.T.);
#19501=ADVANCED_FACE('',(#1644),#18772,.T.);
#19502=ADVANCED_FACE('',(#1645),#18773,.T.);
#19503=ADVANCED_FACE('',(#1646),#18774,.T.);
#19504=ADVANCED_FACE('',(#1647),#18775,.F.);
#19505=ADVANCED_FACE('',(#1648),#898,.F.);
#19506=ADVANCED_FACE('',(#1649),#18776,.F.);
#19507=ADVANCED_FACE('',(#1650),#899,.F.);
#19508=ADVANCED_FACE('',(#1651),#18777,.F.);
#19509=ADVANCED_FACE('',(#1652),#18778,.F.);
#19510=ADVANCED_FACE('',(#1653),#18779,.F.);
#19511=ADVANCED_FACE('',(#1654),#18780,.F.);
#19512=ADVANCED_FACE('',(#1655),#18781,.F.);
#19513=ADVANCED_FACE('',(#1656),#18782,.F.);
#19514=ADVANCED_FACE('',(#1657),#18783,.F.);
#19515=ADVANCED_FACE('',(#1658),#18784,.F.);
#19516=ADVANCED_FACE('',(#1659),#18785,.F.);
#19517=ADVANCED_FACE('',(#1660),#18786,.F.);
#19518=ADVANCED_FACE('',(#1661),#18787,.F.);
#19519=ADVANCED_FACE('',(#1662),#900,.F.);
#19520=ADVANCED_FACE('',(#1663),#18788,.F.);
#19521=ADVANCED_FACE('',(#1664),#901,.F.);
#19522=ADVANCED_FACE('',(#1665),#18789,.F.);
#19523=ADVANCED_FACE('',(#1666),#18790,.F.);
#19524=ADVANCED_FACE('',(#1667),#18791,.F.);
#19525=ADVANCED_FACE('',(#1668),#18792,.F.);
#19526=ADVANCED_FACE('',(#1669),#18793,.F.);
#19527=ADVANCED_FACE('',(#1670),#18794,.F.);
#19528=ADVANCED_FACE('',(#1671),#18795,.F.);
#19529=ADVANCED_FACE('',(#1672),#18796,.F.);
#19530=ADVANCED_FACE('',(#1673),#18797,.F.);
#19531=ADVANCED_FACE('',(#1674),#902,.T.);
#19532=ADVANCED_FACE('',(#1675),#18798,.F.);
#19533=ADVANCED_FACE('',(#1676),#18799,.F.);
#19534=ADVANCED_FACE('',(#1677),#18800,.F.);
#19535=ADVANCED_FACE('',(#1678),#18801,.F.);
#19536=ADVANCED_FACE('',(#1679),#18802,.F.);
#19537=ADVANCED_FACE('',(#1680),#18803,.F.);
#19538=ADVANCED_FACE('',(#1681),#18804,.F.);
#19539=ADVANCED_FACE('',(#1682),#18805,.T.);
#19540=ADVANCED_FACE('',(#1683),#903,.F.);
#19541=ADVANCED_FACE('',(#1684),#18806,.T.);
#19542=ADVANCED_FACE('',(#1685),#904,.F.);
#19543=ADVANCED_FACE('',(#1686),#18807,.T.);
#19544=ADVANCED_FACE('',(#1687),#18808,.T.);
#19545=ADVANCED_FACE('',(#1688),#18809,.T.);
#19546=ADVANCED_FACE('',(#1689),#18810,.T.);
#19547=ADVANCED_FACE('',(#1690),#18811,.T.);
#19548=ADVANCED_FACE('',(#1691),#18812,.T.);
#19549=ADVANCED_FACE('',(#1692),#18813,.T.);
#19550=ADVANCED_FACE('',(#1693),#18814,.T.);
#19551=ADVANCED_FACE('',(#1694),#18815,.T.);
#19552=ADVANCED_FACE('',(#1695),#18816,.T.);
#19553=ADVANCED_FACE('',(#1696),#18817,.T.);
#19554=ADVANCED_FACE('',(#1697),#18818,.T.);
#19555=ADVANCED_FACE('',(#1698),#905,.F.);
#19556=ADVANCED_FACE('',(#1699),#18819,.T.);
#19557=ADVANCED_FACE('',(#1700),#906,.F.);
#19558=ADVANCED_FACE('',(#1701),#18820,.T.);
#19559=ADVANCED_FACE('',(#1702),#907,.F.);
#19560=ADVANCED_FACE('',(#1703),#18821,.T.);
#19561=ADVANCED_FACE('',(#1704),#18822,.T.);
#19562=ADVANCED_FACE('',(#1705),#18823,.T.);
#19563=ADVANCED_FACE('',(#1706),#18824,.T.);
#19564=ADVANCED_FACE('',(#1707),#18825,.T.);
#19565=ADVANCED_FACE('',(#1708),#18826,.T.);
#19566=ADVANCED_FACE('',(#1709),#18827,.T.);
#19567=ADVANCED_FACE('',(#1710),#18828,.T.);
#19568=ADVANCED_FACE('',(#1711),#18829,.T.);
#19569=ADVANCED_FACE('',(#1712),#908,.T.);
#19570=ADVANCED_FACE('',(#1713),#18830,.T.);
#19571=ADVANCED_FACE('',(#1714),#18831,.T.);
#19572=ADVANCED_FACE('',(#1715),#18832,.T.);
#19573=ADVANCED_FACE('',(#1716),#18833,.T.);
#19574=ADVANCED_FACE('',(#1717),#18834,.T.);
#19575=ADVANCED_FACE('',(#1718),#18835,.T.);
#19576=ADVANCED_FACE('',(#1719),#18836,.T.);
#19577=ADVANCED_FACE('',(#1720),#18837,.T.);
#19578=ADVANCED_FACE('',(#1721),#18838,.T.);
#19579=ADVANCED_FACE('',(#1722),#18839,.T.);
#19580=ADVANCED_FACE('',(#1723),#18840,.T.);
#19581=ADVANCED_FACE('',(#1724),#18841,.T.);
#19582=ADVANCED_FACE('',(#1725),#18842,.T.);
#19583=ADVANCED_FACE('',(#1726),#18843,.T.);
#19584=ADVANCED_FACE('',(#1727),#18844,.T.);
#19585=ADVANCED_FACE('',(#1728),#18845,.T.);
#19586=ADVANCED_FACE('',(#1729),#18846,.F.);
#19587=ADVANCED_FACE('',(#1730),#18847,.F.);
#19588=ADVANCED_FACE('',(#1731),#18848,.F.);
#19589=ADVANCED_FACE('',(#1732),#18849,.F.);
#19590=ADVANCED_FACE('',(#1733),#18850,.F.);
#19591=ADVANCED_FACE('',(#1734),#18851,.F.);
#19592=ADVANCED_FACE('',(#1735),#18852,.F.);
#19593=ADVANCED_FACE('',(#1736),#18853,.F.);
#19594=ADVANCED_FACE('',(#1737),#18854,.F.);
#19595=ADVANCED_FACE('',(#1738),#18855,.F.);
#19596=ADVANCED_FACE('',(#1739),#18856,.F.);
#19597=ADVANCED_FACE('',(#1740),#18857,.F.);
#19598=ADVANCED_FACE('',(#1741),#18858,.F.);
#19599=ADVANCED_FACE('',(#1742),#18859,.F.);
#19600=ADVANCED_FACE('',(#1743),#18860,.F.);
#19601=ADVANCED_FACE('',(#1744),#18861,.F.);
#19602=ADVANCED_FACE('',(#1745),#18862,.F.);
#19603=ADVANCED_FACE('',(#1746),#18863,.F.);
#19604=ADVANCED_FACE('',(#1747),#18864,.F.);
#19605=ADVANCED_FACE('',(#1748),#18865,.F.);
#19606=ADVANCED_FACE('',(#1749),#18866,.F.);
#19607=ADVANCED_FACE('',(#1750),#18867,.F.);
#19608=ADVANCED_FACE('',(#1751),#18868,.T.);
#19609=ADVANCED_FACE('',(#1752),#18869,.T.);
#19610=ADVANCED_FACE('',(#1753),#18870,.T.);
#19611=ADVANCED_FACE('',(#1754),#18871,.T.);
#19612=ADVANCED_FACE('',(#1755),#18872,.T.);
#19613=ADVANCED_FACE('',(#1756),#909,.F.);
#19614=ADVANCED_FACE('',(#1757),#18873,.T.);
#19615=ADVANCED_FACE('',(#1758),#18874,.T.);
#19616=ADVANCED_FACE('',(#1759),#18875,.T.);
#19617=ADVANCED_FACE('',(#1760),#18876,.T.);
#19618=ADVANCED_FACE('',(#1761),#18877,.T.);
#19619=ADVANCED_FACE('',(#1762),#18878,.T.);
#19620=ADVANCED_FACE('',(#1763),#18879,.T.);
#19621=ADVANCED_FACE('',(#1764),#18880,.T.);
#19622=ADVANCED_FACE('',(#1765),#18881,.T.);
#19623=ADVANCED_FACE('',(#1766),#18882,.T.);
#19624=ADVANCED_FACE('',(#1767),#18883,.T.);
#19625=ADVANCED_FACE('',(#1768),#18884,.T.);
#19626=ADVANCED_FACE('',(#1769),#18885,.T.);
#19627=ADVANCED_FACE('',(#1770),#18886,.T.);
#19628=ADVANCED_FACE('',(#1771),#18887,.T.);
#19629=ADVANCED_FACE('',(#1772),#18888,.T.);
#19630=ADVANCED_FACE('',(#1773),#18889,.T.);
#19631=ADVANCED_FACE('',(#1774),#18890,.F.);
#19632=ADVANCED_FACE('',(#1775),#18891,.F.);
#19633=ADVANCED_FACE('',(#1776),#18892,.F.);
#19634=ADVANCED_FACE('',(#1777),#18893,.F.);
#19635=ADVANCED_FACE('',(#1778),#18894,.F.);
#19636=ADVANCED_FACE('',(#1779),#18895,.F.);
#19637=ADVANCED_FACE('',(#1780),#18896,.F.);
#19638=ADVANCED_FACE('',(#1781),#18897,.F.);
#19639=ADVANCED_FACE('',(#1782),#18898,.F.);
#19640=ADVANCED_FACE('',(#1783),#18899,.F.);
#19641=ADVANCED_FACE('',(#1784),#18900,.F.);
#19642=ADVANCED_FACE('',(#1785),#18901,.F.);
#19643=ADVANCED_FACE('',(#1786),#18902,.F.);
#19644=ADVANCED_FACE('',(#1787),#18903,.F.);
#19645=ADVANCED_FACE('',(#1788),#18904,.F.);
#19646=ADVANCED_FACE('',(#1789),#18905,.F.);
#19647=ADVANCED_FACE('',(#1790),#18906,.F.);
#19648=ADVANCED_FACE('',(#1791),#18907,.F.);
#19649=ADVANCED_FACE('',(#1792),#18908,.F.);
#19650=ADVANCED_FACE('',(#1793),#18909,.F.);
#19651=ADVANCED_FACE('',(#1794),#18910,.F.);
#19652=ADVANCED_FACE('',(#1795),#18911,.F.);
#19653=ADVANCED_FACE('',(#1796),#18912,.T.);
#19654=ADVANCED_FACE('',(#1797),#18913,.T.);
#19655=ADVANCED_FACE('',(#1798),#18914,.T.);
#19656=ADVANCED_FACE('',(#1799),#18915,.T.);
#19657=ADVANCED_FACE('',(#1800),#18916,.T.);
#19658=ADVANCED_FACE('',(#1801),#910,.F.);
#19659=ADVANCED_FACE('',(#1802),#18917,.T.);
#19660=ADVANCED_FACE('',(#1803),#18918,.T.);
#19661=ADVANCED_FACE('',(#1804),#18919,.T.);
#19662=ADVANCED_FACE('',(#1805),#18920,.T.);
#19663=ADVANCED_FACE('',(#1806),#18921,.T.);
#19664=ADVANCED_FACE('',(#1807),#18922,.T.);
#19665=ADVANCED_FACE('',(#1808),#18923,.T.);
#19666=ADVANCED_FACE('',(#1809),#18924,.T.);
#19667=ADVANCED_FACE('',(#1810),#18925,.F.);
#19668=ADVANCED_FACE('',(#1811),#911,.F.);
#19669=ADVANCED_FACE('',(#1812),#18926,.F.);
#19670=ADVANCED_FACE('',(#1813),#912,.F.);
#19671=ADVANCED_FACE('',(#1814),#18927,.F.);
#19672=ADVANCED_FACE('',(#1815),#18928,.F.);
#19673=ADVANCED_FACE('',(#1816),#18929,.F.);
#19674=ADVANCED_FACE('',(#1817),#18930,.F.);
#19675=ADVANCED_FACE('',(#1818),#18931,.F.);
#19676=ADVANCED_FACE('',(#1819),#18932,.F.);
#19677=ADVANCED_FACE('',(#1820),#18933,.F.);
#19678=ADVANCED_FACE('',(#1821),#18934,.F.);
#19679=ADVANCED_FACE('',(#1822),#18935,.F.);
#19680=ADVANCED_FACE('',(#1823),#18936,.F.);
#19681=ADVANCED_FACE('',(#1824),#18937,.F.);
#19682=ADVANCED_FACE('',(#1825),#913,.F.);
#19683=ADVANCED_FACE('',(#1826),#18938,.F.);
#19684=ADVANCED_FACE('',(#1827),#914,.F.);
#19685=ADVANCED_FACE('',(#1828),#18939,.F.);
#19686=ADVANCED_FACE('',(#1829),#18940,.F.);
#19687=ADVANCED_FACE('',(#1830),#18941,.F.);
#19688=ADVANCED_FACE('',(#1831),#18942,.F.);
#19689=ADVANCED_FACE('',(#1832),#18943,.F.);
#19690=ADVANCED_FACE('',(#1833),#18944,.F.);
#19691=ADVANCED_FACE('',(#1834),#18945,.F.);
#19692=ADVANCED_FACE('',(#1835),#18946,.F.);
#19693=ADVANCED_FACE('',(#1836),#18947,.F.);
#19694=ADVANCED_FACE('',(#1837),#915,.T.);
#19695=ADVANCED_FACE('',(#1838),#18948,.F.);
#19696=ADVANCED_FACE('',(#1839),#18949,.F.);
#19697=ADVANCED_FACE('',(#1840),#18950,.F.);
#19698=ADVANCED_FACE('',(#1841),#18951,.F.);
#19699=ADVANCED_FACE('',(#1842),#18952,.F.);
#19700=ADVANCED_FACE('',(#1843),#18953,.F.);
#19701=ADVANCED_FACE('',(#1844),#18954,.F.);
#19702=ADVANCED_FACE('',(#1845,#659,#660,#661,#662,#663,#664,#665,#666,
#667,#668,#669,#670,#671),#18955,.F.);
#19703=ADVANCED_FACE('',(#1846),#18956,.T.);
#19704=ADVANCED_FACE('',(#1847),#916,.F.);
#19705=ADVANCED_FACE('',(#1848),#18957,.T.);
#19706=ADVANCED_FACE('',(#1849),#917,.F.);
#19707=ADVANCED_FACE('',(#1850),#18958,.T.);
#19708=ADVANCED_FACE('',(#1851),#18959,.T.);
#19709=ADVANCED_FACE('',(#1852),#18960,.T.);
#19710=ADVANCED_FACE('',(#1853),#18961,.T.);
#19711=ADVANCED_FACE('',(#1854),#18962,.T.);
#19712=ADVANCED_FACE('',(#1855),#18963,.T.);
#19713=ADVANCED_FACE('',(#1856),#18964,.T.);
#19714=ADVANCED_FACE('',(#1857),#18965,.T.);
#19715=ADVANCED_FACE('',(#1858),#18966,.T.);
#19716=ADVANCED_FACE('',(#1859),#18967,.T.);
#19717=ADVANCED_FACE('',(#1860),#18968,.T.);
#19718=ADVANCED_FACE('',(#1861),#18969,.T.);
#19719=ADVANCED_FACE('',(#1862),#918,.F.);
#19720=ADVANCED_FACE('',(#1863),#18970,.T.);
#19721=ADVANCED_FACE('',(#1864),#919,.F.);
#19722=ADVANCED_FACE('',(#1865),#18971,.T.);
#19723=ADVANCED_FACE('',(#1866),#920,.F.);
#19724=ADVANCED_FACE('',(#1867),#18972,.T.);
#19725=ADVANCED_FACE('',(#1868),#18973,.T.);
#19726=ADVANCED_FACE('',(#1869),#18974,.T.);
#19727=ADVANCED_FACE('',(#1870),#18975,.T.);
#19728=ADVANCED_FACE('',(#1871),#18976,.T.);
#19729=ADVANCED_FACE('',(#1872),#18977,.T.);
#19730=ADVANCED_FACE('',(#1873),#18978,.T.);
#19731=ADVANCED_FACE('',(#1874),#18979,.T.);
#19732=ADVANCED_FACE('',(#1875),#18980,.T.);
#19733=ADVANCED_FACE('',(#1876),#921,.T.);
#19734=ADVANCED_FACE('',(#1877),#18981,.T.);
#19735=ADVANCED_FACE('',(#1878),#18982,.T.);
#19736=ADVANCED_FACE('',(#1879),#18983,.T.);
#19737=ADVANCED_FACE('',(#1880),#18984,.T.);
#19738=ADVANCED_FACE('',(#1881),#18985,.T.);
#19739=ADVANCED_FACE('',(#1882),#18986,.T.);
#19740=ADVANCED_FACE('',(#1883),#18987,.T.);
#19741=ADVANCED_FACE('',(#1884,#672,#673,#674,#675,#676,#677,#678,#679,
#680,#681,#682,#683,#684),#18988,.T.);
#19742=ADVANCED_FACE('',(#1885),#922,.T.);
#19743=ADVANCED_FACE('',(#1886),#923,.T.);
#19744=ADVANCED_FACE('',(#1887),#924,.T.);
#19745=ADVANCED_FACE('',(#1888),#925,.T.);
#19746=ADVANCED_FACE('',(#1889),#926,.T.);
#19747=ADVANCED_FACE('',(#1890),#927,.T.);
#19748=ADVANCED_FACE('',(#1891),#928,.T.);
#19749=ADVANCED_FACE('',(#1892),#929,.T.);
#19750=ADVANCED_FACE('',(#1893),#930,.T.);
#19751=ADVANCED_FACE('',(#1894),#931,.T.);
#19752=ADVANCED_FACE('',(#1895),#932,.T.);
#19753=ADVANCED_FACE('',(#1896),#933,.T.);
#19754=ADVANCED_FACE('',(#1897),#934,.T.);
#19755=ADVANCED_FACE('',(#1898),#935,.T.);
#19756=ADVANCED_FACE('',(#1899),#936,.T.);
#19757=ADVANCED_FACE('',(#1900),#937,.T.);
#19758=ADVANCED_FACE('',(#1901),#938,.T.);
#19759=ADVANCED_FACE('',(#1902),#939,.T.);
#19760=ADVANCED_FACE('',(#1903),#940,.T.);
#19761=ADVANCED_FACE('',(#1904),#941,.T.);
#19762=ADVANCED_FACE('',(#1905),#942,.T.);
#19763=ADVANCED_FACE('',(#1906),#943,.T.);
#19764=ADVANCED_FACE('',(#1907),#944,.T.);
#19765=ADVANCED_FACE('',(#1908),#945,.T.);
#19766=ADVANCED_FACE('',(#1909),#946,.T.);
#19767=ADVANCED_FACE('',(#1910),#947,.T.);
#19768=ADVANCED_FACE('',(#1911),#948,.T.);
#19769=ADVANCED_FACE('',(#1912),#949,.T.);
#19770=ADVANCED_FACE('',(#1913),#950,.T.);
#19771=ADVANCED_FACE('',(#1914),#951,.T.);
#19772=ADVANCED_FACE('',(#1915),#952,.T.);
#19773=ADVANCED_FACE('',(#1916),#953,.T.);
#19774=ADVANCED_FACE('',(#1917),#954,.T.);
#19775=ADVANCED_FACE('',(#1918),#955,.T.);
#19776=ADVANCED_FACE('',(#1919),#956,.T.);
#19777=ADVANCED_FACE('',(#1920),#957,.T.);
#19778=ADVANCED_FACE('',(#1921),#958,.T.);
#19779=ADVANCED_FACE('',(#1922),#959,.T.);
#19780=ADVANCED_FACE('',(#1923),#960,.T.);
#19781=ADVANCED_FACE('',(#1924),#961,.T.);
#19782=ADVANCED_FACE('',(#1925),#962,.T.);
#19783=ADVANCED_FACE('',(#1926),#963,.T.);
#19784=ADVANCED_FACE('',(#1927),#964,.T.);
#19785=ADVANCED_FACE('',(#1928),#965,.T.);
#19786=ADVANCED_FACE('',(#1929),#966,.T.);
#19787=ADVANCED_FACE('',(#1930),#967,.T.);
#19788=ADVANCED_FACE('',(#1931),#968,.T.);
#19789=ADVANCED_FACE('',(#1932),#969,.T.);
#19790=ADVANCED_FACE('',(#1933),#970,.T.);
#19791=ADVANCED_FACE('',(#1934),#971,.T.);
#19792=ADVANCED_FACE('',(#1935),#972,.T.);
#19793=ADVANCED_FACE('',(#1936),#973,.T.);
#19794=ADVANCED_FACE('',(#1937),#974,.T.);
#19795=ADVANCED_FACE('',(#1938),#975,.T.);
#19796=ADVANCED_FACE('',(#1939),#976,.T.);
#19797=ADVANCED_FACE('',(#1940),#977,.T.);
#19798=ADVANCED_FACE('',(#1941),#978,.T.);
#19799=ADVANCED_FACE('',(#1942),#979,.T.);
#19800=ADVANCED_FACE('',(#1943),#980,.T.);
#19801=ADVANCED_FACE('',(#1944),#981,.T.);
#19802=ADVANCED_FACE('',(#1945),#982,.T.);
#19803=ADVANCED_FACE('',(#1946),#983,.T.);
#19804=ADVANCED_FACE('',(#1947),#984,.T.);
#19805=ADVANCED_FACE('',(#1948),#985,.T.);
#19806=ADVANCED_FACE('',(#1949),#986,.T.);
#19807=ADVANCED_FACE('',(#1950),#987,.T.);
#19808=ADVANCED_FACE('',(#1951),#988,.T.);
#19809=ADVANCED_FACE('',(#1952),#989,.T.);
#19810=ADVANCED_FACE('',(#1953),#990,.T.);
#19811=ADVANCED_FACE('',(#1954),#991,.T.);
#19812=ADVANCED_FACE('',(#1955),#992,.T.);
#19813=ADVANCED_FACE('',(#1956),#993,.T.);
#19814=ADVANCED_FACE('',(#1957),#994,.T.);
#19815=ADVANCED_FACE('',(#1958),#995,.T.);
#19816=ADVANCED_FACE('',(#1959),#996,.T.);
#19817=ADVANCED_FACE('',(#1960),#997,.T.);
#19818=ADVANCED_FACE('',(#1961),#998,.T.);
#19819=ADVANCED_FACE('',(#1962),#999,.T.);
#19820=ADVANCED_FACE('',(#1963),#1000,.T.);
#19821=ADVANCED_FACE('',(#1964),#1001,.T.);
#19822=ADVANCED_FACE('',(#1965),#1002,.T.);
#19823=ADVANCED_FACE('',(#1966),#1003,.T.);
#19824=ADVANCED_FACE('',(#1967),#1004,.T.);
#19825=ADVANCED_FACE('',(#1968),#1005,.T.);
#19826=ADVANCED_FACE('',(#1969),#1006,.T.);
#19827=ADVANCED_FACE('',(#1970),#1007,.T.);
#19828=ADVANCED_FACE('',(#1971),#1008,.T.);
#19829=ADVANCED_FACE('',(#1972),#1009,.T.);
#19830=ADVANCED_FACE('',(#1973),#1010,.T.);
#19831=ADVANCED_FACE('',(#1974),#1011,.T.);
#19832=ADVANCED_FACE('',(#1975),#1012,.T.);
#19833=ADVANCED_FACE('',(#1976),#1013,.T.);
#19834=ADVANCED_FACE('',(#1977),#1014,.T.);
#19835=ADVANCED_FACE('',(#1978),#1015,.T.);
#19836=ADVANCED_FACE('',(#1979),#1016,.T.);
#19837=ADVANCED_FACE('',(#1980),#1017,.T.);
#19838=ADVANCED_FACE('',(#1981),#1018,.T.);
#19839=ADVANCED_FACE('',(#1982),#1019,.T.);
#19840=ADVANCED_FACE('',(#1983),#1020,.T.);
#19841=ADVANCED_FACE('',(#1984),#1021,.T.);
#19842=ADVANCED_FACE('',(#1985),#1022,.T.);
#19843=ADVANCED_FACE('',(#1986),#1023,.T.);
#19844=ADVANCED_FACE('',(#1987),#1024,.T.);
#19845=ADVANCED_FACE('',(#1988),#1025,.T.);
#19846=ADVANCED_FACE('',(#1989),#1026,.T.);
#19847=ADVANCED_FACE('',(#1990),#1027,.T.);
#19848=ADVANCED_FACE('',(#1991),#1028,.T.);
#19849=ADVANCED_FACE('',(#1992),#1029,.T.);
#19850=ADVANCED_FACE('',(#1993),#1030,.T.);
#19851=ADVANCED_FACE('',(#1994),#1031,.T.);
#19852=ADVANCED_FACE('',(#1995),#1032,.T.);
#19853=ADVANCED_FACE('',(#1996),#1033,.T.);
#19854=ADVANCED_FACE('',(#1997),#1034,.T.);
#19855=ADVANCED_FACE('',(#1998),#1035,.T.);
#19856=ADVANCED_FACE('',(#1999),#1036,.T.);
#19857=ADVANCED_FACE('',(#2000),#1037,.T.);
#19858=ADVANCED_FACE('',(#2001),#1038,.T.);
#19859=ADVANCED_FACE('',(#2002),#1039,.T.);
#19860=ADVANCED_FACE('',(#2003),#1040,.T.);
#19861=ADVANCED_FACE('',(#2004),#1041,.T.);
#19862=ADVANCED_FACE('',(#2005),#1042,.T.);
#19863=ADVANCED_FACE('',(#2006),#1043,.T.);
#19864=ADVANCED_FACE('',(#2007),#1044,.T.);
#19865=ADVANCED_FACE('',(#2008),#1045,.T.);
#19866=ADVANCED_FACE('',(#2009),#1046,.T.);
#19867=ADVANCED_FACE('',(#2010),#1047,.T.);
#19868=ADVANCED_FACE('',(#2011),#1048,.T.);
#19869=ADVANCED_FACE('',(#2012),#1049,.T.);
#19870=ADVANCED_FACE('',(#2013),#1050,.T.);
#19871=ADVANCED_FACE('',(#2014),#1051,.T.);
#19872=ADVANCED_FACE('',(#2015),#1052,.T.);
#19873=ADVANCED_FACE('',(#2016),#1053,.T.);
#19874=ADVANCED_FACE('',(#2017),#1054,.T.);
#19875=ADVANCED_FACE('',(#2018),#1055,.T.);
#19876=ADVANCED_FACE('',(#2019),#1056,.T.);
#19877=ADVANCED_FACE('',(#2020),#1057,.T.);
#19878=ADVANCED_FACE('',(#2021),#1058,.T.);
#19879=ADVANCED_FACE('',(#2022),#1059,.T.);
#19880=ADVANCED_FACE('',(#2023),#1060,.T.);
#19881=ADVANCED_FACE('',(#2024),#1061,.T.);
#19882=ADVANCED_FACE('',(#2025),#1062,.T.);
#19883=ADVANCED_FACE('',(#2026),#1063,.T.);
#19884=ADVANCED_FACE('',(#2027),#1064,.T.);
#19885=ADVANCED_FACE('',(#2028),#1065,.T.);
#19886=ADVANCED_FACE('',(#2029),#1066,.T.);
#19887=ADVANCED_FACE('',(#2030),#1067,.T.);
#19888=ADVANCED_FACE('',(#2031),#1068,.T.);
#19889=ADVANCED_FACE('',(#2032),#1069,.T.);
#19890=ADVANCED_FACE('',(#2033),#1070,.T.);
#19891=ADVANCED_FACE('',(#2034),#1071,.T.);
#19892=ADVANCED_FACE('',(#2035),#1072,.T.);
#19893=ADVANCED_FACE('',(#2036),#1073,.T.);
#19894=ADVANCED_FACE('',(#2037),#1074,.T.);
#19895=ADVANCED_FACE('',(#2038),#1075,.T.);
#19896=ADVANCED_FACE('',(#2039),#1076,.T.);
#19897=ADVANCED_FACE('',(#2040),#1077,.T.);
#19898=ADVANCED_FACE('',(#2041),#1078,.T.);
#19899=ADVANCED_FACE('',(#2042),#1079,.T.);
#19900=ADVANCED_FACE('',(#2043),#1080,.T.);
#19901=ADVANCED_FACE('',(#2044),#1081,.T.);
#19902=ADVANCED_FACE('',(#2045),#1082,.T.);
#19903=ADVANCED_FACE('',(#2046),#1083,.T.);
#19904=ADVANCED_FACE('',(#2047),#1084,.T.);
#19905=ADVANCED_FACE('',(#2048),#1085,.T.);
#19906=ADVANCED_FACE('',(#2049),#1086,.T.);
#19907=ADVANCED_FACE('',(#2050),#1087,.T.);
#19908=ADVANCED_FACE('',(#2051),#1088,.T.);
#19909=ADVANCED_FACE('',(#2052),#1089,.T.);
#19910=ADVANCED_FACE('',(#2053),#1090,.T.);
#19911=ADVANCED_FACE('',(#2054),#1091,.T.);
#19912=ADVANCED_FACE('',(#2055),#1092,.T.);
#19913=ADVANCED_FACE('',(#2056),#1093,.T.);
#19914=ADVANCED_FACE('',(#2057),#1094,.T.);
#19915=ADVANCED_FACE('',(#2058),#1095,.T.);
#19916=ADVANCED_FACE('',(#2059),#1096,.T.);
#19917=ADVANCED_FACE('',(#2060),#1097,.T.);
#19918=ADVANCED_FACE('',(#2061),#1098,.T.);
#19919=ADVANCED_FACE('',(#2062),#1099,.T.);
#19920=ADVANCED_FACE('',(#2063),#1100,.T.);
#19921=ADVANCED_FACE('',(#2064),#1101,.T.);
#19922=ADVANCED_FACE('',(#2065),#1102,.T.);
#19923=ADVANCED_FACE('',(#2066),#1103,.T.);
#19924=ADVANCED_FACE('',(#2067),#1104,.T.);
#19925=ADVANCED_FACE('',(#2068),#1105,.T.);
#19926=ADVANCED_FACE('',(#2069),#1106,.T.);
#19927=ADVANCED_FACE('',(#2070),#1107,.T.);
#19928=ADVANCED_FACE('',(#2071),#1108,.T.);
#19929=ADVANCED_FACE('',(#2072),#1109,.T.);
#19930=ADVANCED_FACE('',(#2073),#1110,.T.);
#19931=ADVANCED_FACE('',(#2074),#1111,.T.);
#19932=ADVANCED_FACE('',(#2075),#1112,.T.);
#19933=ADVANCED_FACE('',(#2076),#1113,.T.);
#19934=ADVANCED_FACE('',(#2077),#1114,.T.);
#19935=ADVANCED_FACE('',(#2078),#1115,.T.);
#19936=ADVANCED_FACE('',(#2079),#1116,.T.);
#19937=ADVANCED_FACE('',(#2080),#1117,.T.);
#19938=ADVANCED_FACE('',(#2081),#1118,.T.);
#19939=ADVANCED_FACE('',(#2082),#1119,.T.);
#19940=ADVANCED_FACE('',(#2083),#1120,.T.);
#19941=ADVANCED_FACE('',(#2084),#1121,.T.);
#19942=ADVANCED_FACE('',(#2085),#1122,.T.);
#19943=ADVANCED_FACE('',(#2086),#1123,.T.);
#19944=ADVANCED_FACE('',(#2087),#1124,.T.);
#19945=ADVANCED_FACE('',(#2088),#1125,.T.);
#19946=ADVANCED_FACE('',(#2089),#1126,.T.);
#19947=ADVANCED_FACE('',(#2090),#1127,.T.);
#19948=ADVANCED_FACE('',(#2091),#1128,.T.);
#19949=ADVANCED_FACE('',(#2092),#1129,.T.);
#19950=ADVANCED_FACE('',(#2093),#1130,.T.);
#19951=ADVANCED_FACE('',(#2094),#1131,.T.);
#19952=ADVANCED_FACE('',(#2095),#1132,.T.);
#19953=ADVANCED_FACE('',(#2096),#1133,.T.);
#19954=ADVANCED_FACE('',(#2097),#1134,.T.);
#19955=ADVANCED_FACE('',(#2098),#1135,.T.);
#19956=ADVANCED_FACE('',(#2099),#1136,.T.);
#19957=ADVANCED_FACE('',(#2100),#1137,.T.);
#19958=ADVANCED_FACE('',(#2101),#1138,.T.);
#19959=ADVANCED_FACE('',(#2102),#1139,.T.);
#19960=ADVANCED_FACE('',(#2103),#1140,.T.);
#19961=ADVANCED_FACE('',(#2104),#1141,.T.);
#19962=ADVANCED_FACE('',(#2105),#1142,.T.);
#19963=ADVANCED_FACE('',(#2106),#592,.T.);
#19964=ADVANCED_FACE('',(#2107),#1143,.T.);
#19965=ADVANCED_FACE('',(#2108),#18989,.T.);
#19966=ADVANCED_FACE('',(#2109),#593,.T.);
#19967=ADVANCED_FACE('',(#2110),#1144,.T.);
#19968=ADVANCED_FACE('',(#2111),#18990,.T.);
#19969=ADVANCED_FACE('',(#2112,#685),#18991,.T.);
#19970=ADVANCED_FACE('',(#2113),#67,.F.);
#19971=ADVANCED_FACE('',(#2114),#1145,.T.);
#19972=ADVANCED_FACE('',(#2115,#686),#18992,.F.);
#19973=ADVANCED_FACE('',(#2116),#68,.T.);
#19974=ADVANCED_FACE('',(#2117),#18993,.F.);
#19975=ADVANCED_FACE('',(#2118),#1146,.T.);
#19976=ADVANCED_FACE('',(#2119),#69,.T.);
#19977=ADVANCED_FACE('',(#2120),#1147,.T.);
#19978=ADVANCED_FACE('',(#2121,#687),#18994,.T.);
#19979=ADVANCED_FACE('',(#2122),#70,.F.);
#19980=ADVANCED_FACE('',(#2123),#1148,.T.);
#19981=ADVANCED_FACE('',(#2124,#688),#18995,.T.);
#19982=ADVANCED_FACE('',(#2125),#1149,.F.);
#19983=ADVANCED_FACE('',(#2126),#1150,.F.);
#19984=ADVANCED_FACE('',(#2127),#1151,.F.);
#19985=ADVANCED_FACE('',(#2128),#1152,.F.);
#19986=ADVANCED_FACE('',(#2129),#1153,.F.);
#19987=ADVANCED_FACE('',(#2130),#1154,.F.);
#19988=ADVANCED_FACE('',(#2131),#1155,.F.);
#19989=ADVANCED_FACE('',(#2132),#1156,.F.);
#19990=ADVANCED_FACE('',(#2133),#1157,.F.);
#19991=ADVANCED_FACE('',(#2134),#1158,.F.);
#19992=ADVANCED_FACE('',(#2135),#1159,.F.);
#19993=ADVANCED_FACE('',(#2136),#1160,.F.);
#19994=ADVANCED_FACE('',(#2137),#1161,.F.);
#19995=ADVANCED_FACE('',(#2138),#1162,.F.);
#19996=ADVANCED_FACE('',(#2139),#1163,.F.);
#19997=ADVANCED_FACE('',(#2140),#1164,.F.);
#19998=ADVANCED_FACE('',(#2141),#1165,.F.);
#19999=ADVANCED_FACE('',(#2142),#1166,.T.);
#20000=ADVANCED_FACE('',(#2143),#18996,.T.);
#20001=ADVANCED_FACE('',(#2144),#1167,.T.);
#20002=ADVANCED_FACE('',(#2145),#18997,.T.);
#20003=ADVANCED_FACE('',(#2146,#689),#18998,.T.);
#20004=ADVANCED_FACE('',(#2147),#18999,.T.);
#20005=ADVANCED_FACE('',(#2148),#19000,.F.);
#20006=ADVANCED_FACE('',(#2149,#690),#19001,.F.);
#20007=ADVANCED_FACE('',(#2150),#19002,.F.);
#20008=ADVANCED_FACE('',(#2151,#691,#692,#693,#694,#695,#696,#697,#698),
#19003,.F.);
#20009=ADVANCED_FACE('',(#2152,#699,#700,#701,#702,#703,#704,#705,#706),
#19004,.F.);
#20010=ADVANCED_FACE('',(#2153),#19005,.T.);
#20011=ADVANCED_FACE('',(#2154),#19006,.T.);
#20012=ADVANCED_FACE('',(#2155),#19007,.T.);
#20013=ADVANCED_FACE('',(#2156),#19008,.T.);
#20014=ADVANCED_FACE('',(#2157,#707,#708,#709,#710,#711,#712,#713,#714,
#715,#716,#717,#718,#719,#720,#721,#722),#19009,.T.);
#20015=ADVANCED_FACE('',(#2158),#19010,.T.);
#20016=ADVANCED_FACE('',(#2159),#1168,.T.);
#20017=ADVANCED_FACE('',(#2160),#1169,.F.);
#20018=ADVANCED_FACE('',(#2161),#1170,.T.);
#20019=ADVANCED_FACE('',(#2162),#19011,.T.);
#20020=ADVANCED_FACE('',(#2163),#1171,.T.);
#20021=ADVANCED_FACE('',(#2164),#1172,.F.);
#20022=ADVANCED_FACE('',(#2165),#1173,.T.);
#20023=ADVANCED_FACE('',(#2166),#19012,.T.);
#20024=ADVANCED_FACE('',(#2167),#1174,.F.);
#20025=ADVANCED_FACE('',(#2168),#19013,.T.);
#20026=ADVANCED_FACE('',(#2169),#1175,.F.);
#20027=ADVANCED_FACE('',(#2170),#19014,.T.);
#20028=ADVANCED_FACE('',(#2171),#1176,.T.);
#20029=ADVANCED_FACE('',(#2172),#19015,.T.);
#20030=ADVANCED_FACE('',(#2173),#19016,.T.);
#20031=ADVANCED_FACE('',(#2174),#19017,.T.);
#20032=ADVANCED_FACE('',(#2175),#19018,.F.);
#20033=ADVANCED_FACE('',(#2176),#1177,.T.);
#20034=ADVANCED_FACE('',(#2177),#1178,.F.);
#20035=ADVANCED_FACE('',(#2178),#1179,.T.);
#20036=ADVANCED_FACE('',(#2179),#19019,.F.);
#20037=ADVANCED_FACE('',(#2180),#1180,.T.);
#20038=ADVANCED_FACE('',(#2181),#1181,.F.);
#20039=ADVANCED_FACE('',(#2182),#1182,.T.);
#20040=ADVANCED_FACE('',(#2183),#19020,.F.);
#20041=ADVANCED_FACE('',(#2184),#1183,.F.);
#20042=ADVANCED_FACE('',(#2185),#19021,.F.);
#20043=ADVANCED_FACE('',(#2186),#1184,.F.);
#20044=ADVANCED_FACE('',(#2187),#19022,.F.);
#20045=ADVANCED_FACE('',(#2188),#1185,.T.);
#20046=ADVANCED_FACE('',(#2189),#19023,.F.);
#20047=ADVANCED_FACE('',(#2190),#19024,.F.);
#20048=ADVANCED_FACE('',(#2191),#19025,.F.);
#20049=ADVANCED_FACE('',(#2192),#19026,.F.);
#20050=ADVANCED_FACE('',(#2193),#19027,.F.);
#20051=ADVANCED_FACE('',(#2194),#1186,.F.);
#20052=ADVANCED_FACE('',(#2195),#19028,.T.);
#20053=ADVANCED_FACE('',(#2196),#19029,.T.);
#20054=ADVANCED_FACE('',(#2197),#19030,.T.);
#20055=ADVANCED_FACE('',(#2198),#19031,.T.);
#20056=ADVANCED_FACE('',(#2199,#723),#19032,.T.);
#20057=ADVANCED_FACE('',(#2200,#724),#19033,.F.);
#20058=ADVANCED_FACE('',(#2201),#1187,.F.);
#20059=ADVANCED_FACE('',(#2202),#19034,.T.);
#20060=ADVANCED_FACE('',(#2203),#19035,.T.);
#20061=ADVANCED_FACE('',(#2204),#19036,.T.);
#20062=ADVANCED_FACE('',(#2205),#19037,.T.);
#20063=ADVANCED_FACE('',(#2206,#725),#19038,.T.);
#20064=ADVANCED_FACE('',(#2207,#726),#19039,.F.);
#20065=ADVANCED_FACE('',(#2208),#1188,.F.);
#20066=ADVANCED_FACE('',(#2209),#19040,.T.);
#20067=ADVANCED_FACE('',(#2210),#19041,.T.);
#20068=ADVANCED_FACE('',(#2211),#19042,.T.);
#20069=ADVANCED_FACE('',(#2212),#19043,.T.);
#20070=ADVANCED_FACE('',(#2213,#727),#19044,.T.);
#20071=ADVANCED_FACE('',(#2214,#728),#19045,.F.);
#20072=ADVANCED_FACE('',(#2215),#19046,.F.);
#20073=ADVANCED_FACE('',(#2216),#1189,.T.);
#20074=ADVANCED_FACE('',(#2217),#1190,.F.);
#20075=ADVANCED_FACE('',(#2218),#1191,.T.);
#20076=ADVANCED_FACE('',(#2219),#19047,.F.);
#20077=ADVANCED_FACE('',(#2220),#1192,.T.);
#20078=ADVANCED_FACE('',(#2221),#1193,.F.);
#20079=ADVANCED_FACE('',(#2222),#1194,.T.);
#20080=ADVANCED_FACE('',(#2223),#19048,.F.);
#20081=ADVANCED_FACE('',(#2224),#1195,.F.);
#20082=ADVANCED_FACE('',(#2225),#19049,.F.);
#20083=ADVANCED_FACE('',(#2226),#1196,.F.);
#20084=ADVANCED_FACE('',(#2227),#19050,.F.);
#20085=ADVANCED_FACE('',(#2228),#1197,.T.);
#20086=ADVANCED_FACE('',(#2229),#19051,.F.);
#20087=ADVANCED_FACE('',(#2230),#19052,.F.);
#20088=ADVANCED_FACE('',(#2231),#19053,.F.);
#20089=ADVANCED_FACE('',(#2232),#19054,.T.);
#20090=ADVANCED_FACE('',(#2233),#1198,.T.);
#20091=ADVANCED_FACE('',(#2234),#1199,.F.);
#20092=ADVANCED_FACE('',(#2235),#1200,.T.);
#20093=ADVANCED_FACE('',(#2236),#19055,.T.);
#20094=ADVANCED_FACE('',(#2237),#1201,.T.);
#20095=ADVANCED_FACE('',(#2238),#1202,.F.);
#20096=ADVANCED_FACE('',(#2239),#1203,.T.);
#20097=ADVANCED_FACE('',(#2240),#19056,.T.);
#20098=ADVANCED_FACE('',(#2241),#1204,.F.);
#20099=ADVANCED_FACE('',(#2242),#19057,.T.);
#20100=ADVANCED_FACE('',(#2243),#1205,.F.);
#20101=ADVANCED_FACE('',(#2244),#19058,.T.);
#20102=ADVANCED_FACE('',(#2245),#1206,.T.);
#20103=ADVANCED_FACE('',(#2246),#19059,.T.);
#20104=ADVANCED_FACE('',(#2247),#19060,.T.);
#20105=ADVANCED_FACE('',(#2248),#19061,.T.);
#20106=ADVANCED_FACE('',(#2249),#19062,.T.);
#20107=ADVANCED_FACE('',(#2250),#19063,.T.);
#20108=CLOSED_SHELL('',(#19064,#19065,#19066,#19067,#19068,#19069,#19070,
#19071,#19072,#19073,#19074,#19075,#19076,#19077,#19078,#19079,#19080,#19081,
#19082,#19083,#19084,#19085,#19086,#19087,#19088,#19089,#19090,#19091,#19092,
#19093,#19094,#19095,#19096,#19097,#19098,#19099,#19100,#19101));
#20109=CLOSED_SHELL('',(#19102,#19103,#19104,#19105,#19106,#19107,#19108,
#19109,#19110,#19111,#19112,#19113,#19114,#19115,#19116,#19117,#19118,#19119,
#19120,#19121,#19122,#19123,#19124,#19125,#19126,#19127,#19128,#19129,#19130,
#19131,#19132,#19133,#19134,#19135,#19136,#19137,#19138,#19139,#19140,#19141,
#19142,#19143,#19144,#19145,#19146,#19147,#19148,#19149,#19150,#19151));
#20110=CLOSED_SHELL('',(#19152,#19153,#19154,#19155,#19156,#19157,#19158,
#19159,#19160,#19161,#19162,#19163,#19164,#19165,#19166,#19167,#19168,#19169,
#19170,#19171,#19172,#19173,#19174,#19175,#19176,#19177,#19178,#19179,#19180,
#19181,#19182,#19183,#19184,#19185,#19186,#19187,#19188,#19189));
#20111=CLOSED_SHELL('',(#19190,#19191,#19192,#19193,#19194,#19195,#19196,
#19197,#19198,#19199,#19200,#19201,#19202,#19203,#19204,#19205,#19206,#19207,
#19208,#19209,#19210,#19211,#19212,#19213,#19214,#19215,#19216,#19217,#19218,
#19219,#19220,#19221,#19222,#19223,#19224,#19225,#19226,#19227));
#20112=CLOSED_SHELL('',(#19228,#19229,#19230,#19231,#19232,#19233,#19234,
#19235,#19236,#19237,#19238,#19239,#19240,#19241,#19242,#19243,#19244,#19245,
#19246,#19247,#19248,#19249,#19250,#19251,#19252,#19253,#19254,#19255,#19256,
#19257,#19258,#19259,#19260,#19261,#19262,#19263,#19264,#19265,#19266,#19267,
#19268,#19269,#19270,#19271,#19272,#19273,#19274,#19275,#19276,#19277));
#20113=CLOSED_SHELL('',(#19278,#19279,#19280,#19281,#19282,#19283,#19284,
#19285,#19286,#19287,#19288,#19289,#19290,#19291,#19292,#19293,#19294,#19295,
#19296,#19297,#19298,#19299,#19300,#19301,#19302,#19303,#19304,#19305,#19306,
#19307,#19308,#19309,#19310,#19311,#19312,#19313,#19314,#19315));
#20114=CLOSED_SHELL('',(#19316,#19317,#19318,#19319,#19320,#19321,#19322,
#19323,#19324,#19325,#19326,#19327,#19328,#19329,#19330,#19331,#19332,#19333,
#19334,#19335,#19336,#19337,#19338,#19339,#19340,#19341,#19342,#19343,#19344,
#19345,#19346,#19347,#19348,#19349,#19350,#19351,#19352,#19353,#19354,#19355,
#19356,#19357,#19358,#19359,#19360,#19361,#19362,#19363,#19364,#19365,#19366,
#19367,#19368,#19369,#19370,#19371,#19372,#19373));
#20115=CLOSED_SHELL('',(#19374));
#20116=CLOSED_SHELL('',(#19375,#19376,#19377,#19378,#19379,#19380,#19381,
#19382,#19383,#19384,#19385,#19386));
#20117=CLOSED_SHELL('',(#19387,#19388,#19389,#19390,#19391,#19392,#19393,
#19394,#19395,#19396));
#20118=CLOSED_SHELL('',(#19397));
#20119=CLOSED_SHELL('',(#19398));
#20120=CLOSED_SHELL('',(#19399));
#20121=CLOSED_SHELL('',(#19400));
#20122=CLOSED_SHELL('',(#19401));
#20123=CLOSED_SHELL('',(#19402));
#20124=CLOSED_SHELL('',(#19403));
#20125=CLOSED_SHELL('',(#19404,#19405,#19406,#19407,#19408,#19409,#19410,
#19411,#19412,#19413,#19414,#19415,#19416,#19417,#19418,#19419,#19420,#19421,
#19422,#19423,#19424,#19425,#19426,#19427,#19428,#19429,#19430,#19431,#19432,
#19433,#19434,#19435,#19436,#19437,#19438,#19439,#19440,#19441,#19442,#19443,
#19444,#19445,#19446,#19447,#19448,#19449,#19450,#19451,#19452,#19453,#19454,
#19455,#19456,#19457,#19458,#19459,#19460,#19461,#19462));
#20126=CLOSED_SHELL('',(#19463,#19464,#19465,#19466,#19467,#19468,#19469,
#19470,#19471,#19472,#19473,#19474,#19475,#19476,#19477,#19478,#19479,#19480,
#19481,#19482,#19483,#19484,#19485,#19486,#19487,#19488,#19489,#19490,#19491,
#19492,#19493,#19494,#19495,#19496,#19497,#19498,#19499,#19500,#19501,#19502,
#19503,#19504,#19505,#19506,#19507,#19508,#19509,#19510,#19511,#19512,#19513,
#19514,#19515,#19516,#19517,#19518,#19519,#19520,#19521,#19522,#19523,#19524,
#19525,#19526,#19527,#19528,#19529,#19530,#19531,#19532,#19533,#19534,#19535,
#19536,#19537,#19538,#19539,#19540,#19541,#19542,#19543,#19544,#19545,#19546,
#19547,#19548,#19549,#19550,#19551,#19552,#19553,#19554,#19555,#19556,#19557,
#19558,#19559,#19560,#19561,#19562,#19563,#19564,#19565,#19566,#19567,#19568,
#19569,#19570,#19571,#19572,#19573,#19574,#19575,#19576,#19577,#19578,#19579,
#19580,#19581,#19582,#19583,#19584,#19585,#19586,#19587,#19588,#19589,#19590,
#19591,#19592,#19593,#19594,#19595,#19596,#19597,#19598,#19599,#19600,#19601,
#19602,#19603,#19604,#19605,#19606,#19607,#19608,#19609,#19610,#19611,#19612,
#19613,#19614,#19615,#19616,#19617,#19618,#19619,#19620,#19621,#19622,#19623,
#19624,#19625,#19626,#19627,#19628,#19629,#19630,#19631,#19632,#19633,#19634,
#19635,#19636,#19637,#19638,#19639,#19640,#19641,#19642,#19643,#19644,#19645,
#19646,#19647,#19648,#19649,#19650,#19651,#19652,#19653,#19654,#19655,#19656,
#19657,#19658,#19659,#19660,#19661,#19662,#19663,#19664,#19665,#19666,#19667,
#19668,#19669,#19670,#19671,#19672,#19673,#19674,#19675,#19676,#19677,#19678,
#19679,#19680,#19681,#19682,#19683,#19684,#19685,#19686,#19687,#19688,#19689,
#19690,#19691,#19692,#19693,#19694,#19695,#19696,#19697,#19698,#19699,#19700,
#19701,#19702,#19703,#19704,#19705,#19706,#19707,#19708,#19709,#19710,#19711,
#19712,#19713,#19714,#19715,#19716,#19717,#19718,#19719,#19720,#19721,#19722,
#19723,#19724,#19725,#19726,#19727,#19728,#19729,#19730,#19731,#19732,#19733,
#19734,#19735,#19736,#19737,#19738,#19739,#19740,#19741));
#20127=CLOSED_SHELL('',(#19742,#19743,#19744,#19745,#19746,#19747,#19748,
#19749,#19750,#19751,#19752,#19753,#19754,#19755,#19756,#19757,#19758,#19759,
#19760,#19761,#19762,#19763,#19764,#19765,#19766,#19767,#19768,#19769,#19770,
#19771,#19772,#19773,#19774,#19775,#19776,#19777,#19778,#19779,#19780,#19781,
#19782,#19783,#19784,#19785,#19786,#19787,#19788,#19789,#19790,#19791,#19792,
#19793,#19794,#19795,#19796,#19797,#19798,#19799,#19800,#19801,#19802,#19803,
#19804,#19805,#19806,#19807,#19808,#19809,#19810,#19811,#19812,#19813,#19814,
#19815,#19816,#19817,#19818,#19819,#19820,#19821,#19822,#19823,#19824,#19825,
#19826,#19827,#19828,#19829,#19830,#19831,#19832,#19833,#19834,#19835,#19836,
#19837,#19838,#19839,#19840,#19841,#19842,#19843,#19844,#19845,#19846,#19847,
#19848,#19849,#19850,#19851,#19852,#19853,#19854,#19855,#19856,#19857,#19858,
#19859,#19860,#19861,#19862,#19863,#19864,#19865,#19866,#19867,#19868,#19869,
#19870,#19871,#19872,#19873,#19874,#19875,#19876,#19877,#19878,#19879,#19880,
#19881,#19882,#19883,#19884,#19885,#19886,#19887,#19888,#19889,#19890,#19891,
#19892,#19893,#19894,#19895,#19896,#19897,#19898,#19899,#19900,#19901,#19902,
#19903,#19904,#19905,#19906,#19907,#19908,#19909,#19910,#19911,#19912,#19913,
#19914,#19915,#19916,#19917,#19918,#19919,#19920,#19921,#19922,#19923,#19924,
#19925,#19926,#19927,#19928,#19929,#19930,#19931,#19932,#19933,#19934,#19935,
#19936,#19937,#19938,#19939,#19940,#19941,#19942,#19943,#19944,#19945,#19946,
#19947,#19948,#19949,#19950,#19951,#19952,#19953,#19954,#19955,#19956,#19957,
#19958,#19959,#19960,#19961,#19962,#19963,#19964,#19965,#19966,#19967,#19968,
#19969,#19970,#19971,#19972,#19973,#19974,#19975,#19976,#19977,#19978,#19979,
#19980));
#20128=CLOSED_SHELL('',(#19981,#19982,#19983,#19984,#19985,#19986,#19987,
#19988,#19989,#19990,#19991,#19992,#19993,#19994,#19995,#19996,#19997,#19998,
#19999,#20000,#20001,#20002,#20003,#20004,#20005,#20006,#20007,#20008,#20009,
#20010,#20011,#20012,#20013,#20014));
#20129=CLOSED_SHELL('',(#20015,#20016,#20017,#20018,#20019,#20020,#20021,
#20022,#20023,#20024,#20025,#20026,#20027,#20028,#20029,#20030,#20031,#20032,
#20033,#20034,#20035,#20036,#20037,#20038,#20039,#20040,#20041,#20042,#20043,
#20044,#20045,#20046,#20047,#20048,#20049,#20050));
#20130=CLOSED_SHELL('',(#20051,#20052,#20053,#20054,#20055,#20056,#20057));
#20131=CLOSED_SHELL('',(#20058,#20059,#20060,#20061,#20062,#20063,#20064));
#20132=CLOSED_SHELL('',(#20065,#20066,#20067,#20068,#20069,#20070,#20071));
#20133=CLOSED_SHELL('',(#20072,#20073,#20074,#20075,#20076,#20077,#20078,
#20079,#20080,#20081,#20082,#20083,#20084,#20085,#20086,#20087,#20088,#20089,
#20090,#20091,#20092,#20093,#20094,#20095,#20096,#20097,#20098,#20099,#20100,
#20101,#20102,#20103,#20104,#20105,#20106,#20107));
#20134=DERIVED_UNIT_ELEMENT(#20156,1.);
#20135=DERIVED_UNIT_ELEMENT(#48371,-3.);
#20136=DERIVED_UNIT_ELEMENT(#20156,1.);
#20137=DERIVED_UNIT_ELEMENT(#48371,-3.);
#20138=DERIVED_UNIT_ELEMENT(#20156,1.);
#20139=DERIVED_UNIT_ELEMENT(#48371,-3.);
#20140=DERIVED_UNIT_ELEMENT(#20156,1.);
#20141=DERIVED_UNIT_ELEMENT(#48371,-3.);
#20142=DERIVED_UNIT_ELEMENT(#20156,1.);
#20143=DERIVED_UNIT_ELEMENT(#48371,-3.);
#20144=DERIVED_UNIT_ELEMENT(#20156,1.);
#20145=DERIVED_UNIT_ELEMENT(#48371,-3.);
#20146=DERIVED_UNIT_ELEMENT(#20156,1.);
#20147=DERIVED_UNIT_ELEMENT(#48371,-3.);
#20148=DERIVED_UNIT_ELEMENT(#20156,1.);
#20149=DERIVED_UNIT_ELEMENT(#48371,-3.);
#20150=DERIVED_UNIT_ELEMENT(#20156,1.);
#20151=DERIVED_UNIT_ELEMENT(#48371,-3.);
#20152=DERIVED_UNIT_ELEMENT(#20156,1.);
#20153=DERIVED_UNIT_ELEMENT(#48371,-3.);
#20154=DERIVED_UNIT_ELEMENT(#20156,1.);
#20155=DERIVED_UNIT_ELEMENT(#48371,-3.);
#20156=(
MASS_UNIT()
NAMED_UNIT(*)
SI_UNIT(.KILO.,.GRAM.)
);
#20157=DERIVED_UNIT((#20134,#20135));
#20158=DERIVED_UNIT((#20136,#20137));
#20159=DERIVED_UNIT((#20138,#20139));
#20160=DERIVED_UNIT((#20140,#20141));
#20161=DERIVED_UNIT((#20142,#20143));
#20162=DERIVED_UNIT((#20144,#20145));
#20163=DERIVED_UNIT((#20146,#20147));
#20164=DERIVED_UNIT((#20148,#20149));
#20165=DERIVED_UNIT((#20150,#20151));
#20166=DERIVED_UNIT((#20152,#20153));
#20167=DERIVED_UNIT((#20154,#20155));
#20168=MEASURE_REPRESENTATION_ITEM('density measure',
POSITIVE_RATIO_MEASURE(7850.),#20157);
#20169=MEASURE_REPRESENTATION_ITEM('density measure',
POSITIVE_RATIO_MEASURE(7850.),#20158);
#20170=MEASURE_REPRESENTATION_ITEM('density measure',
POSITIVE_RATIO_MEASURE(7850.),#20159);
#20171=MEASURE_REPRESENTATION_ITEM('density measure',
POSITIVE_RATIO_MEASURE(7850.),#20160);
#20172=MEASURE_REPRESENTATION_ITEM('density measure',
POSITIVE_RATIO_MEASURE(7850.),#20161);
#20173=MEASURE_REPRESENTATION_ITEM('density measure',
POSITIVE_RATIO_MEASURE(7850.),#20162);
#20174=MEASURE_REPRESENTATION_ITEM('density measure',
POSITIVE_RATIO_MEASURE(7850.),#20163);
#20175=MEASURE_REPRESENTATION_ITEM('density measure',
POSITIVE_RATIO_MEASURE(7850.),#20164);
#20176=MEASURE_REPRESENTATION_ITEM('density measure',
POSITIVE_RATIO_MEASURE(7850.),#20165);
#20177=MEASURE_REPRESENTATION_ITEM('density measure',
POSITIVE_RATIO_MEASURE(7850.),#20166);
#20178=MEASURE_REPRESENTATION_ITEM('density measure',
POSITIVE_RATIO_MEASURE(7850.),#20167);
#20179=PROPERTY_DEFINITION_REPRESENTATION(#20234,#20201);
#20180=PROPERTY_DEFINITION_REPRESENTATION(#20235,#20202);
#20181=PROPERTY_DEFINITION_REPRESENTATION(#20236,#20203);
#20182=PROPERTY_DEFINITION_REPRESENTATION(#20237,#20204);
#20183=PROPERTY_DEFINITION_REPRESENTATION(#20238,#20205);
#20184=PROPERTY_DEFINITION_REPRESENTATION(#20239,#20206);
#20185=PROPERTY_DEFINITION_REPRESENTATION(#20240,#20207);
#20186=PROPERTY_DEFINITION_REPRESENTATION(#20241,#20208);
#20187=PROPERTY_DEFINITION_REPRESENTATION(#20242,#20209);
#20188=PROPERTY_DEFINITION_REPRESENTATION(#20243,#20210);
#20189=PROPERTY_DEFINITION_REPRESENTATION(#20244,#20211);
#20190=PROPERTY_DEFINITION_REPRESENTATION(#20245,#20212);
#20191=PROPERTY_DEFINITION_REPRESENTATION(#20246,#20213);
#20192=PROPERTY_DEFINITION_REPRESENTATION(#20247,#20214);
#20193=PROPERTY_DEFINITION_REPRESENTATION(#20248,#20215);
#20194=PROPERTY_DEFINITION_REPRESENTATION(#20249,#20216);
#20195=PROPERTY_DEFINITION_REPRESENTATION(#20250,#20217);
#20196=PROPERTY_DEFINITION_REPRESENTATION(#20251,#20218);
#20197=PROPERTY_DEFINITION_REPRESENTATION(#20252,#20219);
#20198=PROPERTY_DEFINITION_REPRESENTATION(#20253,#20220);
#20199=PROPERTY_DEFINITION_REPRESENTATION(#20254,#20221);
#20200=PROPERTY_DEFINITION_REPRESENTATION(#20255,#20222);
#20201=REPRESENTATION('material name',(#20223),#48358);
#20202=REPRESENTATION('density',(#20168),#48358);
#20203=REPRESENTATION('material name',(#20224),#48359);
#20204=REPRESENTATION('density',(#20169),#48359);
#20205=REPRESENTATION('material name',(#20225),#48360);
#20206=REPRESENTATION('density',(#20170),#48360);
#20207=REPRESENTATION('material name',(#20226),#48361);
#20208=REPRESENTATION('density',(#20171),#48361);
#20209=REPRESENTATION('material name',(#20227),#48362);
#20210=REPRESENTATION('density',(#20172),#48362);
#20211=REPRESENTATION('material name',(#20228),#48363);
#20212=REPRESENTATION('density',(#20173),#48363);
#20213=REPRESENTATION('material name',(#20229),#48364);
#20214=REPRESENTATION('density',(#20174),#48364);
#20215=REPRESENTATION('material name',(#20230),#48365);
#20216=REPRESENTATION('density',(#20175),#48365);
#20217=REPRESENTATION('material name',(#20231),#48366);
#20218=REPRESENTATION('density',(#20176),#48366);
#20219=REPRESENTATION('material name',(#20232),#48367);
#20220=REPRESENTATION('density',(#20177),#48367);
#20221=REPRESENTATION('material name',(#20233),#48368);
#20222=REPRESENTATION('density',(#20178),#48368);
#20223=DESCRIPTIVE_REPRESENTATION_ITEM('Steel','Steel');
#20224=DESCRIPTIVE_REPRESENTATION_ITEM('Steel','Steel');
#20225=DESCRIPTIVE_REPRESENTATION_ITEM('Steel','Steel');
#20226=DESCRIPTIVE_REPRESENTATION_ITEM('Steel','Steel');
#20227=DESCRIPTIVE_REPRESENTATION_ITEM('Steel','Steel');
#20228=DESCRIPTIVE_REPRESENTATION_ITEM('Steel','Steel');
#20229=DESCRIPTIVE_REPRESENTATION_ITEM('Steel','Steel');
#20230=DESCRIPTIVE_REPRESENTATION_ITEM('Steel','Steel');
#20231=DESCRIPTIVE_REPRESENTATION_ITEM('Steel','Steel');
#20232=DESCRIPTIVE_REPRESENTATION_ITEM('Steel','Steel');
#20233=DESCRIPTIVE_REPRESENTATION_ITEM('Steel','Steel');
#20234=PROPERTY_DEFINITION('material property','material name',#48426);
#20235=PROPERTY_DEFINITION('material property','density of part',#48426);
#20236=PROPERTY_DEFINITION('material property','material name',#48427);
#20237=PROPERTY_DEFINITION('material property','density of part',#48427);
#20238=PROPERTY_DEFINITION('material property','material name',#48428);
#20239=PROPERTY_DEFINITION('material property','density of part',#48428);
#20240=PROPERTY_DEFINITION('material property','material name',#48429);
#20241=PROPERTY_DEFINITION('material property','density of part',#48429);
#20242=PROPERTY_DEFINITION('material property','material name',#48430);
#20243=PROPERTY_DEFINITION('material property','density of part',#48430);
#20244=PROPERTY_DEFINITION('material property','material name',#48431);
#20245=PROPERTY_DEFINITION('material property','density of part',#48431);
#20246=PROPERTY_DEFINITION('material property','material name',#48432);
#20247=PROPERTY_DEFINITION('material property','density of part',#48432);
#20248=PROPERTY_DEFINITION('material property','material name',#48433);
#20249=PROPERTY_DEFINITION('material property','density of part',#48433);
#20250=PROPERTY_DEFINITION('material property','material name',#48434);
#20251=PROPERTY_DEFINITION('material property','density of part',#48434);
#20252=PROPERTY_DEFINITION('material property','material name',#48435);
#20253=PROPERTY_DEFINITION('material property','density of part',#48435);
#20254=PROPERTY_DEFINITION('material property','material name',#48436);
#20255=PROPERTY_DEFINITION('material property','density of part',#48436);
#20256=AXIS2_PLACEMENT_3D('',#27147,#21926,#21927);
#20257=AXIS2_PLACEMENT_3D('',#27148,#21928,#21929);
#20258=AXIS2_PLACEMENT_3D('',#27149,#21930,#21931);
#20259=AXIS2_PLACEMENT_3D('',#27160,#21936,#21937);
#20260=AXIS2_PLACEMENT_3D('',#27164,#21939,#21940);
#20261=AXIS2_PLACEMENT_3D('',#27168,#21942,#21943);
#20262=AXIS2_PLACEMENT_3D('',#27170,#21944,#21945);
#20263=AXIS2_PLACEMENT_3D('',#27172,#21946,#21947);
#20264=AXIS2_PLACEMENT_3D('',#27176,#21949,#21950);
#20265=AXIS2_PLACEMENT_3D('',#27178,#21951,#21952);
#20266=AXIS2_PLACEMENT_3D('',#27180,#21953,#21954);
#20267=AXIS2_PLACEMENT_3D('',#27188,#21958,#21959);
#20268=AXIS2_PLACEMENT_3D('',#27190,#21960,#21961);
#20269=AXIS2_PLACEMENT_3D('',#27192,#21962,#21963);
#20270=AXIS2_PLACEMENT_3D('',#27196,#21965,#21966);
#20271=AXIS2_PLACEMENT_3D('',#27198,#21967,#21968);
#20272=AXIS2_PLACEMENT_3D('',#27200,#21969,#21970);
#20273=AXIS2_PLACEMENT_3D('',#27204,#21972,#21973);
#20274=AXIS2_PLACEMENT_3D('',#27208,#21975,#21976);
#20275=AXIS2_PLACEMENT_3D('',#27222,#21984,#21985);
#20276=AXIS2_PLACEMENT_3D('',#27228,#21989,#21990);
#20277=AXIS2_PLACEMENT_3D('',#27230,#21991,#21992);
#20278=AXIS2_PLACEMENT_3D('',#27232,#21994,#21995);
#20279=AXIS2_PLACEMENT_3D('',#27234,#21996,#21997);
#20280=AXIS2_PLACEMENT_3D('',#27236,#21999,#22000);
#20281=AXIS2_PLACEMENT_3D('',#27238,#22001,#22002);
#20282=AXIS2_PLACEMENT_3D('',#27240,#22004,#22005);
#20283=AXIS2_PLACEMENT_3D('',#27244,#22008,#22009);
#20284=AXIS2_PLACEMENT_3D('',#27246,#22010,#22011);
#20285=AXIS2_PLACEMENT_3D('',#27248,#22013,#22014);
#20286=AXIS2_PLACEMENT_3D('',#27250,#22015,#22016);
#20287=AXIS2_PLACEMENT_3D('',#27252,#22018,#22019);
#20288=AXIS2_PLACEMENT_3D('',#27254,#22020,#22021);
#20289=AXIS2_PLACEMENT_3D('',#27256,#22023,#22024);
#20290=AXIS2_PLACEMENT_3D('',#27260,#22027,#22028);
#20291=AXIS2_PLACEMENT_3D('',#27262,#22029,#22030);
#20292=AXIS2_PLACEMENT_3D('',#27264,#22032,#22033);
#20293=AXIS2_PLACEMENT_3D('',#27268,#22036,#22037);
#20294=AXIS2_PLACEMENT_3D('',#27270,#22038,#22039);
#20295=AXIS2_PLACEMENT_3D('',#27272,#22041,#22042);
#20296=AXIS2_PLACEMENT_3D('',#27276,#22045,#22046);
#20297=AXIS2_PLACEMENT_3D('',#27280,#22049,#22050);
#20298=AXIS2_PLACEMENT_3D('',#27284,#22053,#22054);
#20299=AXIS2_PLACEMENT_3D('',#27288,#22057,#22058);
#20300=AXIS2_PLACEMENT_3D('',#27294,#22062,#22063);
#20301=AXIS2_PLACEMENT_3D('',#27298,#22066,#22067);
#20302=AXIS2_PLACEMENT_3D('',#27302,#22070,#22071);
#20303=AXIS2_PLACEMENT_3D('',#27306,#22074,#22075);
#20304=AXIS2_PLACEMENT_3D('',#27308,#22076,#22077);
#20305=AXIS2_PLACEMENT_3D('',#27310,#22079,#22080);
#20306=AXIS2_PLACEMENT_3D('',#27314,#22083,#22084);
#20307=AXIS2_PLACEMENT_3D('',#27318,#22087,#22088);
#20308=AXIS2_PLACEMENT_3D('',#27320,#22090,#22091);
#20309=AXIS2_PLACEMENT_3D('',#27324,#22094,#22095);
#20310=AXIS2_PLACEMENT_3D('',#27328,#22098,#22099);
#20311=AXIS2_PLACEMENT_3D('',#27332,#22102,#22103);
#20312=AXIS2_PLACEMENT_3D('',#27335,#22105,#22106);
#20313=AXIS2_PLACEMENT_3D('',#27336,#22107,#22108);
#20314=AXIS2_PLACEMENT_3D('',#27339,#22110,#22111);
#20315=AXIS2_PLACEMENT_3D('',#27340,#22112,#22113);
#20316=AXIS2_PLACEMENT_3D('',#27343,#22115,#22116);
#20317=AXIS2_PLACEMENT_3D('',#27344,#22117,#22118);
#20318=AXIS2_PLACEMENT_3D('',#27348,#22121,#22122);
#20319=AXIS2_PLACEMENT_3D('',#27351,#22124,#22125);
#20320=AXIS2_PLACEMENT_3D('',#27352,#22126,#22127);
#20321=AXIS2_PLACEMENT_3D('',#27355,#22129,#22130);
#20322=AXIS2_PLACEMENT_3D('',#27356,#22131,#22132);
#20323=AXIS2_PLACEMENT_3D('',#27359,#22134,#22135);
#20324=AXIS2_PLACEMENT_3D('',#27360,#22136,#22137);
#20325=AXIS2_PLACEMENT_3D('',#27364,#22140,#22141);
#20326=AXIS2_PLACEMENT_3D('',#27365,#22142,#22143);
#20327=AXIS2_PLACEMENT_3D('',#27366,#22144,#22145);
#20328=AXIS2_PLACEMENT_3D('',#27367,#22146,#22147);
#20329=AXIS2_PLACEMENT_3D('',#27376,#22152,#22153);
#20330=AXIS2_PLACEMENT_3D('',#27378,#22154,#22155);
#20331=AXIS2_PLACEMENT_3D('',#27381,#22157,#22158);
#20332=AXIS2_PLACEMENT_3D('',#27382,#22159,#22160);
#20333=AXIS2_PLACEMENT_3D('',#27384,#22161,#22162);
#20334=AXIS2_PLACEMENT_3D('',#27387,#22164,#22165);
#20335=AXIS2_PLACEMENT_3D('',#27388,#22166,#22167);
#20336=AXIS2_PLACEMENT_3D('',#27390,#22168,#22169);
#20337=AXIS2_PLACEMENT_3D('',#27393,#22171,#22172);
#20338=AXIS2_PLACEMENT_3D('',#27394,#22173,#22174);
#20339=AXIS2_PLACEMENT_3D('',#27400,#22178,#22179);
#20340=AXIS2_PLACEMENT_3D('',#27402,#22180,#22181);
#20341=AXIS2_PLACEMENT_3D('',#27405,#22183,#22184);
#20342=AXIS2_PLACEMENT_3D('',#27406,#22185,#22186);
#20343=AXIS2_PLACEMENT_3D('',#27408,#22187,#22188);
#20344=AXIS2_PLACEMENT_3D('',#27411,#22190,#22191);
#20345=AXIS2_PLACEMENT_3D('',#27412,#22192,#22193);
#20346=AXIS2_PLACEMENT_3D('',#27425,#22199,#22200);
#20347=AXIS2_PLACEMENT_3D('',#27429,#22202,#22203);
#20348=AXIS2_PLACEMENT_3D('',#27432,#22205,#22206);
#20349=AXIS2_PLACEMENT_3D('',#27438,#22209,#22210);
#20350=AXIS2_PLACEMENT_3D('',#27440,#22211,#22212);
#20351=AXIS2_PLACEMENT_3D('',#27442,#22213,#22214);
#20352=AXIS2_PLACEMENT_3D('',#27446,#22216,#22217);
#20353=AXIS2_PLACEMENT_3D('',#27448,#22218,#22219);
#20354=AXIS2_PLACEMENT_3D('',#27450,#22220,#22221);
#20355=AXIS2_PLACEMENT_3D('',#27454,#22223,#22224);
#20356=AXIS2_PLACEMENT_3D('',#27458,#22226,#22227);
#20357=AXIS2_PLACEMENT_3D('',#27476,#22236,#22237);
#20358=AXIS2_PLACEMENT_3D('',#27480,#22239,#22240);
#20359=AXIS2_PLACEMENT_3D('',#27486,#22244,#22245);
#20360=AXIS2_PLACEMENT_3D('',#27492,#22249,#22250);
#20361=AXIS2_PLACEMENT_3D('',#27496,#22253,#22254);
#20362=AXIS2_PLACEMENT_3D('',#27500,#22257,#22258);
#20363=AXIS2_PLACEMENT_3D('',#27505,#22261,#22262);
#20364=AXIS2_PLACEMENT_3D('',#27507,#22263,#22264);
#20365=AXIS2_PLACEMENT_3D('',#27508,#22265,#22266);
#20366=AXIS2_PLACEMENT_3D('',#27511,#22268,#22269);
#20367=AXIS2_PLACEMENT_3D('',#27512,#22270,#22271);
#20368=AXIS2_PLACEMENT_3D('',#27516,#22274,#22275);
#20369=AXIS2_PLACEMENT_3D('',#27518,#22276,#22277);
#20370=AXIS2_PLACEMENT_3D('',#27536,#22286,#22287);
#20371=AXIS2_PLACEMENT_3D('',#27540,#22289,#22290);
#20372=AXIS2_PLACEMENT_3D('',#27544,#22292,#22293);
#20373=AXIS2_PLACEMENT_3D('',#27546,#22294,#22295);
#20374=AXIS2_PLACEMENT_3D('',#27548,#22296,#22297);
#20375=AXIS2_PLACEMENT_3D('',#27552,#22299,#22300);
#20376=AXIS2_PLACEMENT_3D('',#27554,#22301,#22302);
#20377=AXIS2_PLACEMENT_3D('',#27556,#22303,#22304);
#20378=AXIS2_PLACEMENT_3D('',#27561,#22307,#22308);
#20379=AXIS2_PLACEMENT_3D('',#27565,#22310,#22311);
#20380=AXIS2_PLACEMENT_3D('',#27569,#22313,#22314);
#20381=AXIS2_PLACEMENT_3D('',#27577,#22319,#22320);
#20382=AXIS2_PLACEMENT_3D('',#27580,#22323,#22324);
#20383=AXIS2_PLACEMENT_3D('',#27582,#22326,#22327);
#20384=AXIS2_PLACEMENT_3D('',#27584,#22329,#22330);
#20385=AXIS2_PLACEMENT_3D('',#27587,#22332,#22333);
#20386=AXIS2_PLACEMENT_3D('',#27589,#22334,#22335);
#20387=AXIS2_PLACEMENT_3D('',#27590,#22336,#22337);
#20388=AXIS2_PLACEMENT_3D('',#27591,#22338,#22339);
#20389=AXIS2_PLACEMENT_3D('',#27594,#22341,#22342);
#20390=AXIS2_PLACEMENT_3D('',#27595,#22343,#22344);
#20391=AXIS2_PLACEMENT_3D('',#27598,#22346,#22347);
#20392=AXIS2_PLACEMENT_3D('',#27599,#22348,#22349);
#20393=AXIS2_PLACEMENT_3D('',#27602,#22351,#22352);
#20394=AXIS2_PLACEMENT_3D('',#27603,#22353,#22354);
#20395=AXIS2_PLACEMENT_3D('',#27606,#22356,#22357);
#20396=AXIS2_PLACEMENT_3D('',#27607,#22358,#22359);
#20397=AXIS2_PLACEMENT_3D('',#27609,#22361,#22362);
#20398=AXIS2_PLACEMENT_3D('',#27611,#22364,#22365);
#20399=AXIS2_PLACEMENT_3D('',#27613,#22367,#22368);
#20400=AXIS2_PLACEMENT_3D('',#27615,#22370,#22371);
#20401=AXIS2_PLACEMENT_3D('',#27617,#22373,#22374);
#20402=AXIS2_PLACEMENT_3D('',#27619,#22376,#22377);
#20403=AXIS2_PLACEMENT_3D('',#27621,#22379,#22380);
#20404=AXIS2_PLACEMENT_3D('',#27623,#22382,#22383);
#20405=AXIS2_PLACEMENT_3D('',#27624,#22384,#22385);
#20406=AXIS2_PLACEMENT_3D('',#27626,#22387,#22388);
#20407=AXIS2_PLACEMENT_3D('',#27628,#22390,#22391);
#20408=AXIS2_PLACEMENT_3D('',#27630,#22393,#22394);
#20409=AXIS2_PLACEMENT_3D('',#27632,#22396,#22397);
#20410=AXIS2_PLACEMENT_3D('',#27634,#22399,#22400);
#20411=AXIS2_PLACEMENT_3D('',#27636,#22402,#22403);
#20412=AXIS2_PLACEMENT_3D('',#27638,#22405,#22406);
#20413=AXIS2_PLACEMENT_3D('',#27640,#22408,#22409);
#20414=AXIS2_PLACEMENT_3D('',#27642,#22411,#22412);
#20415=AXIS2_PLACEMENT_3D('',#27644,#22414,#22415);
#20416=AXIS2_PLACEMENT_3D('',#27646,#22417,#22418);
#20417=AXIS2_PLACEMENT_3D('',#27648,#22420,#22421);
#20418=AXIS2_PLACEMENT_3D('',#27650,#22423,#22424);
#20419=AXIS2_PLACEMENT_3D('',#27652,#22426,#22427);
#20420=AXIS2_PLACEMENT_3D('',#27654,#22429,#22430);
#20421=AXIS2_PLACEMENT_3D('',#27656,#22432,#22433);
#20422=AXIS2_PLACEMENT_3D('',#27657,#22434,#22435);
#20423=AXIS2_PLACEMENT_3D('',#27660,#22436,#22437);
#20424=AXIS2_PLACEMENT_3D('',#27664,#22439,#22440);
#20425=AXIS2_PLACEMENT_3D('',#27666,#22442,#22443);
#20426=AXIS2_PLACEMENT_3D('',#27672,#22447,#22448);
#20427=AXIS2_PLACEMENT_3D('',#27674,#22449,#22450);
#20428=AXIS2_PLACEMENT_3D('',#27677,#22452,#22453);
#20429=AXIS2_PLACEMENT_3D('',#27678,#22454,#22455);
#20430=AXIS2_PLACEMENT_3D('',#27684,#22459,#22460);
#20431=AXIS2_PLACEMENT_3D('',#27686,#22461,#22462);
#20432=AXIS2_PLACEMENT_3D('',#27689,#22464,#22465);
#20433=AXIS2_PLACEMENT_3D('',#27690,#22466,#22467);
#20434=AXIS2_PLACEMENT_3D('',#27696,#22471,#22472);
#20435=AXIS2_PLACEMENT_3D('',#27702,#22476,#22477);
#20436=AXIS2_PLACEMENT_3D('',#27708,#22481,#22482);
#20437=AXIS2_PLACEMENT_3D('',#27717,#22487,#22488);
#20438=AXIS2_PLACEMENT_3D('',#27723,#22492,#22493);
#20439=AXIS2_PLACEMENT_3D('',#27729,#22497,#22498);
#20440=AXIS2_PLACEMENT_3D('',#27735,#22502,#22503);
#20441=AXIS2_PLACEMENT_3D('',#27741,#22507,#22508);
#20442=AXIS2_PLACEMENT_3D('',#27747,#22512,#22513);
#20443=AXIS2_PLACEMENT_3D('',#27753,#22517,#22518);
#20444=AXIS2_PLACEMENT_3D('',#27755,#22519,#22520);
#20445=AXIS2_PLACEMENT_3D('',#27758,#22522,#22523);
#20446=AXIS2_PLACEMENT_3D('',#27759,#22524,#22525);
#20447=AXIS2_PLACEMENT_3D('',#27762,#22526,#22527);
#20448=AXIS2_PLACEMENT_3D('',#27766,#22529,#22530);
#20449=AXIS2_PLACEMENT_3D('',#27768,#22531,#22532);
#20450=AXIS2_PLACEMENT_3D('',#27770,#22533,#22534);
#20451=AXIS2_PLACEMENT_3D('',#27774,#22536,#22537);
#20452=AXIS2_PLACEMENT_3D('',#27776,#22538,#22539);
#20453=AXIS2_PLACEMENT_3D('',#27778,#22540,#22541);
#20454=AXIS2_PLACEMENT_3D('',#27786,#22545,#22546);
#20455=AXIS2_PLACEMENT_3D('',#27788,#22547,#22548);
#20456=AXIS2_PLACEMENT_3D('',#27790,#22549,#22550);
#20457=AXIS2_PLACEMENT_3D('',#27794,#22552,#22553);
#20458=AXIS2_PLACEMENT_3D('',#27795,#22554,#22555);
#20459=AXIS2_PLACEMENT_3D('',#27798,#22558,#22559);
#20460=AXIS2_PLACEMENT_3D('',#27800,#22561,#22562);
#20461=AXIS2_PLACEMENT_3D('',#27804,#22565,#22566);
#20462=AXIS2_PLACEMENT_3D('',#27806,#22567,#22568);
#20463=AXIS2_PLACEMENT_3D('',#27808,#22570,#22571);
#20464=AXIS2_PLACEMENT_3D('',#27812,#22574,#22575);
#20465=AXIS2_PLACEMENT_3D('',#27814,#22576,#22577);
#20466=AXIS2_PLACEMENT_3D('',#27816,#22579,#22580);
#20467=AXIS2_PLACEMENT_3D('',#27818,#22581,#22582);
#20468=AXIS2_PLACEMENT_3D('',#27820,#22584,#22585);
#20469=AXIS2_PLACEMENT_3D('',#27822,#22586,#22587);
#20470=AXIS2_PLACEMENT_3D('',#27824,#22589,#22590);
#20471=AXIS2_PLACEMENT_3D('',#27828,#22593,#22594);
#20472=AXIS2_PLACEMENT_3D('',#27830,#22595,#22596);
#20473=AXIS2_PLACEMENT_3D('',#27832,#22598,#22599);
#20474=AXIS2_PLACEMENT_3D('',#27834,#22600,#22601);
#20475=AXIS2_PLACEMENT_3D('',#27836,#22603,#22604);
#20476=AXIS2_PLACEMENT_3D('',#27838,#22605,#22606);
#20477=AXIS2_PLACEMENT_3D('',#27840,#22608,#22609);
#20478=AXIS2_PLACEMENT_3D('',#27844,#22612,#22613);
#20479=AXIS2_PLACEMENT_3D('',#27848,#22616,#22617);
#20480=AXIS2_PLACEMENT_3D('',#27852,#22620,#22621);
#20481=AXIS2_PLACEMENT_3D('',#27854,#22622,#22623);
#20482=AXIS2_PLACEMENT_3D('',#27856,#22625,#22626);
#20483=AXIS2_PLACEMENT_3D('',#27858,#22627,#22628);
#20484=AXIS2_PLACEMENT_3D('',#27860,#22630,#22631);
#20485=AXIS2_PLACEMENT_3D('',#27862,#22632,#22633);
#20486=AXIS2_PLACEMENT_3D('',#27864,#22635,#22636);
#20487=AXIS2_PLACEMENT_3D('',#27868,#22639,#22640);
#20488=AXIS2_PLACEMENT_3D('',#27870,#22641,#22642);
#20489=AXIS2_PLACEMENT_3D('',#27872,#22644,#22645);
#20490=AXIS2_PLACEMENT_3D('',#27873,#22646,#22647);
#20491=AXIS2_PLACEMENT_3D('',#27874,#22648,#22649);
#20492=AXIS2_PLACEMENT_3D('',#27875,#22650,#22651);
#20493=AXIS2_PLACEMENT_3D('',#27876,#22652,#22653);
#20494=AXIS2_PLACEMENT_3D('',#27895,#22662,#22663);
#20495=AXIS2_PLACEMENT_3D('',#27899,#22665,#22666);
#20496=AXIS2_PLACEMENT_3D('',#27903,#22668,#22669);
#20497=AXIS2_PLACEMENT_3D('',#27905,#22670,#22671);
#20498=AXIS2_PLACEMENT_3D('',#27907,#22672,#22673);
#20499=AXIS2_PLACEMENT_3D('',#27911,#22675,#22676);
#20500=AXIS2_PLACEMENT_3D('',#27913,#22677,#22678);
#20501=AXIS2_PLACEMENT_3D('',#27915,#22679,#22680);
#20502=AXIS2_PLACEMENT_3D('',#27923,#22684,#22685);
#20503=AXIS2_PLACEMENT_3D('',#27925,#22686,#22687);
#20504=AXIS2_PLACEMENT_3D('',#27927,#22688,#22689);
#20505=AXIS2_PLACEMENT_3D('',#27931,#22691,#22692);
#20506=AXIS2_PLACEMENT_3D('',#27933,#22693,#22694);
#20507=AXIS2_PLACEMENT_3D('',#27935,#22695,#22696);
#20508=AXIS2_PLACEMENT_3D('',#27939,#22698,#22699);
#20509=AXIS2_PLACEMENT_3D('',#27943,#22701,#22702);
#20510=AXIS2_PLACEMENT_3D('',#27949,#22706,#22707);
#20511=AXIS2_PLACEMENT_3D('',#27955,#22711,#22712);
#20512=AXIS2_PLACEMENT_3D('',#27958,#22714,#22715);
#20513=AXIS2_PLACEMENT_3D('',#27959,#22716,#22717);
#20514=AXIS2_PLACEMENT_3D('',#27962,#22719,#22720);
#20515=AXIS2_PLACEMENT_3D('',#27963,#22721,#22722);
#20516=AXIS2_PLACEMENT_3D('',#27966,#22724,#22725);
#20517=AXIS2_PLACEMENT_3D('',#27967,#22726,#22727);
#20518=AXIS2_PLACEMENT_3D('',#27971,#22730,#22731);
#20519=AXIS2_PLACEMENT_3D('',#27974,#22733,#22734);
#20520=AXIS2_PLACEMENT_3D('',#27975,#22735,#22736);
#20521=AXIS2_PLACEMENT_3D('',#27978,#22738,#22739);
#20522=AXIS2_PLACEMENT_3D('',#27979,#22740,#22741);
#20523=AXIS2_PLACEMENT_3D('',#27982,#22743,#22744);
#20524=AXIS2_PLACEMENT_3D('',#27983,#22745,#22746);
#20525=AXIS2_PLACEMENT_3D('',#27987,#22749,#22750);
#20526=AXIS2_PLACEMENT_3D('',#27990,#22752,#22753);
#20527=AXIS2_PLACEMENT_3D('',#27991,#22754,#22755);
#20528=AXIS2_PLACEMENT_3D('',#27995,#22758,#22759);
#20529=AXIS2_PLACEMENT_3D('',#27998,#22761,#22762);
#20530=AXIS2_PLACEMENT_3D('',#27999,#22763,#22764);
#20531=AXIS2_PLACEMENT_3D('',#28003,#22767,#22768);
#20532=AXIS2_PLACEMENT_3D('',#28007,#22771,#22772);
#20533=AXIS2_PLACEMENT_3D('',#28011,#22775,#22776);
#20534=AXIS2_PLACEMENT_3D('',#28015,#22779,#22780);
#20535=AXIS2_PLACEMENT_3D('',#28021,#22784,#22785);
#20536=AXIS2_PLACEMENT_3D('',#28025,#22788,#22789);
#20537=AXIS2_PLACEMENT_3D('',#28029,#22792,#22793);
#20538=AXIS2_PLACEMENT_3D('',#28033,#22796,#22797);
#20539=AXIS2_PLACEMENT_3D('',#28036,#22799,#22800);
#20540=AXIS2_PLACEMENT_3D('',#28037,#22801,#22802);
#20541=AXIS2_PLACEMENT_3D('',#28041,#22805,#22806);
#20542=AXIS2_PLACEMENT_3D('',#28045,#22809,#22810);
#20543=AXIS2_PLACEMENT_3D('',#28047,#22812,#22813);
#20544=AXIS2_PLACEMENT_3D('',#28051,#22816,#22817);
#20545=AXIS2_PLACEMENT_3D('',#28055,#22820,#22821);
#20546=AXIS2_PLACEMENT_3D('',#28059,#22824,#22825);
#20547=AXIS2_PLACEMENT_3D('',#28061,#22826,#22827);
#20548=AXIS2_PLACEMENT_3D('',#28063,#22829,#22830);
#20549=AXIS2_PLACEMENT_3D('',#28065,#22831,#22832);
#20550=AXIS2_PLACEMENT_3D('',#28067,#22834,#22835);
#20551=AXIS2_PLACEMENT_3D('',#28069,#22836,#22837);
#20552=AXIS2_PLACEMENT_3D('',#28071,#22839,#22840);
#20553=AXIS2_PLACEMENT_3D('',#28075,#22843,#22844);
#20554=AXIS2_PLACEMENT_3D('',#28077,#22845,#22846);
#20555=AXIS2_PLACEMENT_3D('',#28079,#22848,#22849);
#20556=AXIS2_PLACEMENT_3D('',#28081,#22850,#22851);
#20557=AXIS2_PLACEMENT_3D('',#28083,#22853,#22854);
#20558=AXIS2_PLACEMENT_3D('',#28085,#22855,#22856);
#20559=AXIS2_PLACEMENT_3D('',#28087,#22858,#22859);
#20560=AXIS2_PLACEMENT_3D('',#28091,#22862,#22863);
#20561=AXIS2_PLACEMENT_3D('',#28092,#22864,#22865);
#20562=AXIS2_PLACEMENT_3D('',#28093,#22866,#22867);
#20563=AXIS2_PLACEMENT_3D('',#28094,#22868,#22869);
#20564=AXIS2_PLACEMENT_3D('',#28103,#22874,#22875);
#20565=AXIS2_PLACEMENT_3D('',#28105,#22876,#22877);
#20566=AXIS2_PLACEMENT_3D('',#28107,#22878,#22879);
#20567=AXIS2_PLACEMENT_3D('',#28109,#22881,#22882);
#20568=AXIS2_PLACEMENT_3D('',#28111,#22883,#22884);
#20569=AXIS2_PLACEMENT_3D('',#28113,#22885,#22886);
#20570=AXIS2_PLACEMENT_3D('',#28115,#22888,#22889);
#20571=AXIS2_PLACEMENT_3D('',#28117,#22890,#22891);
#20572=AXIS2_PLACEMENT_3D('',#28119,#22892,#22893);
#20573=AXIS2_PLACEMENT_3D('',#28121,#22895,#22896);
#20574=AXIS2_PLACEMENT_3D('',#28127,#22900,#22901);
#20575=AXIS2_PLACEMENT_3D('',#28129,#22902,#22903);
#20576=AXIS2_PLACEMENT_3D('',#28131,#22904,#22905);
#20577=AXIS2_PLACEMENT_3D('',#28133,#22907,#22908);
#20578=AXIS2_PLACEMENT_3D('',#28135,#22909,#22910);
#20579=AXIS2_PLACEMENT_3D('',#28137,#22911,#22912);
#20580=AXIS2_PLACEMENT_3D('',#28139,#22914,#22915);
#20581=AXIS2_PLACEMENT_3D('',#28150,#22920,#22921);
#20582=AXIS2_PLACEMENT_3D('',#28154,#22923,#22924);
#20583=AXIS2_PLACEMENT_3D('',#28172,#22933,#22934);
#20584=AXIS2_PLACEMENT_3D('',#28176,#22936,#22937);
#20585=AXIS2_PLACEMENT_3D('',#28180,#22939,#22940);
#20586=AXIS2_PLACEMENT_3D('',#28182,#22941,#22942);
#20587=AXIS2_PLACEMENT_3D('',#28184,#22943,#22944);
#20588=AXIS2_PLACEMENT_3D('',#28188,#22946,#22947);
#20589=AXIS2_PLACEMENT_3D('',#28190,#22948,#22949);
#20590=AXIS2_PLACEMENT_3D('',#28192,#22950,#22951);
#20591=AXIS2_PLACEMENT_3D('',#28197,#22954,#22955);
#20592=AXIS2_PLACEMENT_3D('',#28201,#22957,#22958);
#20593=AXIS2_PLACEMENT_3D('',#28205,#22960,#22961);
#20594=AXIS2_PLACEMENT_3D('',#28213,#22966,#22967);
#20595=AXIS2_PLACEMENT_3D('',#28219,#22971,#22972);
#20596=AXIS2_PLACEMENT_3D('',#28223,#22975,#22976);
#20597=AXIS2_PLACEMENT_3D('',#28227,#22979,#22980);
#20598=AXIS2_PLACEMENT_3D('',#28232,#22983,#22984);
#20599=AXIS2_PLACEMENT_3D('',#28234,#22985,#22986);
#20600=AXIS2_PLACEMENT_3D('',#28235,#22987,#22988);
#20601=AXIS2_PLACEMENT_3D('',#28238,#22990,#22991);
#20602=AXIS2_PLACEMENT_3D('',#28239,#22992,#22993);
#20603=AXIS2_PLACEMENT_3D('',#28243,#22996,#22997);
#20604=AXIS2_PLACEMENT_3D('',#28253,#23002,#23003);
#20605=AXIS2_PLACEMENT_3D('',#28257,#23005,#23006);
#20606=AXIS2_PLACEMENT_3D('',#28260,#23008,#23009);
#20607=AXIS2_PLACEMENT_3D('',#28266,#23012,#23013);
#20608=AXIS2_PLACEMENT_3D('',#28268,#23014,#23015);
#20609=AXIS2_PLACEMENT_3D('',#28270,#23016,#23017);
#20610=AXIS2_PLACEMENT_3D('',#28274,#23019,#23020);
#20611=AXIS2_PLACEMENT_3D('',#28276,#23021,#23022);
#20612=AXIS2_PLACEMENT_3D('',#28278,#23023,#23024);
#20613=AXIS2_PLACEMENT_3D('',#28282,#23026,#23027);
#20614=AXIS2_PLACEMENT_3D('',#28286,#23029,#23030);
#20615=AXIS2_PLACEMENT_3D('',#28303,#23039,#23040);
#20616=AXIS2_PLACEMENT_3D('',#28304,#23041,#23042);
#20617=AXIS2_PLACEMENT_3D('',#28307,#23045,#23046);
#20618=AXIS2_PLACEMENT_3D('',#28309,#23048,#23049);
#20619=AXIS2_PLACEMENT_3D('',#28311,#23051,#23052);
#20620=AXIS2_PLACEMENT_3D('',#28314,#23054,#23055);
#20621=AXIS2_PLACEMENT_3D('',#28316,#23056,#23057);
#20622=AXIS2_PLACEMENT_3D('',#28317,#23058,#23059);
#20623=AXIS2_PLACEMENT_3D('',#28318,#23060,#23061);
#20624=AXIS2_PLACEMENT_3D('',#28321,#23063,#23064);
#20625=AXIS2_PLACEMENT_3D('',#28322,#23065,#23066);
#20626=AXIS2_PLACEMENT_3D('',#28325,#23068,#23069);
#20627=AXIS2_PLACEMENT_3D('',#28326,#23070,#23071);
#20628=AXIS2_PLACEMENT_3D('',#28329,#23073,#23074);
#20629=AXIS2_PLACEMENT_3D('',#28330,#23075,#23076);
#20630=AXIS2_PLACEMENT_3D('',#28333,#23078,#23079);
#20631=AXIS2_PLACEMENT_3D('',#28334,#23080,#23081);
#20632=AXIS2_PLACEMENT_3D('',#28336,#23083,#23084);
#20633=AXIS2_PLACEMENT_3D('',#28338,#23086,#23087);
#20634=AXIS2_PLACEMENT_3D('',#28340,#23089,#23090);
#20635=AXIS2_PLACEMENT_3D('',#28342,#23092,#23093);
#20636=AXIS2_PLACEMENT_3D('',#28344,#23095,#23096);
#20637=AXIS2_PLACEMENT_3D('',#28346,#23098,#23099);
#20638=AXIS2_PLACEMENT_3D('',#28348,#23101,#23102);
#20639=AXIS2_PLACEMENT_3D('',#28350,#23104,#23105);
#20640=AXIS2_PLACEMENT_3D('',#28351,#23106,#23107);
#20641=AXIS2_PLACEMENT_3D('',#28353,#23109,#23110);
#20642=AXIS2_PLACEMENT_3D('',#28355,#23112,#23113);
#20643=AXIS2_PLACEMENT_3D('',#28357,#23115,#23116);
#20644=AXIS2_PLACEMENT_3D('',#28359,#23118,#23119);
#20645=AXIS2_PLACEMENT_3D('',#28361,#23121,#23122);
#20646=AXIS2_PLACEMENT_3D('',#28363,#23124,#23125);
#20647=AXIS2_PLACEMENT_3D('',#28365,#23127,#23128);
#20648=AXIS2_PLACEMENT_3D('',#28367,#23130,#23131);
#20649=AXIS2_PLACEMENT_3D('',#28369,#23133,#23134);
#20650=AXIS2_PLACEMENT_3D('',#28371,#23136,#23137);
#20651=AXIS2_PLACEMENT_3D('',#28373,#23139,#23140);
#20652=AXIS2_PLACEMENT_3D('',#28375,#23142,#23143);
#20653=AXIS2_PLACEMENT_3D('',#28377,#23145,#23146);
#20654=AXIS2_PLACEMENT_3D('',#28379,#23148,#23149);
#20655=AXIS2_PLACEMENT_3D('',#28381,#23151,#23152);
#20656=AXIS2_PLACEMENT_3D('',#28383,#23154,#23155);
#20657=AXIS2_PLACEMENT_3D('',#28384,#23156,#23157);
#20658=AXIS2_PLACEMENT_3D('',#28387,#23158,#23159);
#20659=AXIS2_PLACEMENT_3D('',#28391,#23161,#23162);
#20660=AXIS2_PLACEMENT_3D('',#28393,#23164,#23165);
#20661=AXIS2_PLACEMENT_3D('',#28399,#23169,#23170);
#20662=AXIS2_PLACEMENT_3D('',#28401,#23171,#23172);
#20663=AXIS2_PLACEMENT_3D('',#28403,#23173,#23174);
#20664=AXIS2_PLACEMENT_3D('',#28405,#23176,#23177);
#20665=AXIS2_PLACEMENT_3D('',#28411,#23181,#23182);
#20666=AXIS2_PLACEMENT_3D('',#28413,#23183,#23184);
#20667=AXIS2_PLACEMENT_3D('',#28415,#23185,#23186);
#20668=AXIS2_PLACEMENT_3D('',#28417,#23188,#23189);
#20669=AXIS2_PLACEMENT_3D('',#28423,#23193,#23194);
#20670=AXIS2_PLACEMENT_3D('',#28429,#23198,#23199);
#20671=AXIS2_PLACEMENT_3D('',#28435,#23203,#23204);
#20672=AXIS2_PLACEMENT_3D('',#28444,#23209,#23210);
#20673=AXIS2_PLACEMENT_3D('',#28450,#23214,#23215);
#20674=AXIS2_PLACEMENT_3D('',#28456,#23219,#23220);
#20675=AXIS2_PLACEMENT_3D('',#28462,#23224,#23225);
#20676=AXIS2_PLACEMENT_3D('',#28468,#23229,#23230);
#20677=AXIS2_PLACEMENT_3D('',#28474,#23234,#23235);
#20678=AXIS2_PLACEMENT_3D('',#28480,#23239,#23240);
#20679=AXIS2_PLACEMENT_3D('',#28482,#23241,#23242);
#20680=AXIS2_PLACEMENT_3D('',#28484,#23243,#23244);
#20681=AXIS2_PLACEMENT_3D('',#28486,#23246,#23247);
#20682=AXIS2_PLACEMENT_3D('',#28489,#23248,#23249);
#20683=AXIS2_PLACEMENT_3D('',#28493,#23252,#23253);
#20684=AXIS2_PLACEMENT_3D('',#28495,#23254,#23255);
#20685=AXIS2_PLACEMENT_3D('',#28499,#23257,#23258);
#20686=AXIS2_PLACEMENT_3D('',#28501,#23259,#23260);
#20687=AXIS2_PLACEMENT_3D('',#28503,#23261,#23262);
#20688=AXIS2_PLACEMENT_3D('',#28511,#23266,#23267);
#20689=AXIS2_PLACEMENT_3D('',#28513,#23268,#23269);
#20690=AXIS2_PLACEMENT_3D('',#28515,#23270,#23271);
#20691=AXIS2_PLACEMENT_3D('',#28519,#23273,#23274);
#20692=AXIS2_PLACEMENT_3D('',#28521,#23275,#23276);
#20693=AXIS2_PLACEMENT_3D('',#28523,#23277,#23278);
#20694=AXIS2_PLACEMENT_3D('',#28525,#23280,#23281);
#20695=AXIS2_PLACEMENT_3D('',#28527,#23283,#23284);
#20696=AXIS2_PLACEMENT_3D('',#28531,#23287,#23288);
#20697=AXIS2_PLACEMENT_3D('',#28533,#23289,#23290);
#20698=AXIS2_PLACEMENT_3D('',#28535,#23292,#23293);
#20699=AXIS2_PLACEMENT_3D('',#28539,#23296,#23297);
#20700=AXIS2_PLACEMENT_3D('',#28541,#23298,#23299);
#20701=AXIS2_PLACEMENT_3D('',#28543,#23301,#23302);
#20702=AXIS2_PLACEMENT_3D('',#28545,#23303,#23304);
#20703=AXIS2_PLACEMENT_3D('',#28547,#23306,#23307);
#20704=AXIS2_PLACEMENT_3D('',#28549,#23308,#23309);
#20705=AXIS2_PLACEMENT_3D('',#28551,#23311,#23312);
#20706=AXIS2_PLACEMENT_3D('',#28555,#23315,#23316);
#20707=AXIS2_PLACEMENT_3D('',#28557,#23317,#23318);
#20708=AXIS2_PLACEMENT_3D('',#28559,#23320,#23321);
#20709=AXIS2_PLACEMENT_3D('',#28561,#23322,#23323);
#20710=AXIS2_PLACEMENT_3D('',#28563,#23325,#23326);
#20711=AXIS2_PLACEMENT_3D('',#28565,#23327,#23328);
#20712=AXIS2_PLACEMENT_3D('',#28567,#23330,#23331);
#20713=AXIS2_PLACEMENT_3D('',#28571,#23334,#23335);
#20714=AXIS2_PLACEMENT_3D('',#28575,#23338,#23339);
#20715=AXIS2_PLACEMENT_3D('',#28579,#23342,#23343);
#20716=AXIS2_PLACEMENT_3D('',#28581,#23344,#23345);
#20717=AXIS2_PLACEMENT_3D('',#28583,#23347,#23348);
#20718=AXIS2_PLACEMENT_3D('',#28585,#23349,#23350);
#20719=AXIS2_PLACEMENT_3D('',#28587,#23352,#23353);
#20720=AXIS2_PLACEMENT_3D('',#28589,#23354,#23355);
#20721=AXIS2_PLACEMENT_3D('',#28591,#23357,#23358);
#20722=AXIS2_PLACEMENT_3D('',#28595,#23361,#23362);
#20723=AXIS2_PLACEMENT_3D('',#28597,#23363,#23364);
#20724=AXIS2_PLACEMENT_3D('',#28599,#23366,#23367);
#20725=AXIS2_PLACEMENT_3D('',#28600,#23368,#23369);
#20726=AXIS2_PLACEMENT_3D('',#28601,#23370,#23371);
#20727=AXIS2_PLACEMENT_3D('',#28602,#23372,#23373);
#20728=AXIS2_PLACEMENT_3D('',#28603,#23374,#23375);
#20729=AXIS2_PLACEMENT_3D('',#28605,#23376,#23377);
#20730=AXIS2_PLACEMENT_3D('',#28608,#23379,#23380);
#20731=AXIS2_PLACEMENT_3D('',#28609,#23381,#23382);
#20732=AXIS2_PLACEMENT_3D('',#28611,#23383,#23384);
#20733=AXIS2_PLACEMENT_3D('',#28612,#23385,#23386);
#20734=AXIS2_PLACEMENT_3D('',#28613,#23387,#23388);
#20735=AXIS2_PLACEMENT_3D('',#28615,#23389,#23390);
#20736=AXIS2_PLACEMENT_3D('',#28617,#23391,#23392);
#20737=AXIS2_PLACEMENT_3D('',#28618,#23393,#23394);
#20738=AXIS2_PLACEMENT_3D('',#28619,#23395,#23396);
#20739=AXIS2_PLACEMENT_3D('',#28621,#23397,#23398);
#20740=AXIS2_PLACEMENT_3D('',#28623,#23400,#23401);
#20741=AXIS2_PLACEMENT_3D('',#28626,#23402,#23403);
#20742=AXIS2_PLACEMENT_3D('',#28628,#23404,#23405);
#20743=AXIS2_PLACEMENT_3D('',#28630,#23406,#23407);
#20744=AXIS2_PLACEMENT_3D('',#28632,#23408,#23409);
#20745=AXIS2_PLACEMENT_3D('',#28634,#23410,#23411);
#20746=AXIS2_PLACEMENT_3D('',#28636,#23412,#23413);
#20747=AXIS2_PLACEMENT_3D('',#28638,#23414,#23415);
#20748=AXIS2_PLACEMENT_3D('',#28640,#23416,#23417);
#20749=AXIS2_PLACEMENT_3D('',#28642,#23418,#23419);
#20750=AXIS2_PLACEMENT_3D('',#28643,#23420,#23421);
#20751=AXIS2_PLACEMENT_3D('',#28645,#23422,#23423);
#20752=AXIS2_PLACEMENT_3D('',#28647,#23424,#23425);
#20753=AXIS2_PLACEMENT_3D('',#28649,#23426,#23427);
#20754=AXIS2_PLACEMENT_3D('',#28651,#23428,#23429);
#20755=AXIS2_PLACEMENT_3D('',#28653,#23430,#23431);
#20756=AXIS2_PLACEMENT_3D('',#28655,#23432,#23433);
#20757=AXIS2_PLACEMENT_3D('',#28657,#23434,#23435);
#20758=AXIS2_PLACEMENT_3D('',#28658,#23436,#23437);
#20759=AXIS2_PLACEMENT_3D('',#28659,#23438,#23439);
#20760=AXIS2_PLACEMENT_3D('',#28661,#23440,#23441);
#20761=AXIS2_PLACEMENT_3D('',#28664,#23443,#23444);
#20762=AXIS2_PLACEMENT_3D('',#28665,#23445,#23446);
#20763=AXIS2_PLACEMENT_3D('',#28667,#23447,#23448);
#20764=AXIS2_PLACEMENT_3D('',#28668,#23449,#23450);
#20765=AXIS2_PLACEMENT_3D('',#28669,#23451,#23452);
#20766=AXIS2_PLACEMENT_3D('',#28671,#23453,#23454);
#20767=AXIS2_PLACEMENT_3D('',#28673,#23455,#23456);
#20768=AXIS2_PLACEMENT_3D('',#28675,#23457,#23458);
#20769=AXIS2_PLACEMENT_3D('',#28677,#23459,#23460);
#20770=AXIS2_PLACEMENT_3D('',#28679,#23461,#23462);
#20771=AXIS2_PLACEMENT_3D('',#28681,#23463,#23464);
#20772=AXIS2_PLACEMENT_3D('',#28683,#23465,#23466);
#20773=AXIS2_PLACEMENT_3D('',#28685,#23467,#23468);
#20774=AXIS2_PLACEMENT_3D('',#28687,#23469,#23470);
#20775=AXIS2_PLACEMENT_3D('',#28689,#23471,#23472);
#20776=AXIS2_PLACEMENT_3D('',#28691,#23473,#23474);
#20777=AXIS2_PLACEMENT_3D('',#28693,#23475,#23476);
#20778=AXIS2_PLACEMENT_3D('',#28695,#23477,#23478);
#20779=AXIS2_PLACEMENT_3D('',#28697,#23479,#23480);
#20780=AXIS2_PLACEMENT_3D('',#28699,#23481,#23482);
#20781=AXIS2_PLACEMENT_3D('',#28701,#23483,#23484);
#20782=AXIS2_PLACEMENT_3D('',#28703,#23485,#23486);
#20783=AXIS2_PLACEMENT_3D('',#28705,#23487,#23488);
#20784=AXIS2_PLACEMENT_3D('',#28707,#23489,#23490);
#20785=AXIS2_PLACEMENT_3D('',#28709,#23491,#23492);
#20786=AXIS2_PLACEMENT_3D('',#28711,#23493,#23494);
#20787=AXIS2_PLACEMENT_3D('',#28713,#23495,#23496);
#20788=AXIS2_PLACEMENT_3D('',#28715,#23497,#23498);
#20789=AXIS2_PLACEMENT_3D('',#28717,#23499,#23500);
#20790=AXIS2_PLACEMENT_3D('',#28719,#23501,#23502);
#20791=AXIS2_PLACEMENT_3D('',#28721,#23503,#23504);
#20792=AXIS2_PLACEMENT_3D('',#28723,#23505,#23506);
#20793=AXIS2_PLACEMENT_3D('',#28725,#23507,#23508);
#20794=AXIS2_PLACEMENT_3D('',#28727,#23509,#23510);
#20795=AXIS2_PLACEMENT_3D('',#28729,#23511,#23512);
#20796=AXIS2_PLACEMENT_3D('',#28731,#23513,#23514);
#20797=AXIS2_PLACEMENT_3D('',#28733,#23515,#23516);
#20798=AXIS2_PLACEMENT_3D('',#28735,#23517,#23518);
#20799=AXIS2_PLACEMENT_3D('',#28736,#23519,#23520);
#20800=AXIS2_PLACEMENT_3D('',#28737,#23521,#23522);
#20801=AXIS2_PLACEMENT_3D('',#28741,#23524,#23525);
#20802=AXIS2_PLACEMENT_3D('',#28743,#23527,#23528);
#20803=AXIS2_PLACEMENT_3D('',#28746,#23529,#23530);
#20804=AXIS2_PLACEMENT_3D('',#28749,#23533,#23534);
#20805=AXIS2_PLACEMENT_3D('',#28753,#23536,#23537);
#20806=AXIS2_PLACEMENT_3D('',#28755,#23539,#23540);
#20807=AXIS2_PLACEMENT_3D('',#28759,#23542,#23543);
#20808=AXIS2_PLACEMENT_3D('',#28761,#23545,#23546);
#20809=AXIS2_PLACEMENT_3D('',#28765,#23548,#23549);
#20810=AXIS2_PLACEMENT_3D('',#28767,#23551,#23552);
#20811=AXIS2_PLACEMENT_3D('',#28771,#23554,#23555);
#20812=AXIS2_PLACEMENT_3D('',#28773,#23557,#23558);
#20813=AXIS2_PLACEMENT_3D('',#28777,#23560,#23561);
#20814=AXIS2_PLACEMENT_3D('',#28779,#23563,#23564);
#20815=AXIS2_PLACEMENT_3D('',#28782,#23565,#23566);
#20816=AXIS2_PLACEMENT_3D('',#28785,#23569,#23570);
#20817=AXIS2_PLACEMENT_3D('',#28789,#23572,#23573);
#20818=AXIS2_PLACEMENT_3D('',#28791,#23575,#23576);
#20819=AXIS2_PLACEMENT_3D('',#28794,#23577,#23578);
#20820=AXIS2_PLACEMENT_3D('',#28797,#23581,#23582);
#20821=AXIS2_PLACEMENT_3D('',#28801,#23584,#23585);
#20822=AXIS2_PLACEMENT_3D('',#28803,#23587,#23588);
#20823=AXIS2_PLACEMENT_3D('',#28807,#23590,#23591);
#20824=AXIS2_PLACEMENT_3D('',#28809,#23593,#23594);
#20825=AXIS2_PLACEMENT_3D('',#28813,#23596,#23597);
#20826=AXIS2_PLACEMENT_3D('',#28815,#23599,#23600);
#20827=AXIS2_PLACEMENT_3D('',#28819,#23602,#23603);
#20828=AXIS2_PLACEMENT_3D('',#28821,#23605,#23606);
#20829=AXIS2_PLACEMENT_3D('',#28825,#23608,#23609);
#20830=AXIS2_PLACEMENT_3D('',#28827,#23611,#23612);
#20831=AXIS2_PLACEMENT_3D('',#28830,#23613,#23614);
#20832=AXIS2_PLACEMENT_3D('',#28833,#23617,#23618);
#20833=AXIS2_PLACEMENT_3D('',#28836,#23621,#23622);
#20834=AXIS2_PLACEMENT_3D('',#28839,#23625,#23626);
#20835=AXIS2_PLACEMENT_3D('',#28842,#23629,#23630);
#20836=AXIS2_PLACEMENT_3D('',#28845,#23633,#23634);
#20837=AXIS2_PLACEMENT_3D('',#28848,#23637,#23638);
#20838=AXIS2_PLACEMENT_3D('',#28851,#23641,#23642);
#20839=AXIS2_PLACEMENT_3D('',#28854,#23645,#23646);
#20840=AXIS2_PLACEMENT_3D('',#28857,#23649,#23650);
#20841=AXIS2_PLACEMENT_3D('',#28858,#23651,#23652);
#20842=AXIS2_PLACEMENT_3D('',#28859,#23653,#23654);
#20843=AXIS2_PLACEMENT_3D('',#28861,#23656,#23657);
#20844=AXIS2_PLACEMENT_3D('',#28863,#23659,#23660);
#20845=AXIS2_PLACEMENT_3D('',#28864,#23661,#23662);
#20846=AXIS2_PLACEMENT_3D('',#28866,#23664,#23665);
#20847=AXIS2_PLACEMENT_3D('',#28868,#23667,#23668);
#20848=AXIS2_PLACEMENT_3D('',#28869,#23669,#23670);
#20849=AXIS2_PLACEMENT_3D('',#28871,#23672,#23673);
#20850=AXIS2_PLACEMENT_3D('',#28873,#23675,#23676);
#20851=AXIS2_PLACEMENT_3D('',#28874,#23677,#23678);
#20852=AXIS2_PLACEMENT_3D('',#28876,#23680,#23681);
#20853=AXIS2_PLACEMENT_3D('',#28878,#23683,#23684);
#20854=AXIS2_PLACEMENT_3D('',#28879,#23685,#23686);
#20855=AXIS2_PLACEMENT_3D('',#28881,#23688,#23689);
#20856=AXIS2_PLACEMENT_3D('',#28883,#23691,#23692);
#20857=AXIS2_PLACEMENT_3D('',#28884,#23693,#23694);
#20858=AXIS2_PLACEMENT_3D('',#28886,#23696,#23697);
#20859=AXIS2_PLACEMENT_3D('',#28888,#23699,#23700);
#20860=AXIS2_PLACEMENT_3D('',#28889,#23701,#23702);
#20861=AXIS2_PLACEMENT_3D('',#28891,#23704,#23705);
#20862=AXIS2_PLACEMENT_3D('',#28893,#23707,#23708);
#20863=AXIS2_PLACEMENT_3D('',#28894,#23709,#23710);
#20864=AXIS2_PLACEMENT_3D('',#28896,#23712,#23713);
#20865=AXIS2_PLACEMENT_3D('',#28898,#23715,#23716);
#20866=AXIS2_PLACEMENT_3D('',#28899,#23717,#23718);
#20867=AXIS2_PLACEMENT_3D('',#28902,#23719,#23720);
#20868=AXIS2_PLACEMENT_3D('',#28903,#23721,#23722);
#20869=AXIS2_PLACEMENT_3D('',#28905,#23723,#23724);
#20870=AXIS2_PLACEMENT_3D('',#28907,#23725,#23726);
#20871=AXIS2_PLACEMENT_3D('',#28908,#23727,#23728);
#20872=AXIS2_PLACEMENT_3D('',#28909,#23729,#23730);
#20873=AXIS2_PLACEMENT_3D('',#28911,#23731,#23732);
#20874=AXIS2_PLACEMENT_3D('',#28913,#23733,#23734);
#20875=AXIS2_PLACEMENT_3D('',#28915,#23735,#23736);
#20876=AXIS2_PLACEMENT_3D('',#28916,#23737,#23738);
#20877=AXIS2_PLACEMENT_3D('',#28917,#23739,#23740);
#20878=AXIS2_PLACEMENT_3D('',#28920,#23741,#23742);
#20879=AXIS2_PLACEMENT_3D('',#28922,#23744,#23745);
#20880=AXIS2_PLACEMENT_3D('',#28923,#23746,#23747);
#20881=AXIS2_PLACEMENT_3D('',#28926,#23749,#23750);
#20882=AXIS2_PLACEMENT_3D('',#28927,#23751,#23752);
#20883=AXIS2_PLACEMENT_3D('',#28930,#23754,#23755);
#20884=AXIS2_PLACEMENT_3D('',#28931,#23756,#23757);
#20885=AXIS2_PLACEMENT_3D('',#28933,#23758,#23759);
#20886=AXIS2_PLACEMENT_3D('',#28934,#23760,#23761);
#20887=AXIS2_PLACEMENT_3D('',#28935,#23762,#23763);
#20888=AXIS2_PLACEMENT_3D('',#28937,#23764,#23765);
#20889=AXIS2_PLACEMENT_3D('',#28939,#23766,#23767);
#20890=AXIS2_PLACEMENT_3D('',#28940,#23768,#23769);
#20891=AXIS2_PLACEMENT_3D('',#28941,#23770,#23771);
#20892=AXIS2_PLACEMENT_3D('',#28943,#23772,#23773);
#20893=AXIS2_PLACEMENT_3D('',#28945,#23774,#23775);
#20894=AXIS2_PLACEMENT_3D('',#28946,#23776,#23777);
#20895=AXIS2_PLACEMENT_3D('',#28947,#23778,#23779);
#20896=AXIS2_PLACEMENT_3D('',#28949,#23781,#23782);
#20897=AXIS2_PLACEMENT_3D('',#28951,#23784,#23785);
#20898=AXIS2_PLACEMENT_3D('',#28952,#23786,#23787);
#20899=AXIS2_PLACEMENT_3D('',#28953,#23788,#23789);
#20900=AXIS2_PLACEMENT_3D('',#28955,#23790,#23791);
#20901=AXIS2_PLACEMENT_3D('',#28957,#23792,#23793);
#20902=AXIS2_PLACEMENT_3D('',#28958,#23794,#23795);
#20903=AXIS2_PLACEMENT_3D('',#28959,#23796,#23797);
#20904=AXIS2_PLACEMENT_3D('',#28961,#23798,#23799);
#20905=AXIS2_PLACEMENT_3D('',#28964,#23801,#23802);
#20906=AXIS2_PLACEMENT_3D('',#28965,#23803,#23804);
#20907=AXIS2_PLACEMENT_3D('',#28967,#23805,#23806);
#20908=AXIS2_PLACEMENT_3D('',#28968,#23807,#23808);
#20909=AXIS2_PLACEMENT_3D('',#28969,#23809,#23810);
#20910=AXIS2_PLACEMENT_3D('',#28972,#23812,#23813);
#20911=AXIS2_PLACEMENT_3D('',#28973,#23814,#23815);
#20912=AXIS2_PLACEMENT_3D('',#28976,#23816,#23817);
#20913=AXIS2_PLACEMENT_3D('',#28979,#23819,#23820);
#20914=AXIS2_PLACEMENT_3D('',#28980,#23821,#23822);
#20915=AXIS2_PLACEMENT_3D('',#28981,#23823,#23824);
#20916=AXIS2_PLACEMENT_3D('',#28982,#23825,#23826);
#20917=AXIS2_PLACEMENT_3D('',#28983,#23827,#23828);
#20918=AXIS2_PLACEMENT_3D('',#28985,#23829,#23830);
#20919=AXIS2_PLACEMENT_3D('',#28987,#23832,#23833);
#20920=AXIS2_PLACEMENT_3D('',#28990,#23835,#23836);
#20921=AXIS2_PLACEMENT_3D('',#28991,#23837,#23838);
#20922=AXIS2_PLACEMENT_3D('',#28992,#23839,#23840);
#20923=AXIS2_PLACEMENT_3D('',#28993,#23841,#23842);
#20924=AXIS2_PLACEMENT_3D('',#28996,#23843,#23844);
#20925=AXIS2_PLACEMENT_3D('',#28997,#23845,#23846);
#20926=AXIS2_PLACEMENT_3D('',#29000,#23847,#23848);
#20927=AXIS2_PLACEMENT_3D('',#29001,#23849,#23850);
#20928=AXIS2_PLACEMENT_3D('',#29004,#23851,#23852);
#20929=AXIS2_PLACEMENT_3D('',#29005,#23853,#23854);
#20930=AXIS2_PLACEMENT_3D('',#29008,#23855,#23856);
#20931=AXIS2_PLACEMENT_3D('',#29009,#23857,#23858);
#20932=AXIS2_PLACEMENT_3D('',#29012,#23859,#23860);
#20933=AXIS2_PLACEMENT_3D('',#29013,#23861,#23862);
#20934=AXIS2_PLACEMENT_3D('',#29016,#23863,#23864);
#20935=AXIS2_PLACEMENT_3D('',#29017,#23865,#23866);
#20936=AXIS2_PLACEMENT_3D('',#29020,#23867,#23868);
#20937=AXIS2_PLACEMENT_3D('',#29021,#23869,#23870);
#20938=AXIS2_PLACEMENT_3D('',#29024,#23871,#23872);
#20939=AXIS2_PLACEMENT_3D('',#29025,#23873,#23874);
#20940=AXIS2_PLACEMENT_3D('',#29027,#23875,#23876);
#20941=AXIS2_PLACEMENT_3D('',#29029,#23877,#23878);
#20942=AXIS2_PLACEMENT_3D('',#29030,#23879,#23880);
#20943=AXIS2_PLACEMENT_3D('',#29031,#23881,#23882);
#20944=AXIS2_PLACEMENT_3D('',#29033,#23883,#23884);
#20945=AXIS2_PLACEMENT_3D('',#29036,#23886,#23887);
#20946=AXIS2_PLACEMENT_3D('',#29037,#23888,#23889);
#20947=AXIS2_PLACEMENT_3D('',#29039,#23890,#23891);
#20948=AXIS2_PLACEMENT_3D('',#29040,#23892,#23893);
#20949=AXIS2_PLACEMENT_3D('',#29041,#23894,#23895);
#20950=AXIS2_PLACEMENT_3D('',#29043,#23896,#23897);
#20951=AXIS2_PLACEMENT_3D('',#29045,#23898,#23899);
#20952=AXIS2_PLACEMENT_3D('',#29046,#23900,#23901);
#20953=AXIS2_PLACEMENT_3D('',#29047,#23902,#23903);
#20954=AXIS2_PLACEMENT_3D('',#29049,#23904,#23905);
#20955=AXIS2_PLACEMENT_3D('',#29051,#23907,#23908);
#20956=AXIS2_PLACEMENT_3D('',#29054,#23909,#23910);
#20957=AXIS2_PLACEMENT_3D('',#29056,#23911,#23912);
#20958=AXIS2_PLACEMENT_3D('',#29058,#23913,#23914);
#20959=AXIS2_PLACEMENT_3D('',#29060,#23915,#23916);
#20960=AXIS2_PLACEMENT_3D('',#29062,#23917,#23918);
#20961=AXIS2_PLACEMENT_3D('',#29064,#23919,#23920);
#20962=AXIS2_PLACEMENT_3D('',#29066,#23921,#23922);
#20963=AXIS2_PLACEMENT_3D('',#29068,#23923,#23924);
#20964=AXIS2_PLACEMENT_3D('',#29070,#23925,#23926);
#20965=AXIS2_PLACEMENT_3D('',#29071,#23927,#23928);
#20966=AXIS2_PLACEMENT_3D('',#29073,#23929,#23930);
#20967=AXIS2_PLACEMENT_3D('',#29075,#23931,#23932);
#20968=AXIS2_PLACEMENT_3D('',#29077,#23933,#23934);
#20969=AXIS2_PLACEMENT_3D('',#29079,#23935,#23936);
#20970=AXIS2_PLACEMENT_3D('',#29081,#23937,#23938);
#20971=AXIS2_PLACEMENT_3D('',#29083,#23939,#23940);
#20972=AXIS2_PLACEMENT_3D('',#29085,#23941,#23942);
#20973=AXIS2_PLACEMENT_3D('',#29086,#23943,#23944);
#20974=AXIS2_PLACEMENT_3D('',#29087,#23945,#23946);
#20975=AXIS2_PLACEMENT_3D('',#29089,#23947,#23948);
#20976=AXIS2_PLACEMENT_3D('',#29091,#23949,#23950);
#20977=AXIS2_PLACEMENT_3D('',#29092,#23951,#23952);
#20978=AXIS2_PLACEMENT_3D('',#29093,#23953,#23954);
#20979=AXIS2_PLACEMENT_3D('',#29095,#23956,#23957);
#20980=AXIS2_PLACEMENT_3D('',#29097,#23958,#23959);
#20981=AXIS2_PLACEMENT_3D('',#29099,#23960,#23961);
#20982=AXIS2_PLACEMENT_3D('',#29101,#23962,#23963);
#20983=AXIS2_PLACEMENT_3D('',#29103,#23964,#23965);
#20984=AXIS2_PLACEMENT_3D('',#29105,#23966,#23967);
#20985=AXIS2_PLACEMENT_3D('',#29107,#23968,#23969);
#20986=AXIS2_PLACEMENT_3D('',#29109,#23970,#23971);
#20987=AXIS2_PLACEMENT_3D('',#29111,#23972,#23973);
#20988=AXIS2_PLACEMENT_3D('',#29113,#23974,#23975);
#20989=AXIS2_PLACEMENT_3D('',#29115,#23976,#23977);
#20990=AXIS2_PLACEMENT_3D('',#29117,#23978,#23979);
#20991=AXIS2_PLACEMENT_3D('',#29119,#23980,#23981);
#20992=AXIS2_PLACEMENT_3D('',#29121,#23982,#23983);
#20993=AXIS2_PLACEMENT_3D('',#29123,#23984,#23985);
#20994=AXIS2_PLACEMENT_3D('',#29125,#23986,#23987);
#20995=AXIS2_PLACEMENT_3D('',#29127,#23988,#23989);
#20996=AXIS2_PLACEMENT_3D('',#29129,#23990,#23991);
#20997=AXIS2_PLACEMENT_3D('',#29131,#23992,#23993);
#20998=AXIS2_PLACEMENT_3D('',#29133,#23994,#23995);
#20999=AXIS2_PLACEMENT_3D('',#29135,#23996,#23997);
#21000=AXIS2_PLACEMENT_3D('',#29137,#23998,#23999);
#21001=AXIS2_PLACEMENT_3D('',#29139,#24000,#24001);
#21002=AXIS2_PLACEMENT_3D('',#29141,#24002,#24003);
#21003=AXIS2_PLACEMENT_3D('',#29143,#24004,#24005);
#21004=AXIS2_PLACEMENT_3D('',#29145,#24006,#24007);
#21005=AXIS2_PLACEMENT_3D('',#29147,#24008,#24009);
#21006=AXIS2_PLACEMENT_3D('',#29149,#24010,#24011);
#21007=AXIS2_PLACEMENT_3D('',#29151,#24012,#24013);
#21008=AXIS2_PLACEMENT_3D('',#29153,#24014,#24015);
#21009=AXIS2_PLACEMENT_3D('',#29155,#24016,#24017);
#21010=AXIS2_PLACEMENT_3D('',#29157,#24018,#24019);
#21011=AXIS2_PLACEMENT_3D('',#29159,#24020,#24021);
#21012=AXIS2_PLACEMENT_3D('',#29161,#24022,#24023);
#21013=AXIS2_PLACEMENT_3D('',#29162,#24024,#24025);
#21014=AXIS2_PLACEMENT_3D('',#29163,#24026,#24027);
#21015=AXIS2_PLACEMENT_3D('',#29167,#24029,#24030);
#21016=AXIS2_PLACEMENT_3D('',#29169,#24032,#24033);
#21017=AXIS2_PLACEMENT_3D('',#29172,#24034,#24035);
#21018=AXIS2_PLACEMENT_3D('',#29175,#24038,#24039);
#21019=AXIS2_PLACEMENT_3D('',#29179,#24041,#24042);
#21020=AXIS2_PLACEMENT_3D('',#29181,#24044,#24045);
#21021=AXIS2_PLACEMENT_3D('',#29185,#24047,#24048);
#21022=AXIS2_PLACEMENT_3D('',#29187,#24050,#24051);
#21023=AXIS2_PLACEMENT_3D('',#29191,#24053,#24054);
#21024=AXIS2_PLACEMENT_3D('',#29193,#24056,#24057);
#21025=AXIS2_PLACEMENT_3D('',#29197,#24059,#24060);
#21026=AXIS2_PLACEMENT_3D('',#29199,#24062,#24063);
#21027=AXIS2_PLACEMENT_3D('',#29203,#24065,#24066);
#21028=AXIS2_PLACEMENT_3D('',#29205,#24068,#24069);
#21029=AXIS2_PLACEMENT_3D('',#29208,#24070,#24071);
#21030=AXIS2_PLACEMENT_3D('',#29211,#24074,#24075);
#21031=AXIS2_PLACEMENT_3D('',#29215,#24077,#24078);
#21032=AXIS2_PLACEMENT_3D('',#29217,#24080,#24081);
#21033=AXIS2_PLACEMENT_3D('',#29220,#24082,#24083);
#21034=AXIS2_PLACEMENT_3D('',#29223,#24086,#24087);
#21035=AXIS2_PLACEMENT_3D('',#29227,#24089,#24090);
#21036=AXIS2_PLACEMENT_3D('',#29229,#24092,#24093);
#21037=AXIS2_PLACEMENT_3D('',#29233,#24095,#24096);
#21038=AXIS2_PLACEMENT_3D('',#29235,#24098,#24099);
#21039=AXIS2_PLACEMENT_3D('',#29239,#24101,#24102);
#21040=AXIS2_PLACEMENT_3D('',#29241,#24104,#24105);
#21041=AXIS2_PLACEMENT_3D('',#29245,#24107,#24108);
#21042=AXIS2_PLACEMENT_3D('',#29247,#24110,#24111);
#21043=AXIS2_PLACEMENT_3D('',#29251,#24113,#24114);
#21044=AXIS2_PLACEMENT_3D('',#29253,#24116,#24117);
#21045=AXIS2_PLACEMENT_3D('',#29256,#24118,#24119);
#21046=AXIS2_PLACEMENT_3D('',#29259,#24122,#24123);
#21047=AXIS2_PLACEMENT_3D('',#29262,#24126,#24127);
#21048=AXIS2_PLACEMENT_3D('',#29265,#24130,#24131);
#21049=AXIS2_PLACEMENT_3D('',#29268,#24134,#24135);
#21050=AXIS2_PLACEMENT_3D('',#29271,#24138,#24139);
#21051=AXIS2_PLACEMENT_3D('',#29274,#24142,#24143);
#21052=AXIS2_PLACEMENT_3D('',#29277,#24146,#24147);
#21053=AXIS2_PLACEMENT_3D('',#29280,#24150,#24151);
#21054=AXIS2_PLACEMENT_3D('',#29283,#24154,#24155);
#21055=AXIS2_PLACEMENT_3D('',#29284,#24156,#24157);
#21056=AXIS2_PLACEMENT_3D('',#29285,#24158,#24159);
#21057=AXIS2_PLACEMENT_3D('',#29287,#24161,#24162);
#21058=AXIS2_PLACEMENT_3D('',#29289,#24164,#24165);
#21059=AXIS2_PLACEMENT_3D('',#29290,#24166,#24167);
#21060=AXIS2_PLACEMENT_3D('',#29292,#24169,#24170);
#21061=AXIS2_PLACEMENT_3D('',#29294,#24172,#24173);
#21062=AXIS2_PLACEMENT_3D('',#29295,#24174,#24175);
#21063=AXIS2_PLACEMENT_3D('',#29297,#24177,#24178);
#21064=AXIS2_PLACEMENT_3D('',#29299,#24180,#24181);
#21065=AXIS2_PLACEMENT_3D('',#29300,#24182,#24183);
#21066=AXIS2_PLACEMENT_3D('',#29302,#24185,#24186);
#21067=AXIS2_PLACEMENT_3D('',#29304,#24188,#24189);
#21068=AXIS2_PLACEMENT_3D('',#29305,#24190,#24191);
#21069=AXIS2_PLACEMENT_3D('',#29307,#24193,#24194);
#21070=AXIS2_PLACEMENT_3D('',#29309,#24196,#24197);
#21071=AXIS2_PLACEMENT_3D('',#29310,#24198,#24199);
#21072=AXIS2_PLACEMENT_3D('',#29312,#24201,#24202);
#21073=AXIS2_PLACEMENT_3D('',#29314,#24204,#24205);
#21074=AXIS2_PLACEMENT_3D('',#29315,#24206,#24207);
#21075=AXIS2_PLACEMENT_3D('',#29317,#24209,#24210);
#21076=AXIS2_PLACEMENT_3D('',#29319,#24212,#24213);
#21077=AXIS2_PLACEMENT_3D('',#29320,#24214,#24215);
#21078=AXIS2_PLACEMENT_3D('',#29322,#24217,#24218);
#21079=AXIS2_PLACEMENT_3D('',#29324,#24220,#24221);
#21080=AXIS2_PLACEMENT_3D('',#29325,#24222,#24223);
#21081=AXIS2_PLACEMENT_3D('',#29326,#24224,#24225);
#21082=AXIS2_PLACEMENT_3D('',#29335,#24230,#24231);
#21083=AXIS2_PLACEMENT_3D('',#29341,#24235,#24236);
#21084=AXIS2_PLACEMENT_3D('',#29347,#24240,#24241);
#21085=AXIS2_PLACEMENT_3D('',#29356,#24246,#24247);
#21086=AXIS2_PLACEMENT_3D('',#29362,#24251,#24252);
#21087=AXIS2_PLACEMENT_3D('',#29368,#24256,#24257);
#21088=AXIS2_PLACEMENT_3D('',#29374,#24261,#24262);
#21089=AXIS2_PLACEMENT_3D('',#29380,#24266,#24267);
#21090=AXIS2_PLACEMENT_3D('',#29386,#24271,#24272);
#21091=AXIS2_PLACEMENT_3D('',#29395,#24277,#24278);
#21092=AXIS2_PLACEMENT_3D('',#29401,#24282,#24283);
#21093=AXIS2_PLACEMENT_3D('',#29407,#24287,#24288);
#21094=AXIS2_PLACEMENT_3D('',#29413,#24292,#24293);
#21095=AXIS2_PLACEMENT_3D('',#29422,#24298,#24299);
#21096=AXIS2_PLACEMENT_3D('',#29428,#24303,#24304);
#21097=AXIS2_PLACEMENT_3D('',#29434,#24308,#24309);
#21098=AXIS2_PLACEMENT_3D('',#29440,#24313,#24314);
#21099=AXIS2_PLACEMENT_3D('',#29446,#24318,#24319);
#21100=AXIS2_PLACEMENT_3D('',#29449,#24322,#24323);
#21101=AXIS2_PLACEMENT_3D('',#29458,#24328,#24329);
#21102=AXIS2_PLACEMENT_3D('',#29464,#24333,#24334);
#21103=AXIS2_PLACEMENT_3D('',#29470,#24338,#24339);
#21104=AXIS2_PLACEMENT_3D('',#29473,#24342,#24343);
#21105=AXIS2_PLACEMENT_3D('',#29482,#24348,#24349);
#21106=AXIS2_PLACEMENT_3D('',#29488,#24353,#24354);
#21107=AXIS2_PLACEMENT_3D('',#29494,#24358,#24359);
#21108=AXIS2_PLACEMENT_3D('',#29500,#24363,#24364);
#21109=AXIS2_PLACEMENT_3D('',#29506,#24368,#24369);
#21110=AXIS2_PLACEMENT_3D('',#29512,#24373,#24374);
#21111=AXIS2_PLACEMENT_3D('',#29521,#24379,#24380);
#21112=AXIS2_PLACEMENT_3D('',#29527,#24384,#24385);
#21113=AXIS2_PLACEMENT_3D('',#29533,#24389,#24390);
#21114=AXIS2_PLACEMENT_3D('',#29536,#24393,#24394);
#21115=AXIS2_PLACEMENT_3D('',#29538,#24395,#24396);
#21116=AXIS2_PLACEMENT_3D('',#29541,#24398,#24399);
#21117=AXIS2_PLACEMENT_3D('',#29542,#24400,#24401);
#21118=AXIS2_PLACEMENT_3D('',#29548,#24405,#24406);
#21119=AXIS2_PLACEMENT_3D('',#29557,#24411,#24412);
#21120=AXIS2_PLACEMENT_3D('',#29563,#24416,#24417);
#21121=AXIS2_PLACEMENT_3D('',#29569,#24421,#24422);
#21122=AXIS2_PLACEMENT_3D('',#29575,#24426,#24427);
#21123=AXIS2_PLACEMENT_3D('',#29581,#24431,#24432);
#21124=AXIS2_PLACEMENT_3D('',#29584,#24435,#24436);
#21125=AXIS2_PLACEMENT_3D('',#29593,#24441,#24442);
#21126=AXIS2_PLACEMENT_3D('',#29595,#24443,#24444);
#21127=AXIS2_PLACEMENT_3D('',#29597,#24445,#24446);
#21128=AXIS2_PLACEMENT_3D('',#29599,#24448,#24449);
#21129=AXIS2_PLACEMENT_3D('',#29605,#24453,#24454);
#21130=AXIS2_PLACEMENT_3D('',#29607,#24455,#24456);
#21131=AXIS2_PLACEMENT_3D('',#29609,#24457,#24458);
#21132=AXIS2_PLACEMENT_3D('',#29611,#24460,#24461);
#21133=AXIS2_PLACEMENT_3D('',#29620,#24466,#24467);
#21134=AXIS2_PLACEMENT_3D('',#29626,#24471,#24472);
#21135=AXIS2_PLACEMENT_3D('',#29632,#24476,#24477);
#21136=AXIS2_PLACEMENT_3D('',#29638,#24481,#24482);
#21137=AXIS2_PLACEMENT_3D('',#29644,#24486,#24487);
#21138=AXIS2_PLACEMENT_3D('',#29650,#24491,#24492);
#21139=AXIS2_PLACEMENT_3D('',#29653,#24495,#24496);
#21140=AXIS2_PLACEMENT_3D('',#29659,#24500,#24501);
#21141=AXIS2_PLACEMENT_3D('',#29665,#24505,#24506);
#21142=AXIS2_PLACEMENT_3D('',#29671,#24510,#24511);
#21143=AXIS2_PLACEMENT_3D('',#29677,#24515,#24516);
#21144=AXIS2_PLACEMENT_3D('',#29679,#24517,#24518);
#21145=AXIS2_PLACEMENT_3D('',#29682,#24520,#24521);
#21146=AXIS2_PLACEMENT_3D('',#29683,#24522,#24523);
#21147=AXIS2_PLACEMENT_3D('',#29689,#24527,#24528);
#21148=AXIS2_PLACEMENT_3D('',#29691,#24529,#24530);
#21149=AXIS2_PLACEMENT_3D('',#29694,#24532,#24533);
#21150=AXIS2_PLACEMENT_3D('',#29695,#24534,#24535);
#21151=AXIS2_PLACEMENT_3D('',#29698,#24538,#24539);
#21152=AXIS2_PLACEMENT_3D('',#29704,#24543,#24544);
#21153=AXIS2_PLACEMENT_3D('',#29710,#24548,#24549);
#21154=AXIS2_PLACEMENT_3D('',#29716,#24553,#24554);
#21155=AXIS2_PLACEMENT_3D('',#29722,#24558,#24559);
#21156=AXIS2_PLACEMENT_3D('',#29728,#24563,#24564);
#21157=AXIS2_PLACEMENT_3D('',#29734,#24568,#24569);
#21158=AXIS2_PLACEMENT_3D('',#29740,#24573,#24574);
#21159=AXIS2_PLACEMENT_3D('',#29746,#24578,#24579);
#21160=AXIS2_PLACEMENT_3D('',#29748,#24580,#24581);
#21161=AXIS2_PLACEMENT_3D('',#29751,#24583,#24584);
#21162=AXIS2_PLACEMENT_3D('',#29752,#24585,#24586);
#21163=AXIS2_PLACEMENT_3D('',#29758,#24590,#24591);
#21164=AXIS2_PLACEMENT_3D('',#29764,#24595,#24596);
#21165=AXIS2_PLACEMENT_3D('',#29770,#24600,#24601);
#21166=AXIS2_PLACEMENT_3D('',#29776,#24605,#24606);
#21167=AXIS2_PLACEMENT_3D('',#29782,#24610,#24611);
#21168=AXIS2_PLACEMENT_3D('',#29788,#24615,#24616);
#21169=AXIS2_PLACEMENT_3D('',#29794,#24620,#24621);
#21170=AXIS2_PLACEMENT_3D('',#29803,#24626,#24627);
#21171=AXIS2_PLACEMENT_3D('',#29805,#24628,#24629);
#21172=AXIS2_PLACEMENT_3D('',#29808,#24631,#24632);
#21173=AXIS2_PLACEMENT_3D('',#29809,#24633,#24634);
#21174=AXIS2_PLACEMENT_3D('',#29815,#24638,#24639);
#21175=AXIS2_PLACEMENT_3D('',#29817,#24640,#24641);
#21176=AXIS2_PLACEMENT_3D('',#29820,#24643,#24644);
#21177=AXIS2_PLACEMENT_3D('',#29821,#24645,#24646);
#21178=AXIS2_PLACEMENT_3D('',#29830,#24651,#24652);
#21179=AXIS2_PLACEMENT_3D('',#29836,#24656,#24657);
#21180=AXIS2_PLACEMENT_3D('',#29842,#24661,#24662);
#21181=AXIS2_PLACEMENT_3D('',#29848,#24666,#24667);
#21182=AXIS2_PLACEMENT_3D('',#29854,#24671,#24672);
#21183=AXIS2_PLACEMENT_3D('',#29860,#24676,#24677);
#21184=AXIS2_PLACEMENT_3D('',#29863,#24680,#24681);
#21185=AXIS2_PLACEMENT_3D('',#29869,#24685,#24686);
#21186=AXIS2_PLACEMENT_3D('',#29875,#24690,#24691);
#21187=AXIS2_PLACEMENT_3D('',#29881,#24695,#24696);
#21188=AXIS2_PLACEMENT_3D('',#29887,#24700,#24701);
#21189=AXIS2_PLACEMENT_3D('',#29890,#24704,#24705);
#21190=AXIS2_PLACEMENT_3D('',#29892,#24706,#24707);
#21191=AXIS2_PLACEMENT_3D('',#29895,#24709,#24710);
#21192=AXIS2_PLACEMENT_3D('',#29896,#24711,#24712);
#21193=AXIS2_PLACEMENT_3D('',#29902,#24716,#24717);
#21194=AXIS2_PLACEMENT_3D('',#29904,#24718,#24719);
#21195=AXIS2_PLACEMENT_3D('',#29906,#24720,#24721);
#21196=AXIS2_PLACEMENT_3D('',#29908,#24723,#24724);
#21197=AXIS2_PLACEMENT_3D('',#29914,#24728,#24729);
#21198=AXIS2_PLACEMENT_3D('',#29916,#24730,#24731);
#21199=AXIS2_PLACEMENT_3D('',#29918,#24732,#24733);
#21200=AXIS2_PLACEMENT_3D('',#29920,#24735,#24736);
#21201=AXIS2_PLACEMENT_3D('',#29923,#24739,#24740);
#21202=AXIS2_PLACEMENT_3D('',#29929,#24744,#24745);
#21203=AXIS2_PLACEMENT_3D('',#29935,#24749,#24750);
#21204=AXIS2_PLACEMENT_3D('',#29941,#24754,#24755);
#21205=AXIS2_PLACEMENT_3D('',#29947,#24759,#24760);
#21206=AXIS2_PLACEMENT_3D('',#29953,#24764,#24765);
#21207=AXIS2_PLACEMENT_3D('',#29959,#24769,#24770);
#21208=AXIS2_PLACEMENT_3D('',#29965,#24774,#24775);
#21209=AXIS2_PLACEMENT_3D('',#29971,#24779,#24780);
#21210=AXIS2_PLACEMENT_3D('',#29973,#24781,#24782);
#21211=AXIS2_PLACEMENT_3D('',#29975,#24783,#24784);
#21212=AXIS2_PLACEMENT_3D('',#29977,#24786,#24787);
#21213=AXIS2_PLACEMENT_3D('',#29983,#24791,#24792);
#21214=AXIS2_PLACEMENT_3D('',#29989,#24796,#24797);
#21215=AXIS2_PLACEMENT_3D('',#29995,#24801,#24802);
#21216=AXIS2_PLACEMENT_3D('',#30001,#24806,#24807);
#21217=AXIS2_PLACEMENT_3D('',#30007,#24811,#24812);
#21218=AXIS2_PLACEMENT_3D('',#30013,#24816,#24817);
#21219=AXIS2_PLACEMENT_3D('',#30016,#24820,#24821);
#21220=AXIS2_PLACEMENT_3D('',#30025,#24826,#24827);
#21221=AXIS2_PLACEMENT_3D('',#30031,#24831,#24832);
#21222=AXIS2_PLACEMENT_3D('',#30037,#24836,#24837);
#21223=AXIS2_PLACEMENT_3D('',#30046,#24842,#24843);
#21224=AXIS2_PLACEMENT_3D('',#30052,#24847,#24848);
#21225=AXIS2_PLACEMENT_3D('',#30058,#24852,#24853);
#21226=AXIS2_PLACEMENT_3D('',#30064,#24857,#24858);
#21227=AXIS2_PLACEMENT_3D('',#30070,#24862,#24863);
#21228=AXIS2_PLACEMENT_3D('',#30076,#24867,#24868);
#21229=AXIS2_PLACEMENT_3D('',#30082,#24872,#24873);
#21230=AXIS2_PLACEMENT_3D('',#30088,#24877,#24878);
#21231=AXIS2_PLACEMENT_3D('',#30094,#24882,#24883);
#21232=AXIS2_PLACEMENT_3D('',#30100,#24887,#24888);
#21233=AXIS2_PLACEMENT_3D('',#30106,#24892,#24893);
#21234=AXIS2_PLACEMENT_3D('',#30112,#24897,#24898);
#21235=AXIS2_PLACEMENT_3D('',#30118,#24902,#24903);
#21236=AXIS2_PLACEMENT_3D('',#30124,#24907,#24908);
#21237=AXIS2_PLACEMENT_3D('',#30130,#24912,#24913);
#21238=AXIS2_PLACEMENT_3D('',#30136,#24917,#24918);
#21239=AXIS2_PLACEMENT_3D('',#30142,#24922,#24923);
#21240=AXIS2_PLACEMENT_3D('',#30145,#24926,#24927);
#21241=AXIS2_PLACEMENT_3D('',#30154,#24932,#24933);
#21242=AXIS2_PLACEMENT_3D('',#30160,#24937,#24938);
#21243=AXIS2_PLACEMENT_3D('',#30166,#24942,#24943);
#21244=AXIS2_PLACEMENT_3D('',#30169,#24946,#24947);
#21245=AXIS2_PLACEMENT_3D('',#30178,#24952,#24953);
#21246=AXIS2_PLACEMENT_3D('',#30184,#24957,#24958);
#21247=AXIS2_PLACEMENT_3D('',#30190,#24962,#24963);
#21248=AXIS2_PLACEMENT_3D('',#30196,#24967,#24968);
#21249=AXIS2_PLACEMENT_3D('',#30202,#24972,#24973);
#21250=AXIS2_PLACEMENT_3D('',#30208,#24977,#24978);
#21251=AXIS2_PLACEMENT_3D('',#30214,#24982,#24983);
#21252=AXIS2_PLACEMENT_3D('',#30220,#24987,#24988);
#21253=AXIS2_PLACEMENT_3D('',#30226,#24992,#24993);
#21254=AXIS2_PLACEMENT_3D('',#30232,#24997,#24998);
#21255=AXIS2_PLACEMENT_3D('',#30235,#25001,#25002);
#21256=AXIS2_PLACEMENT_3D('',#30237,#25003,#25004);
#21257=AXIS2_PLACEMENT_3D('',#30240,#25006,#25007);
#21258=AXIS2_PLACEMENT_3D('',#30241,#25008,#25009);
#21259=AXIS2_PLACEMENT_3D('',#30247,#25013,#25014);
#21260=AXIS2_PLACEMENT_3D('',#30253,#25018,#25019);
#21261=AXIS2_PLACEMENT_3D('',#30259,#25023,#25024);
#21262=AXIS2_PLACEMENT_3D('',#30265,#25028,#25029);
#21263=AXIS2_PLACEMENT_3D('',#30271,#25033,#25034);
#21264=AXIS2_PLACEMENT_3D('',#30277,#25038,#25039);
#21265=AXIS2_PLACEMENT_3D('',#30283,#25043,#25044);
#21266=AXIS2_PLACEMENT_3D('',#30286,#25047,#25048);
#21267=AXIS2_PLACEMENT_3D('',#30295,#25053,#25054);
#21268=AXIS2_PLACEMENT_3D('',#30301,#25058,#25059);
#21269=AXIS2_PLACEMENT_3D('',#30307,#25063,#25064);
#21270=AXIS2_PLACEMENT_3D('',#30316,#25069,#25070);
#21271=AXIS2_PLACEMENT_3D('',#30322,#25074,#25075);
#21272=AXIS2_PLACEMENT_3D('',#30328,#25079,#25080);
#21273=AXIS2_PLACEMENT_3D('',#30334,#25084,#25085);
#21274=AXIS2_PLACEMENT_3D('',#30340,#25089,#25090);
#21275=AXIS2_PLACEMENT_3D('',#30346,#25094,#25095);
#21276=AXIS2_PLACEMENT_3D('',#30352,#25099,#25100);
#21277=AXIS2_PLACEMENT_3D('',#30358,#25104,#25105);
#21278=AXIS2_PLACEMENT_3D('',#30364,#25109,#25110);
#21279=AXIS2_PLACEMENT_3D('',#30370,#25114,#25115);
#21280=AXIS2_PLACEMENT_3D('',#30376,#25119,#25120);
#21281=AXIS2_PLACEMENT_3D('',#30382,#25124,#25125);
#21282=AXIS2_PLACEMENT_3D('',#30388,#25129,#25130);
#21283=AXIS2_PLACEMENT_3D('',#30394,#25134,#25135);
#21284=AXIS2_PLACEMENT_3D('',#30400,#25139,#25140);
#21285=AXIS2_PLACEMENT_3D('',#30406,#25144,#25145);
#21286=AXIS2_PLACEMENT_3D('',#30412,#25149,#25150);
#21287=AXIS2_PLACEMENT_3D('',#30415,#25153,#25154);
#21288=AXIS2_PLACEMENT_3D('',#30424,#25159,#25160);
#21289=AXIS2_PLACEMENT_3D('',#30430,#25164,#25165);
#21290=AXIS2_PLACEMENT_3D('',#30436,#25169,#25170);
#21291=AXIS2_PLACEMENT_3D('',#30439,#25173,#25174);
#21292=AXIS2_PLACEMENT_3D('',#30448,#25179,#25180);
#21293=AXIS2_PLACEMENT_3D('',#30454,#25184,#25185);
#21294=AXIS2_PLACEMENT_3D('',#30460,#25189,#25190);
#21295=AXIS2_PLACEMENT_3D('',#30466,#25194,#25195);
#21296=AXIS2_PLACEMENT_3D('',#30472,#25199,#25200);
#21297=AXIS2_PLACEMENT_3D('',#30478,#25204,#25205);
#21298=AXIS2_PLACEMENT_3D('',#30484,#25209,#25210);
#21299=AXIS2_PLACEMENT_3D('',#30490,#25214,#25215);
#21300=AXIS2_PLACEMENT_3D('',#30496,#25219,#25220);
#21301=AXIS2_PLACEMENT_3D('',#30502,#25224,#25225);
#21302=AXIS2_PLACEMENT_3D('',#30505,#25228,#25229);
#21303=AXIS2_PLACEMENT_3D('',#30507,#25230,#25231);
#21304=AXIS2_PLACEMENT_3D('',#30510,#25233,#25234);
#21305=AXIS2_PLACEMENT_3D('',#30511,#25235,#25236);
#21306=AXIS2_PLACEMENT_3D('',#30517,#25240,#25241);
#21307=AXIS2_PLACEMENT_3D('',#30523,#25245,#25246);
#21308=AXIS2_PLACEMENT_3D('',#30529,#25250,#25251);
#21309=AXIS2_PLACEMENT_3D('',#30535,#25255,#25256);
#21310=AXIS2_PLACEMENT_3D('',#30541,#25260,#25261);
#21311=AXIS2_PLACEMENT_3D('',#30547,#25265,#25266);
#21312=AXIS2_PLACEMENT_3D('',#30553,#25270,#25271);
#21313=AXIS2_PLACEMENT_3D('',#30556,#25274,#25275);
#21314=AXIS2_PLACEMENT_3D('',#30565,#25280,#25281);
#21315=AXIS2_PLACEMENT_3D('',#30567,#25282,#25283);
#21316=AXIS2_PLACEMENT_3D('',#30569,#25284,#25285);
#21317=AXIS2_PLACEMENT_3D('',#30571,#25287,#25288);
#21318=AXIS2_PLACEMENT_3D('',#30577,#25292,#25293);
#21319=AXIS2_PLACEMENT_3D('',#30579,#25294,#25295);
#21320=AXIS2_PLACEMENT_3D('',#30581,#25296,#25297);
#21321=AXIS2_PLACEMENT_3D('',#30583,#25299,#25300);
#21322=AXIS2_PLACEMENT_3D('',#30592,#25305,#25306);
#21323=AXIS2_PLACEMENT_3D('',#30598,#25310,#25311);
#21324=AXIS2_PLACEMENT_3D('',#30604,#25315,#25316);
#21325=AXIS2_PLACEMENT_3D('',#30610,#25320,#25321);
#21326=AXIS2_PLACEMENT_3D('',#30616,#25325,#25326);
#21327=AXIS2_PLACEMENT_3D('',#30622,#25330,#25331);
#21328=AXIS2_PLACEMENT_3D('',#30625,#25334,#25335);
#21329=AXIS2_PLACEMENT_3D('',#30631,#25339,#25340);
#21330=AXIS2_PLACEMENT_3D('',#30637,#25344,#25345);
#21331=AXIS2_PLACEMENT_3D('',#30643,#25349,#25350);
#21332=AXIS2_PLACEMENT_3D('',#30649,#25354,#25355);
#21333=AXIS2_PLACEMENT_3D('',#30651,#25356,#25357);
#21334=AXIS2_PLACEMENT_3D('',#30654,#25359,#25360);
#21335=AXIS2_PLACEMENT_3D('',#30655,#25361,#25362);
#21336=AXIS2_PLACEMENT_3D('',#30661,#25366,#25367);
#21337=AXIS2_PLACEMENT_3D('',#30663,#25368,#25369);
#21338=AXIS2_PLACEMENT_3D('',#30666,#25371,#25372);
#21339=AXIS2_PLACEMENT_3D('',#30667,#25373,#25374);
#21340=AXIS2_PLACEMENT_3D('',#30670,#25377,#25378);
#21341=AXIS2_PLACEMENT_3D('',#30676,#25382,#25383);
#21342=AXIS2_PLACEMENT_3D('',#30682,#25387,#25388);
#21343=AXIS2_PLACEMENT_3D('',#30688,#25392,#25393);
#21344=AXIS2_PLACEMENT_3D('',#30694,#25397,#25398);
#21345=AXIS2_PLACEMENT_3D('',#30700,#25402,#25403);
#21346=AXIS2_PLACEMENT_3D('',#30706,#25407,#25408);
#21347=AXIS2_PLACEMENT_3D('',#30712,#25412,#25413);
#21348=AXIS2_PLACEMENT_3D('',#30718,#25417,#25418);
#21349=AXIS2_PLACEMENT_3D('',#30720,#25419,#25420);
#21350=AXIS2_PLACEMENT_3D('',#30723,#25422,#25423);
#21351=AXIS2_PLACEMENT_3D('',#30724,#25424,#25425);
#21352=AXIS2_PLACEMENT_3D('',#30730,#25429,#25430);
#21353=AXIS2_PLACEMENT_3D('',#30736,#25434,#25435);
#21354=AXIS2_PLACEMENT_3D('',#30742,#25439,#25440);
#21355=AXIS2_PLACEMENT_3D('',#30748,#25444,#25445);
#21356=AXIS2_PLACEMENT_3D('',#30754,#25449,#25450);
#21357=AXIS2_PLACEMENT_3D('',#30760,#25454,#25455);
#21358=AXIS2_PLACEMENT_3D('',#30766,#25459,#25460);
#21359=AXIS2_PLACEMENT_3D('',#30798,#25476,#25477);
#21360=AXIS2_PLACEMENT_3D('',#30825,#25491,#25492);
#21361=AXIS2_PLACEMENT_3D('',#30829,#25494,#25495);
#21362=AXIS2_PLACEMENT_3D('',#30833,#25497,#25498);
#21363=AXIS2_PLACEMENT_3D('',#30837,#25500,#25501);
#21364=AXIS2_PLACEMENT_3D('',#30840,#25503,#25504);
#21365=AXIS2_PLACEMENT_3D('',#30841,#25505,#25506);
#21366=AXIS2_PLACEMENT_3D('',#30847,#25510,#25511);
#21367=AXIS2_PLACEMENT_3D('',#30850,#25513,#25514);
#21368=AXIS2_PLACEMENT_3D('',#30851,#25515,#25516);
#21369=AXIS2_PLACEMENT_3D('',#30855,#25519,#25520);
#21370=AXIS2_PLACEMENT_3D('',#30858,#25522,#25523);
#21371=AXIS2_PLACEMENT_3D('',#30859,#25524,#25525);
#21372=AXIS2_PLACEMENT_3D('',#30865,#25529,#25530);
#21373=AXIS2_PLACEMENT_3D('',#30869,#25533,#25534);
#21374=AXIS2_PLACEMENT_3D('',#30873,#25537,#25538);
#21375=AXIS2_PLACEMENT_3D('',#30877,#25541,#25542);
#21376=AXIS2_PLACEMENT_3D('',#30881,#25545,#25546);
#21377=AXIS2_PLACEMENT_3D('',#30885,#25549,#25550);
#21378=AXIS2_PLACEMENT_3D('',#30887,#25552,#25553);
#21379=AXIS2_PLACEMENT_3D('',#30891,#25556,#25557);
#21380=AXIS2_PLACEMENT_3D('',#30895,#25560,#25561);
#21381=AXIS2_PLACEMENT_3D('',#30899,#25564,#25565);
#21382=AXIS2_PLACEMENT_3D('',#30903,#25568,#25569);
#21383=AXIS2_PLACEMENT_3D('',#30905,#25571,#25572);
#21384=AXIS2_PLACEMENT_3D('',#30907,#25573,#25574);
#21385=AXIS2_PLACEMENT_3D('',#30909,#25576,#25577);
#21386=AXIS2_PLACEMENT_3D('',#30913,#25580,#25581);
#21387=AXIS2_PLACEMENT_3D('',#30915,#25582,#25583);
#21388=AXIS2_PLACEMENT_3D('',#30917,#25585,#25586);
#21389=AXIS2_PLACEMENT_3D('',#30921,#25589,#25590);
#21390=AXIS2_PLACEMENT_3D('',#30923,#25591,#25592);
#21391=AXIS2_PLACEMENT_3D('',#30925,#25594,#25595);
#21392=AXIS2_PLACEMENT_3D('',#30927,#25597,#25598);
#21393=AXIS2_PLACEMENT_3D('',#30931,#25601,#25602);
#21394=AXIS2_PLACEMENT_3D('',#30935,#25605,#25606);
#21395=AXIS2_PLACEMENT_3D('',#30939,#25609,#25610);
#21396=AXIS2_PLACEMENT_3D('',#30943,#25613,#25614);
#21397=AXIS2_PLACEMENT_3D('',#30947,#25617,#25618);
#21398=AXIS2_PLACEMENT_3D('',#30951,#25621,#25622);
#21399=AXIS2_PLACEMENT_3D('',#30955,#25625,#25626);
#21400=AXIS2_PLACEMENT_3D('',#30959,#25629,#25630);
#21401=AXIS2_PLACEMENT_3D('',#30961,#25631,#25632);
#21402=AXIS2_PLACEMENT_3D('',#30963,#25634,#25635);
#21403=AXIS2_PLACEMENT_3D('',#30967,#25638,#25639);
#21404=AXIS2_PLACEMENT_3D('',#30971,#25642,#25643);
#21405=AXIS2_PLACEMENT_3D('',#30975,#25646,#25647);
#21406=AXIS2_PLACEMENT_3D('',#30979,#25650,#25651);
#21407=AXIS2_PLACEMENT_3D('',#30983,#25654,#25655);
#21408=AXIS2_PLACEMENT_3D('',#30987,#25658,#25659);
#21409=AXIS2_PLACEMENT_3D('',#30989,#25661,#25662);
#21410=AXIS2_PLACEMENT_3D('',#30990,#25663,#25664);
#21411=AXIS2_PLACEMENT_3D('',#30991,#25665,#25666);
#21412=AXIS2_PLACEMENT_3D('',#31010,#25668,#25669);
#21413=AXIS2_PLACEMENT_3D('',#31015,#25670,#25671);
#21414=AXIS2_PLACEMENT_3D('',#31069,#25673,#25674);
#21415=AXIS2_PLACEMENT_3D('',#31126,#25676,#25677);
#21416=AXIS2_PLACEMENT_3D('',#31180,#25679,#25680);
#21417=AXIS2_PLACEMENT_3D('',#31234,#25682,#25683);
#21418=AXIS2_PLACEMENT_3D('',#31288,#25685,#25686);
#21419=AXIS2_PLACEMENT_3D('',#31339,#25688,#25689);
#21420=AXIS2_PLACEMENT_3D('',#31393,#25691,#25692);
#21421=AXIS2_PLACEMENT_3D('',#31447,#25694,#25695);
#21422=AXIS2_PLACEMENT_3D('',#31501,#25697,#25698);
#21423=AXIS2_PLACEMENT_3D('',#31555,#25700,#25701);
#21424=AXIS2_PLACEMENT_3D('',#31609,#25703,#25704);
#21425=AXIS2_PLACEMENT_3D('',#31663,#25706,#25707);
#21426=AXIS2_PLACEMENT_3D('',#31717,#25709,#25710);
#21427=AXIS2_PLACEMENT_3D('',#31771,#25712,#25713);
#21428=AXIS2_PLACEMENT_3D('',#31825,#25715,#25716);
#21429=AXIS2_PLACEMENT_3D('',#31879,#25718,#25719);
#21430=AXIS2_PLACEMENT_3D('',#31936,#25721,#25722);
#21431=AXIS2_PLACEMENT_3D('',#31990,#25724,#25725);
#21432=AXIS2_PLACEMENT_3D('',#32044,#25727,#25728);
#21433=AXIS2_PLACEMENT_3D('',#32098,#25730,#25731);
#21434=AXIS2_PLACEMENT_3D('',#32149,#25733,#25734);
#21435=AXIS2_PLACEMENT_3D('',#32203,#25736,#25737);
#21436=AXIS2_PLACEMENT_3D('',#32257,#25739,#25740);
#21437=AXIS2_PLACEMENT_3D('',#32311,#25742,#25743);
#21438=AXIS2_PLACEMENT_3D('',#32365,#25745,#25746);
#21439=AXIS2_PLACEMENT_3D('',#32419,#25748,#25749);
#21440=AXIS2_PLACEMENT_3D('',#32476,#25751,#25752);
#21441=AXIS2_PLACEMENT_3D('',#32530,#25754,#25755);
#21442=AXIS2_PLACEMENT_3D('',#32584,#25757,#25758);
#21443=AXIS2_PLACEMENT_3D('',#32641,#25760,#25761);
#21444=AXIS2_PLACEMENT_3D('',#32695,#25763,#25764);
#21445=AXIS2_PLACEMENT_3D('',#32749,#25766,#25767);
#21446=AXIS2_PLACEMENT_3D('',#32803,#25769,#25770);
#21447=AXIS2_PLACEMENT_3D('',#32857,#25772,#25773);
#21448=AXIS2_PLACEMENT_3D('',#32911,#25775,#25776);
#21449=AXIS2_PLACEMENT_3D('',#32962,#25778,#25779);
#21450=AXIS2_PLACEMENT_3D('',#33016,#25781,#25782);
#21451=AXIS2_PLACEMENT_3D('',#33070,#25784,#25785);
#21452=AXIS2_PLACEMENT_3D('',#33124,#25787,#25788);
#21453=AXIS2_PLACEMENT_3D('',#33181,#25790,#25791);
#21454=AXIS2_PLACEMENT_3D('',#33235,#25793,#25794);
#21455=AXIS2_PLACEMENT_3D('',#33289,#25796,#25797);
#21456=AXIS2_PLACEMENT_3D('',#33343,#25799,#25800);
#21457=AXIS2_PLACEMENT_3D('',#33397,#25802,#25803);
#21458=AXIS2_PLACEMENT_3D('',#33451,#25805,#25806);
#21459=AXIS2_PLACEMENT_3D('',#33505,#25808,#25809);
#21460=AXIS2_PLACEMENT_3D('',#33559,#25811,#25812);
#21461=AXIS2_PLACEMENT_3D('',#33613,#25814,#25815);
#21462=AXIS2_PLACEMENT_3D('',#33667,#25817,#25818);
#21463=AXIS2_PLACEMENT_3D('',#33721,#25820,#25821);
#21464=AXIS2_PLACEMENT_3D('',#33772,#25823,#25824);
#21465=AXIS2_PLACEMENT_3D('',#33826,#25826,#25827);
#21466=AXIS2_PLACEMENT_3D('',#33880,#25829,#25830);
#21467=AXIS2_PLACEMENT_3D('',#33934,#25832,#25833);
#21468=AXIS2_PLACEMENT_3D('',#33988,#25835,#25836);
#21469=AXIS2_PLACEMENT_3D('',#34042,#25838,#25839);
#21470=AXIS2_PLACEMENT_3D('',#34096,#25841,#25842);
#21471=AXIS2_PLACEMENT_3D('',#34147,#25844,#25845);
#21472=AXIS2_PLACEMENT_3D('',#34201,#25847,#25848);
#21473=AXIS2_PLACEMENT_3D('',#34255,#25850,#25851);
#21474=AXIS2_PLACEMENT_3D('',#34309,#25853,#25854);
#21475=AXIS2_PLACEMENT_3D('',#34360,#25856,#25857);
#21476=AXIS2_PLACEMENT_3D('',#34414,#25859,#25860);
#21477=AXIS2_PLACEMENT_3D('',#34468,#25862,#25863);
#21478=AXIS2_PLACEMENT_3D('',#34522,#25865,#25866);
#21479=AXIS2_PLACEMENT_3D('',#34576,#25868,#25869);
#21480=AXIS2_PLACEMENT_3D('',#34630,#25871,#25872);
#21481=AXIS2_PLACEMENT_3D('',#34687,#25874,#25875);
#21482=AXIS2_PLACEMENT_3D('',#34741,#25877,#25878);
#21483=AXIS2_PLACEMENT_3D('',#34795,#25880,#25881);
#21484=AXIS2_PLACEMENT_3D('',#34849,#25883,#25884);
#21485=AXIS2_PLACEMENT_3D('',#34903,#25886,#25887);
#21486=AXIS2_PLACEMENT_3D('',#34960,#25889,#25890);
#21487=AXIS2_PLACEMENT_3D('',#35014,#25892,#25893);
#21488=AXIS2_PLACEMENT_3D('',#35071,#25895,#25896);
#21489=AXIS2_PLACEMENT_3D('',#35125,#25898,#25899);
#21490=AXIS2_PLACEMENT_3D('',#35176,#25901,#25902);
#21491=AXIS2_PLACEMENT_3D('',#35230,#25904,#25905);
#21492=AXIS2_PLACEMENT_3D('',#35284,#25907,#25908);
#21493=AXIS2_PLACEMENT_3D('',#35338,#25910,#25911);
#21494=AXIS2_PLACEMENT_3D('',#35392,#25913,#25914);
#21495=AXIS2_PLACEMENT_3D('',#35446,#25916,#25917);
#21496=AXIS2_PLACEMENT_3D('',#35503,#25919,#25920);
#21497=AXIS2_PLACEMENT_3D('',#35557,#25922,#25923);
#21498=AXIS2_PLACEMENT_3D('',#35611,#25925,#25926);
#21499=AXIS2_PLACEMENT_3D('',#35665,#25928,#25929);
#21500=AXIS2_PLACEMENT_3D('',#35719,#25931,#25932);
#21501=AXIS2_PLACEMENT_3D('',#35773,#25934,#25935);
#21502=AXIS2_PLACEMENT_3D('',#35827,#25937,#25938);
#21503=AXIS2_PLACEMENT_3D('',#35881,#25940,#25941);
#21504=AXIS2_PLACEMENT_3D('',#35935,#25943,#25944);
#21505=AXIS2_PLACEMENT_3D('',#35986,#25946,#25947);
#21506=AXIS2_PLACEMENT_3D('',#36040,#25949,#25950);
#21507=AXIS2_PLACEMENT_3D('',#36094,#25952,#25953);
#21508=AXIS2_PLACEMENT_3D('',#36148,#25955,#25956);
#21509=AXIS2_PLACEMENT_3D('',#36202,#25958,#25959);
#21510=AXIS2_PLACEMENT_3D('',#36259,#25961,#25962);
#21511=AXIS2_PLACEMENT_3D('',#36313,#25964,#25965);
#21512=AXIS2_PLACEMENT_3D('',#36367,#25967,#25968);
#21513=AXIS2_PLACEMENT_3D('',#36372,#25970,#25971);
#21514=AXIS2_PLACEMENT_3D('',#36420,#25972,#25973);
#21515=AXIS2_PLACEMENT_3D('',#36444,#25976,#25977);
#21516=AXIS2_PLACEMENT_3D('',#36452,#25978,#25979);
#21517=AXIS2_PLACEMENT_3D('',#36466,#25980,#25981);
#21518=AXIS2_PLACEMENT_3D('',#36529,#25983,#25984);
#21519=AXIS2_PLACEMENT_3D('',#36590,#25986,#25987);
#21520=AXIS2_PLACEMENT_3D('',#36654,#25989,#25990);
#21521=AXIS2_PLACEMENT_3D('',#36718,#25992,#25993);
#21522=AXIS2_PLACEMENT_3D('',#36781,#25995,#25996);
#21523=AXIS2_PLACEMENT_3D('',#36842,#25998,#25999);
#21524=AXIS2_PLACEMENT_3D('',#36906,#26001,#26002);
#21525=AXIS2_PLACEMENT_3D('',#36969,#26004,#26005);
#21526=AXIS2_PLACEMENT_3D('',#36974,#26007,#26008);
#21527=AXIS2_PLACEMENT_3D('',#37030,#26009,#26010);
#21528=AXIS2_PLACEMENT_3D('',#37048,#26012,#26013);
#21529=AXIS2_PLACEMENT_3D('',#37058,#26014,#26015);
#21530=AXIS2_PLACEMENT_3D('',#37095,#26017,#26018);
#21531=AXIS2_PLACEMENT_3D('',#37133,#26020,#26021);
#21532=AXIS2_PLACEMENT_3D('',#37171,#26023,#26024);
#21533=AXIS2_PLACEMENT_3D('',#37207,#26026,#26027);
#21534=AXIS2_PLACEMENT_3D('',#37245,#26029,#26030);
#21535=AXIS2_PLACEMENT_3D('',#37283,#26032,#26033);
#21536=AXIS2_PLACEMENT_3D('',#37321,#26035,#26036);
#21537=AXIS2_PLACEMENT_3D('',#37357,#26038,#26039);
#21538=AXIS2_PLACEMENT_3D('',#37395,#26041,#26042);
#21539=AXIS2_PLACEMENT_3D('',#37410,#26044,#26045);
#21540=AXIS2_PLACEMENT_3D('',#37418,#26046,#26047);
#21541=AXIS2_PLACEMENT_3D('',#37444,#26049,#26050);
#21542=AXIS2_PLACEMENT_3D('',#37481,#26052,#26053);
#21543=AXIS2_PLACEMENT_3D('',#37524,#26055,#26056);
#21544=AXIS2_PLACEMENT_3D('',#37578,#26058,#26059);
#21545=AXIS2_PLACEMENT_3D('',#37629,#26061,#26062);
#21546=AXIS2_PLACEMENT_3D('',#37655,#26064,#26065);
#21547=AXIS2_PLACEMENT_3D('',#37683,#26067,#26068);
#21548=AXIS2_PLACEMENT_3D('',#37720,#26070,#26071);
#21549=AXIS2_PLACEMENT_3D('',#37774,#26073,#26074);
#21550=AXIS2_PLACEMENT_3D('',#37814,#26076,#26077);
#21551=AXIS2_PLACEMENT_3D('',#37842,#26079,#26080);
#21552=AXIS2_PLACEMENT_3D('',#37879,#26082,#26083);
#21553=AXIS2_PLACEMENT_3D('',#37919,#26085,#26086);
#21554=AXIS2_PLACEMENT_3D('',#37976,#26088,#26089);
#21555=AXIS2_PLACEMENT_3D('',#38030,#26091,#26092);
#21556=AXIS2_PLACEMENT_3D('',#38070,#26094,#26095);
#21557=AXIS2_PLACEMENT_3D('',#38096,#26097,#26098);
#21558=AXIS2_PLACEMENT_3D('',#38123,#26100,#26101);
#21559=AXIS2_PLACEMENT_3D('',#38163,#26103,#26104);
#21560=AXIS2_PLACEMENT_3D('',#38217,#26106,#26107);
#21561=AXIS2_PLACEMENT_3D('',#38261,#26109,#26110);
#21562=AXIS2_PLACEMENT_3D('',#38287,#26112,#26113);
#21563=AXIS2_PLACEMENT_3D('',#38313,#26115,#26116);
#21564=AXIS2_PLACEMENT_3D('',#38338,#26118,#26119);
#21565=AXIS2_PLACEMENT_3D('',#38366,#26121,#26122);
#21566=AXIS2_PLACEMENT_3D('',#38392,#26124,#26125);
#21567=AXIS2_PLACEMENT_3D('',#38418,#26127,#26128);
#21568=AXIS2_PLACEMENT_3D('',#38445,#26130,#26131);
#21569=AXIS2_PLACEMENT_3D('',#38471,#26133,#26134);
#21570=AXIS2_PLACEMENT_3D('',#38508,#26136,#26137);
#21571=AXIS2_PLACEMENT_3D('',#38548,#26139,#26140);
#21572=AXIS2_PLACEMENT_3D('',#38592,#26142,#26143);
#21573=AXIS2_PLACEMENT_3D('',#38617,#26145,#26146);
#21574=AXIS2_PLACEMENT_3D('',#38643,#26148,#26149);
#21575=AXIS2_PLACEMENT_3D('',#38671,#26151,#26152);
#21576=AXIS2_PLACEMENT_3D('',#38697,#26154,#26155);
#21577=AXIS2_PLACEMENT_3D('',#38734,#26157,#26158);
#21578=AXIS2_PLACEMENT_3D('',#38759,#26160,#26161);
#21579=AXIS2_PLACEMENT_3D('',#38787,#26163,#26164);
#21580=AXIS2_PLACEMENT_3D('',#38813,#26166,#26167);
#21581=AXIS2_PLACEMENT_3D('',#38839,#26169,#26170);
#21582=AXIS2_PLACEMENT_3D('',#38867,#26172,#26173);
#21583=AXIS2_PLACEMENT_3D('',#38892,#26175,#26176);
#21584=AXIS2_PLACEMENT_3D('',#38929,#26178,#26179);
#21585=AXIS2_PLACEMENT_3D('',#38955,#26181,#26182);
#21586=AXIS2_PLACEMENT_3D('',#38983,#26184,#26185);
#21587=AXIS2_PLACEMENT_3D('',#39009,#26187,#26188);
#21588=AXIS2_PLACEMENT_3D('',#39034,#26190,#26191);
#21589=AXIS2_PLACEMENT_3D('',#39062,#26193,#26194);
#21590=AXIS2_PLACEMENT_3D('',#39087,#26196,#26197);
#21591=AXIS2_PLACEMENT_3D('',#39124,#26199,#26200);
#21592=AXIS2_PLACEMENT_3D('',#39150,#26202,#26203);
#21593=AXIS2_PLACEMENT_3D('',#39178,#26205,#26206);
#21594=AXIS2_PLACEMENT_3D('',#39204,#26208,#26209);
#21595=AXIS2_PLACEMENT_3D('',#39229,#26211,#26212);
#21596=AXIS2_PLACEMENT_3D('',#39257,#26214,#26215);
#21597=AXIS2_PLACEMENT_3D('',#39283,#26217,#26218);
#21598=AXIS2_PLACEMENT_3D('',#39320,#26220,#26221);
#21599=AXIS2_PLACEMENT_3D('',#39346,#26223,#26224);
#21600=AXIS2_PLACEMENT_3D('',#39373,#26226,#26227);
#21601=AXIS2_PLACEMENT_3D('',#39399,#26229,#26230);
#21602=AXIS2_PLACEMENT_3D('',#39425,#26232,#26233);
#21603=AXIS2_PLACEMENT_3D('',#39453,#26235,#26236);
#21604=AXIS2_PLACEMENT_3D('',#39478,#26238,#26239);
#21605=AXIS2_PLACEMENT_3D('',#39504,#26241,#26242);
#21606=AXIS2_PLACEMENT_3D('',#39530,#26244,#26245);
#21607=AXIS2_PLACEMENT_3D('',#39558,#26247,#26248);
#21608=AXIS2_PLACEMENT_3D('',#39584,#26250,#26251);
#21609=AXIS2_PLACEMENT_3D('',#39610,#26253,#26254);
#21610=AXIS2_PLACEMENT_3D('',#39637,#26256,#26257);
#21611=AXIS2_PLACEMENT_3D('',#39663,#26259,#26260);
#21612=AXIS2_PLACEMENT_3D('',#39689,#26262,#26263);
#21613=AXIS2_PLACEMENT_3D('',#39715,#26265,#26266);
#21614=AXIS2_PLACEMENT_3D('',#39742,#26268,#26269);
#21615=AXIS2_PLACEMENT_3D('',#39768,#26271,#26272);
#21616=AXIS2_PLACEMENT_3D('',#39805,#26274,#26275);
#21617=AXIS2_PLACEMENT_3D('',#39833,#26277,#26278);
#21618=AXIS2_PLACEMENT_3D('',#39859,#26280,#26281);
#21619=AXIS2_PLACEMENT_3D('',#39885,#26283,#26284);
#21620=AXIS2_PLACEMENT_3D('',#39910,#26286,#26287);
#21621=AXIS2_PLACEMENT_3D('',#39938,#26289,#26290);
#21622=AXIS2_PLACEMENT_3D('',#39964,#26292,#26293);
#21623=AXIS2_PLACEMENT_3D('',#40001,#26295,#26296);
#21624=AXIS2_PLACEMENT_3D('',#40028,#26298,#26299);
#21625=AXIS2_PLACEMENT_3D('',#40054,#26301,#26302);
#21626=AXIS2_PLACEMENT_3D('',#40091,#26304,#26305);
#21627=AXIS2_PLACEMENT_3D('',#40117,#26307,#26308);
#21628=AXIS2_PLACEMENT_3D('',#40145,#26310,#26311);
#21629=AXIS2_PLACEMENT_3D('',#40170,#26313,#26314);
#21630=AXIS2_PLACEMENT_3D('',#40196,#26316,#26317);
#21631=AXIS2_PLACEMENT_3D('',#40224,#26319,#26320);
#21632=AXIS2_PLACEMENT_3D('',#40250,#26322,#26323);
#21633=AXIS2_PLACEMENT_3D('',#40287,#26325,#26326);
#21634=AXIS2_PLACEMENT_3D('',#40312,#26328,#26329);
#21635=AXIS2_PLACEMENT_3D('',#40340,#26331,#26332);
#21636=AXIS2_PLACEMENT_3D('',#40366,#26334,#26335);
#21637=AXIS2_PLACEMENT_3D('',#40392,#26337,#26338);
#21638=AXIS2_PLACEMENT_3D('',#40419,#26340,#26341);
#21639=AXIS2_PLACEMENT_3D('',#40445,#26343,#26344);
#21640=AXIS2_PLACEMENT_3D('',#40447,#26345,#26346);
#21641=AXIS2_PLACEMENT_3D('',#40450,#26348,#26349);
#21642=AXIS2_PLACEMENT_3D('',#40451,#26350,#26351);
#21643=AXIS2_PLACEMENT_3D('',#40454,#26353,#26354);
#21644=AXIS2_PLACEMENT_3D('',#40455,#26355,#26356);
#21645=AXIS2_PLACEMENT_3D('',#40456,#26357,#26358);
#21646=AXIS2_PLACEMENT_3D('',#40458,#26359,#26360);
#21647=AXIS2_PLACEMENT_3D('',#40461,#26362,#26363);
#21648=AXIS2_PLACEMENT_3D('',#40462,#26364,#26365);
#21649=AXIS2_PLACEMENT_3D('',#40465,#26367,#26368);
#21650=AXIS2_PLACEMENT_3D('',#40466,#26369,#26370);
#21651=AXIS2_PLACEMENT_3D('',#40467,#26371,#26372);
#21652=AXIS2_PLACEMENT_3D('',#40579,#26373,#26374);
#21653=AXIS2_PLACEMENT_3D('',#43550,#26375,#26376);
#21654=AXIS2_PLACEMENT_3D('',#43563,#26377,#26378);
#21655=AXIS2_PLACEMENT_3D('',#43564,#26379,#26380);
#21656=AXIS2_PLACEMENT_3D('',#43576,#26381,#26382);
#21657=AXIS2_PLACEMENT_3D('',#44132,#26383,#26384);
#21658=AXIS2_PLACEMENT_3D('',#44144,#26385,#26386);
#21659=AXIS2_PLACEMENT_3D('',#44145,#26387,#26388);
#21660=AXIS2_PLACEMENT_3D('',#44659,#26389,#26390);
#21661=AXIS2_PLACEMENT_3D('',#44660,#26391,#26392);
#21662=AXIS2_PLACEMENT_3D('',#47626,#26393,#26394);
#21663=AXIS2_PLACEMENT_3D('',#47627,#26395,#26396);
#21664=AXIS2_PLACEMENT_3D('',#47628,#26397,#26398);
#21665=AXIS2_PLACEMENT_3D('',#47631,#26399,#26400);
#21666=AXIS2_PLACEMENT_3D('',#47635,#26402,#26403);
#21667=AXIS2_PLACEMENT_3D('',#47642,#26407,#26408);
#21668=AXIS2_PLACEMENT_3D('',#47643,#26409,#26410);
#21669=AXIS2_PLACEMENT_3D('',#47645,#26411,#26412);
#21670=AXIS2_PLACEMENT_3D('',#47648,#26414,#26415);
#21671=AXIS2_PLACEMENT_3D('',#47649,#26416,#26417);
#21672=AXIS2_PLACEMENT_3D('',#47651,#26418,#26419);
#21673=AXIS2_PLACEMENT_3D('',#47654,#26421,#26422);
#21674=AXIS2_PLACEMENT_3D('',#47655,#26423,#26424);
#21675=AXIS2_PLACEMENT_3D('',#47657,#26425,#26426);
#21676=AXIS2_PLACEMENT_3D('',#47660,#26428,#26429);
#21677=AXIS2_PLACEMENT_3D('',#47661,#26430,#26431);
#21678=AXIS2_PLACEMENT_3D('',#47663,#26432,#26433);
#21679=AXIS2_PLACEMENT_3D('',#47666,#26435,#26436);
#21680=AXIS2_PLACEMENT_3D('',#47667,#26437,#26438);
#21681=AXIS2_PLACEMENT_3D('',#47669,#26439,#26440);
#21682=AXIS2_PLACEMENT_3D('',#47672,#26442,#26443);
#21683=AXIS2_PLACEMENT_3D('',#47673,#26444,#26445);
#21684=AXIS2_PLACEMENT_3D('',#47675,#26446,#26447);
#21685=AXIS2_PLACEMENT_3D('',#47678,#26449,#26450);
#21686=AXIS2_PLACEMENT_3D('',#47679,#26451,#26452);
#21687=AXIS2_PLACEMENT_3D('',#47681,#26453,#26454);
#21688=AXIS2_PLACEMENT_3D('',#47684,#26456,#26457);
#21689=AXIS2_PLACEMENT_3D('',#47685,#26458,#26459);
#21690=AXIS2_PLACEMENT_3D('',#47687,#26460,#26461);
#21691=AXIS2_PLACEMENT_3D('',#47690,#26463,#26464);
#21692=AXIS2_PLACEMENT_3D('',#47691,#26465,#26466);
#21693=AXIS2_PLACEMENT_3D('',#47693,#26467,#26468);
#21694=AXIS2_PLACEMENT_3D('',#47696,#26470,#26471);
#21695=AXIS2_PLACEMENT_3D('',#47697,#26472,#26473);
#21696=AXIS2_PLACEMENT_3D('',#47699,#26474,#26475);
#21697=AXIS2_PLACEMENT_3D('',#47702,#26477,#26478);
#21698=AXIS2_PLACEMENT_3D('',#47703,#26479,#26480);
#21699=AXIS2_PLACEMENT_3D('',#47705,#26481,#26482);
#21700=AXIS2_PLACEMENT_3D('',#47708,#26484,#26485);
#21701=AXIS2_PLACEMENT_3D('',#47709,#26486,#26487);
#21702=AXIS2_PLACEMENT_3D('',#47711,#26488,#26489);
#21703=AXIS2_PLACEMENT_3D('',#47714,#26491,#26492);
#21704=AXIS2_PLACEMENT_3D('',#47715,#26493,#26494);
#21705=AXIS2_PLACEMENT_3D('',#47717,#26495,#26496);
#21706=AXIS2_PLACEMENT_3D('',#47720,#26498,#26499);
#21707=AXIS2_PLACEMENT_3D('',#47721,#26500,#26501);
#21708=AXIS2_PLACEMENT_3D('',#47723,#26502,#26503);
#21709=AXIS2_PLACEMENT_3D('',#47726,#26505,#26506);
#21710=AXIS2_PLACEMENT_3D('',#47727,#26507,#26508);
#21711=AXIS2_PLACEMENT_3D('',#47729,#26509,#26510);
#21712=AXIS2_PLACEMENT_3D('',#47732,#26512,#26513);
#21713=AXIS2_PLACEMENT_3D('',#47733,#26514,#26515);
#21714=AXIS2_PLACEMENT_3D('',#47735,#26516,#26517);
#21715=AXIS2_PLACEMENT_3D('',#47738,#26519,#26520);
#21716=AXIS2_PLACEMENT_3D('',#47739,#26521,#26522);
#21717=AXIS2_PLACEMENT_3D('',#47741,#26523,#26524);
#21718=AXIS2_PLACEMENT_3D('',#47743,#26526,#26527);
#21719=AXIS2_PLACEMENT_3D('',#47746,#26528,#26529);
#21720=AXIS2_PLACEMENT_3D('',#47749,#26532,#26533);
#21721=AXIS2_PLACEMENT_3D('',#47753,#26536,#26537);
#21722=AXIS2_PLACEMENT_3D('',#47755,#26538,#26539);
#21723=AXIS2_PLACEMENT_3D('',#47757,#26541,#26542);
#21724=AXIS2_PLACEMENT_3D('',#47761,#26545,#26546);
#21725=AXIS2_PLACEMENT_3D('',#47765,#26549,#26550);
#21726=AXIS2_PLACEMENT_3D('',#47767,#26552,#26553);
#21727=AXIS2_PLACEMENT_3D('',#47776,#26558,#26559);
#21728=AXIS2_PLACEMENT_3D('',#47782,#26563,#26564);
#21729=AXIS2_PLACEMENT_3D('',#47788,#26568,#26569);
#21730=AXIS2_PLACEMENT_3D('',#47794,#26573,#26574);
#21731=AXIS2_PLACEMENT_3D('',#47800,#26578,#26579);
#21732=AXIS2_PLACEMENT_3D('',#47806,#26583,#26584);
#21733=AXIS2_PLACEMENT_3D('',#47812,#26588,#26589);
#21734=AXIS2_PLACEMENT_3D('',#47814,#26591,#26592);
#21735=AXIS2_PLACEMENT_3D('',#47816,#26594,#26595);
#21736=AXIS2_PLACEMENT_3D('',#47817,#26596,#26597);
#21737=AXIS2_PLACEMENT_3D('',#47818,#26598,#26599);
#21738=AXIS2_PLACEMENT_3D('',#47827,#26604,#26605);
#21739=AXIS2_PLACEMENT_3D('',#47829,#26606,#26607);
#21740=AXIS2_PLACEMENT_3D('',#47832,#26609,#26610);
#21741=AXIS2_PLACEMENT_3D('',#47833,#26611,#26612);
#21742=AXIS2_PLACEMENT_3D('',#47835,#26613,#26614);
#21743=AXIS2_PLACEMENT_3D('',#47838,#26616,#26617);
#21744=AXIS2_PLACEMENT_3D('',#47839,#26618,#26619);
#21745=AXIS2_PLACEMENT_3D('',#47841,#26620,#26621);
#21746=AXIS2_PLACEMENT_3D('',#47844,#26623,#26624);
#21747=AXIS2_PLACEMENT_3D('',#47845,#26625,#26626);
#21748=AXIS2_PLACEMENT_3D('',#47851,#26630,#26631);
#21749=AXIS2_PLACEMENT_3D('',#47853,#26632,#26633);
#21750=AXIS2_PLACEMENT_3D('',#47856,#26635,#26636);
#21751=AXIS2_PLACEMENT_3D('',#47857,#26637,#26638);
#21752=AXIS2_PLACEMENT_3D('',#47859,#26639,#26640);
#21753=AXIS2_PLACEMENT_3D('',#47862,#26642,#26643);
#21754=AXIS2_PLACEMENT_3D('',#47863,#26644,#26645);
#21755=AXIS2_PLACEMENT_3D('',#47865,#26646,#26647);
#21756=AXIS2_PLACEMENT_3D('',#47868,#26649,#26650);
#21757=AXIS2_PLACEMENT_3D('',#47869,#26651,#26652);
#21758=AXIS2_PLACEMENT_3D('',#47875,#26656,#26657);
#21759=AXIS2_PLACEMENT_3D('',#47877,#26658,#26659);
#21760=AXIS2_PLACEMENT_3D('',#47880,#26661,#26662);
#21761=AXIS2_PLACEMENT_3D('',#47881,#26663,#26664);
#21762=AXIS2_PLACEMENT_3D('',#47887,#26668,#26669);
#21763=AXIS2_PLACEMENT_3D('',#47889,#26670,#26671);
#21764=AXIS2_PLACEMENT_3D('',#47892,#26673,#26674);
#21765=AXIS2_PLACEMENT_3D('',#47893,#26675,#26676);
#21766=AXIS2_PLACEMENT_3D('',#47899,#26680,#26681);
#21767=AXIS2_PLACEMENT_3D('',#47901,#26682,#26683);
#21768=AXIS2_PLACEMENT_3D('',#47904,#26685,#26686);
#21769=AXIS2_PLACEMENT_3D('',#47905,#26687,#26688);
#21770=AXIS2_PLACEMENT_3D('',#47911,#26692,#26693);
#21771=AXIS2_PLACEMENT_3D('',#47917,#26697,#26698);
#21772=AXIS2_PLACEMENT_3D('',#47927,#26703,#26704);
#21773=AXIS2_PLACEMENT_3D('',#47931,#26706,#26707);
#21774=AXIS2_PLACEMENT_3D('',#47935,#26709,#26710);
#21775=AXIS2_PLACEMENT_3D('',#47939,#26712,#26713);
#21776=AXIS2_PLACEMENT_3D('',#47941,#26714,#26715);
#21777=AXIS2_PLACEMENT_3D('',#47943,#26716,#26717);
#21778=AXIS2_PLACEMENT_3D('',#47947,#26719,#26720);
#21779=AXIS2_PLACEMENT_3D('',#47949,#26721,#26722);
#21780=AXIS2_PLACEMENT_3D('',#47951,#26723,#26724);
#21781=AXIS2_PLACEMENT_3D('',#47953,#26726,#26727);
#21782=AXIS2_PLACEMENT_3D('',#47959,#26731,#26732);
#21783=AXIS2_PLACEMENT_3D('',#47962,#26734,#26735);
#21784=AXIS2_PLACEMENT_3D('',#47963,#26736,#26737);
#21785=AXIS2_PLACEMENT_3D('',#47966,#26739,#26740);
#21786=AXIS2_PLACEMENT_3D('',#47967,#26741,#26742);
#21787=AXIS2_PLACEMENT_3D('',#47970,#26744,#26745);
#21788=AXIS2_PLACEMENT_3D('',#47971,#26746,#26747);
#21789=AXIS2_PLACEMENT_3D('',#47975,#26750,#26751);
#21790=AXIS2_PLACEMENT_3D('',#47978,#26753,#26754);
#21791=AXIS2_PLACEMENT_3D('',#47979,#26755,#26756);
#21792=AXIS2_PLACEMENT_3D('',#47982,#26758,#26759);
#21793=AXIS2_PLACEMENT_3D('',#47983,#26760,#26761);
#21794=AXIS2_PLACEMENT_3D('',#47986,#26763,#26764);
#21795=AXIS2_PLACEMENT_3D('',#47987,#26765,#26766);
#21796=AXIS2_PLACEMENT_3D('',#47991,#26769,#26770);
#21797=AXIS2_PLACEMENT_3D('',#47994,#26772,#26773);
#21798=AXIS2_PLACEMENT_3D('',#47995,#26774,#26775);
#21799=AXIS2_PLACEMENT_3D('',#47999,#26778,#26779);
#21800=AXIS2_PLACEMENT_3D('',#48002,#26781,#26782);
#21801=AXIS2_PLACEMENT_3D('',#48003,#26783,#26784);
#21802=AXIS2_PLACEMENT_3D('',#48007,#26787,#26788);
#21803=AXIS2_PLACEMENT_3D('',#48010,#26790,#26791);
#21804=AXIS2_PLACEMENT_3D('',#48011,#26792,#26793);
#21805=AXIS2_PLACEMENT_3D('',#48015,#26796,#26797);
#21806=AXIS2_PLACEMENT_3D('',#48019,#26800,#26801);
#21807=AXIS2_PLACEMENT_3D('',#48021,#26803,#26804);
#21808=AXIS2_PLACEMENT_3D('',#48023,#26806,#26807);
#21809=AXIS2_PLACEMENT_3D('',#48024,#26808,#26809);
#21810=AXIS2_PLACEMENT_3D('',#48025,#26810,#26811);
#21811=AXIS2_PLACEMENT_3D('',#48027,#26812,#26813);
#21812=AXIS2_PLACEMENT_3D('',#48030,#26815,#26816);
#21813=AXIS2_PLACEMENT_3D('',#48031,#26817,#26818);
#21814=AXIS2_PLACEMENT_3D('',#48040,#26823,#26824);
#21815=AXIS2_PLACEMENT_3D('',#48046,#26828,#26829);
#21816=AXIS2_PLACEMENT_3D('',#48052,#26833,#26834);
#21817=AXIS2_PLACEMENT_3D('',#48055,#26837,#26838);
#21818=AXIS2_PLACEMENT_3D('',#48056,#26839,#26840);
#21819=AXIS2_PLACEMENT_3D('',#48057,#26841,#26842);
#21820=AXIS2_PLACEMENT_3D('',#48058,#26843,#26844);
#21821=AXIS2_PLACEMENT_3D('',#48060,#26845,#26846);
#21822=AXIS2_PLACEMENT_3D('',#48063,#26848,#26849);
#21823=AXIS2_PLACEMENT_3D('',#48064,#26850,#26851);
#21824=AXIS2_PLACEMENT_3D('',#48073,#26856,#26857);
#21825=AXIS2_PLACEMENT_3D('',#48079,#26861,#26862);
#21826=AXIS2_PLACEMENT_3D('',#48085,#26866,#26867);
#21827=AXIS2_PLACEMENT_3D('',#48088,#26870,#26871);
#21828=AXIS2_PLACEMENT_3D('',#48089,#26872,#26873);
#21829=AXIS2_PLACEMENT_3D('',#48090,#26874,#26875);
#21830=AXIS2_PLACEMENT_3D('',#48091,#26876,#26877);
#21831=AXIS2_PLACEMENT_3D('',#48093,#26878,#26879);
#21832=AXIS2_PLACEMENT_3D('',#48096,#26881,#26882);
#21833=AXIS2_PLACEMENT_3D('',#48097,#26883,#26884);
#21834=AXIS2_PLACEMENT_3D('',#48106,#26889,#26890);
#21835=AXIS2_PLACEMENT_3D('',#48112,#26894,#26895);
#21836=AXIS2_PLACEMENT_3D('',#48118,#26899,#26900);
#21837=AXIS2_PLACEMENT_3D('',#48121,#26903,#26904);
#21838=AXIS2_PLACEMENT_3D('',#48122,#26905,#26906);
#21839=AXIS2_PLACEMENT_3D('',#48123,#26907,#26908);
#21840=AXIS2_PLACEMENT_3D('',#48124,#26909,#26910);
#21841=AXIS2_PLACEMENT_3D('',#48133,#26915,#26916);
#21842=AXIS2_PLACEMENT_3D('',#48135,#26917,#26918);
#21843=AXIS2_PLACEMENT_3D('',#48138,#26920,#26921);
#21844=AXIS2_PLACEMENT_3D('',#48139,#26922,#26923);
#21845=AXIS2_PLACEMENT_3D('',#48141,#26924,#26925);
#21846=AXIS2_PLACEMENT_3D('',#48144,#26927,#26928);
#21847=AXIS2_PLACEMENT_3D('',#48145,#26929,#26930);
#21848=AXIS2_PLACEMENT_3D('',#48147,#26931,#26932);
#21849=AXIS2_PLACEMENT_3D('',#48150,#26934,#26935);
#21850=AXIS2_PLACEMENT_3D('',#48151,#26936,#26937);
#21851=AXIS2_PLACEMENT_3D('',#48157,#26941,#26942);
#21852=AXIS2_PLACEMENT_3D('',#48159,#26943,#26944);
#21853=AXIS2_PLACEMENT_3D('',#48162,#26946,#26947);
#21854=AXIS2_PLACEMENT_3D('',#48163,#26948,#26949);
#21855=AXIS2_PLACEMENT_3D('',#48165,#26950,#26951);
#21856=AXIS2_PLACEMENT_3D('',#48168,#26953,#26954);
#21857=AXIS2_PLACEMENT_3D('',#48169,#26955,#26956);
#21858=AXIS2_PLACEMENT_3D('',#48171,#26957,#26958);
#21859=AXIS2_PLACEMENT_3D('',#48174,#26960,#26961);
#21860=AXIS2_PLACEMENT_3D('',#48175,#26962,#26963);
#21861=AXIS2_PLACEMENT_3D('',#48181,#26967,#26968);
#21862=AXIS2_PLACEMENT_3D('',#48183,#26969,#26970);
#21863=AXIS2_PLACEMENT_3D('',#48186,#26972,#26973);
#21864=AXIS2_PLACEMENT_3D('',#48187,#26974,#26975);
#21865=AXIS2_PLACEMENT_3D('',#48193,#26979,#26980);
#21866=AXIS2_PLACEMENT_3D('',#48195,#26981,#26982);
#21867=AXIS2_PLACEMENT_3D('',#48198,#26984,#26985);
#21868=AXIS2_PLACEMENT_3D('',#48199,#26986,#26987);
#21869=AXIS2_PLACEMENT_3D('',#48205,#26991,#26992);
#21870=AXIS2_PLACEMENT_3D('',#48207,#26993,#26994);
#21871=AXIS2_PLACEMENT_3D('',#48210,#26996,#26997);
#21872=AXIS2_PLACEMENT_3D('',#48211,#26998,#26999);
#21873=AXIS2_PLACEMENT_3D('',#48217,#27003,#27004);
#21874=AXIS2_PLACEMENT_3D('',#48223,#27008,#27009);
#21875=AXIS2_PLACEMENT_3D('',#48229,#27012,#27013);
#21876=AXIS2_PLACEMENT_3D('',#48231,#27014,#27015);
#21877=AXIS2_PLACEMENT_3D('',#48233,#27016,#27017);
#21878=AXIS2_PLACEMENT_3D('',#48237,#27019,#27020);
#21879=AXIS2_PLACEMENT_3D('',#48239,#27021,#27022);
#21880=AXIS2_PLACEMENT_3D('',#48241,#27023,#27024);
#21881=AXIS2_PLACEMENT_3D('',#48245,#27026,#27027);
#21882=AXIS2_PLACEMENT_3D('',#48249,#27029,#27030);
#21883=AXIS2_PLACEMENT_3D('',#48253,#27032,#27033);
#21884=AXIS2_PLACEMENT_3D('',#48259,#27037,#27038);
#21885=AXIS2_PLACEMENT_3D('',#48265,#27042,#27043);
#21886=AXIS2_PLACEMENT_3D('',#48267,#27044,#27045);
#21887=AXIS2_PLACEMENT_3D('',#48269,#27047,#27048);
#21888=AXIS2_PLACEMENT_3D('',#48271,#27049,#27050);
#21889=AXIS2_PLACEMENT_3D('',#48273,#27052,#27053);
#21890=AXIS2_PLACEMENT_3D('',#48275,#27054,#27055);
#21891=AXIS2_PLACEMENT_3D('',#48277,#27057,#27058);
#21892=AXIS2_PLACEMENT_3D('',#48281,#27061,#27062);
#21893=AXIS2_PLACEMENT_3D('',#48283,#27063,#27064);
#21894=AXIS2_PLACEMENT_3D('',#48285,#27066,#27067);
#21895=AXIS2_PLACEMENT_3D('',#48287,#27068,#27069);
#21896=AXIS2_PLACEMENT_3D('',#48289,#27071,#27072);
#21897=AXIS2_PLACEMENT_3D('',#48291,#27073,#27074);
#21898=AXIS2_PLACEMENT_3D('',#48293,#27076,#27077);
#21899=AXIS2_PLACEMENT_3D('',#48297,#27080,#27081);
#21900=AXIS2_PLACEMENT_3D('',#48299,#27082,#27083);
#21901=AXIS2_PLACEMENT_3D('',#48301,#27085,#27086);
#21902=AXIS2_PLACEMENT_3D('',#48305,#27089,#27090);
#21903=AXIS2_PLACEMENT_3D('',#48307,#27091,#27092);
#21904=AXIS2_PLACEMENT_3D('',#48309,#27094,#27095);
#21905=AXIS2_PLACEMENT_3D('',#48313,#27098,#27099);
#21906=AXIS2_PLACEMENT_3D('',#48315,#27100,#27101);
#21907=AXIS2_PLACEMENT_3D('',#48317,#27103,#27104);
#21908=AXIS2_PLACEMENT_3D('',#48321,#27107,#27108);
#21909=AXIS2_PLACEMENT_3D('',#48325,#27111,#27112);
#21910=AXIS2_PLACEMENT_3D('',#48327,#27114,#27115);
#21911=AXIS2_PLACEMENT_3D('',#48329,#27117,#27118);
#21912=AXIS2_PLACEMENT_3D('',#48330,#27119,#27120);
#21913=AXIS2_PLACEMENT_3D('',#48331,#27121,#27122);
#21914=AXIS2_PLACEMENT_3D('',#48332,#27123,#27124);
#21915=AXIS2_PLACEMENT_3D('',#48333,#27125,#27126);
#21916=AXIS2_PLACEMENT_3D('',#48334,#27127,#27128);
#21917=AXIS2_PLACEMENT_3D('',#48335,#27129,#27130);
#21918=AXIS2_PLACEMENT_3D('',#48336,#27131,#27132);
#21919=AXIS2_PLACEMENT_3D('',#48337,#27133,#27134);
#21920=AXIS2_PLACEMENT_3D('',#48338,#27135,#27136);
#21921=AXIS2_PLACEMENT_3D('',#48339,#27137,#27138);
#21922=AXIS2_PLACEMENT_3D('',#48340,#27139,#27140);
#21923=AXIS2_PLACEMENT_3D('',#48341,#27141,#27142);
#21924=AXIS2_PLACEMENT_3D('',#48342,#27143,#27144);
#21925=AXIS2_PLACEMENT_3D('',#48343,#27145,#27146);
#21926=DIRECTION('axis',(0.,0.,1.));
#21927=DIRECTION('refdir',(1.,0.,0.));
#21928=DIRECTION('axis',(0.,0.,1.));
#21929=DIRECTION('refdir',(1.,0.,0.));
#21930=DIRECTION('center_axis',(0.,1.,0.));
#21931=DIRECTION('ref_axis',(1.,0.,0.));
#21932=DIRECTION('',(-1.60844785188215E-15,0.,1.));
#21933=DIRECTION('',(0.707106781186549,0.,0.707106781186546));
#21934=DIRECTION('',(1.,0.,1.55356845212375E-15));
#21935=DIRECTION('',(0.704727298913668,0.,-0.709478283082608));
#21936=DIRECTION('center_axis',(0.,1.,0.));
#21937=DIRECTION('ref_axis',(0.709478283082593,0.,0.704727298913683));
#21938=DIRECTION('',(0.,0.,-1.));
#21939=DIRECTION('center_axis',(0.,1.,0.));
#21940=DIRECTION('ref_axis',(1.,0.,0.));
#21941=DIRECTION('',(-0.702199901316075,0.,-0.711979844231348));
#21942=DIRECTION('center_axis',(0.,-1.,0.));
#21943=DIRECTION('ref_axis',(-0.951733868867053,0.,0.306924490471762));
#21944=DIRECTION('center_axis',(0.,1.,0.));
#21945=DIRECTION('ref_axis',(0.951733868867033,0.,-0.306924490471823));
#21946=DIRECTION('center_axis',(0.,-1.,0.));
#21947=DIRECTION('ref_axis',(-1.,0.,-1.48029736616691E-14));
#21948=DIRECTION('',(1.93287220490857E-14,0.,-1.));
#21949=DIRECTION('center_axis',(0.,-1.,0.));
#21950=DIRECTION('ref_axis',(-0.295138112194515,0.,-0.955454601082782));
#21951=DIRECTION('center_axis',(0.,1.,0.));
#21952=DIRECTION('ref_axis',(0.295138112194494,0.,0.955454601082788));
#21953=DIRECTION('center_axis',(0.,-1.,0.));
#21954=DIRECTION('ref_axis',(-0.710729249896308,0.,-0.703465658964126));
#21955=DIRECTION('',(0.703465658964212,0.,-0.710729249896223));
#21956=DIRECTION('',(1.,0.,6.14369354430926E-16));
#21957=DIRECTION('',(0.703465658964231,0.,0.710729249896204));
#21958=DIRECTION('center_axis',(0.,-1.,0.));
#21959=DIRECTION('ref_axis',(0.963381374692962,0.,-0.26813490428271));
#21960=DIRECTION('center_axis',(0.,1.,0.));
#21961=DIRECTION('ref_axis',(-0.963381374692976,0.,0.268134904282661));
#21962=DIRECTION('center_axis',(0.,-1.,0.));
#21963=DIRECTION('ref_axis',(1.,0.,0.));
#21964=DIRECTION('',(0.,0.,1.));
#21965=DIRECTION('center_axis',(0.,-1.,0.));
#21966=DIRECTION('ref_axis',(0.245760053518526,0.,0.969330694909932));
#21967=DIRECTION('center_axis',(0.,1.,0.));
#21968=DIRECTION('ref_axis',(-0.245760053518557,0.,-0.969330694909924));
#21969=DIRECTION('center_axis',(0.,-1.,0.));
#21970=DIRECTION('ref_axis',(0.711979844231347,0.,0.702199901316076));
#21971=DIRECTION('',(-0.702199901316085,0.,0.711979844231338));
#21972=DIRECTION('center_axis',(0.,1.,0.));
#21973=DIRECTION('ref_axis',(-0.711979844231317,0.,-0.702199901316106));
#21974=DIRECTION('',(1.18143967662125E-14,0.,1.));
#21975=DIRECTION('center_axis',(0.,1.,0.));
#21976=DIRECTION('ref_axis',(-1.,0.,-7.19001577852613E-14));
#21977=DIRECTION('',(0.70472729891367,0.,0.709478283082607));
#21978=DIRECTION('',(1.,0.,0.));
#21979=DIRECTION('',(0.707106781186549,0.,-0.707106781186546));
#21980=DIRECTION('',(0.,0.,-1.));
#21981=DIRECTION('',(-0.707106781186548,0.,-0.707106781186548));
#21982=DIRECTION('',(-1.,0.,0.));
#21983=DIRECTION('',(-0.707106781186551,0.,0.707106781186544));
#21984=DIRECTION('center_axis',(0.710729249896204,0.,-0.703465658964231));
#21985=DIRECTION('ref_axis',(0.703465658964231,0.,0.710729249896204));
#21986=DIRECTION('',(0.,-1.,0.));
#21987=DIRECTION('',(0.703465658964231,0.,0.710729249896204));
#21988=DIRECTION('',(0.,-1.,0.));
#21989=DIRECTION('center_axis',(0.,1.,0.));
#21990=DIRECTION('ref_axis',(0.963381374692962,0.,-0.26813490428271));
#21991=DIRECTION('center_axis',(0.,-1.,0.));
#21992=DIRECTION('ref_axis',(0.963381374692962,0.,-0.26813490428271));
#21993=DIRECTION('',(0.,-1.,0.));
#21994=DIRECTION('center_axis',(0.,1.,0.));
#21995=DIRECTION('ref_axis',(-0.963381374692976,0.,0.268134904282661));
#21996=DIRECTION('center_axis',(0.,1.,0.));
#21997=DIRECTION('ref_axis',(-0.963381374692976,0.,0.268134904282661));
#21998=DIRECTION('',(0.,-1.,0.));
#21999=DIRECTION('center_axis',(0.,1.,0.));
#22000=DIRECTION('ref_axis',(1.,0.,0.));
#22001=DIRECTION('center_axis',(0.,-1.,0.));
#22002=DIRECTION('ref_axis',(1.,0.,0.));
#22003=DIRECTION('',(0.,-1.,0.));
#22004=DIRECTION('center_axis',(1.,0.,0.));
#22005=DIRECTION('ref_axis',(0.,0.,1.));
#22006=DIRECTION('',(0.,0.,1.));
#22007=DIRECTION('',(0.,-1.,0.));
#22008=DIRECTION('center_axis',(0.,1.,0.));
#22009=DIRECTION('ref_axis',(0.245760053518526,0.,0.969330694909932));
#22010=DIRECTION('center_axis',(0.,-1.,0.));
#22011=DIRECTION('ref_axis',(0.245760053518526,0.,0.969330694909932));
#22012=DIRECTION('',(0.,-1.,0.));
#22013=DIRECTION('center_axis',(0.,1.,0.));
#22014=DIRECTION('ref_axis',(-0.245760053518557,0.,-0.969330694909924));
#22015=DIRECTION('center_axis',(0.,1.,0.));
#22016=DIRECTION('ref_axis',(-0.245760053518557,0.,-0.969330694909924));
#22017=DIRECTION('',(0.,-1.,0.));
#22018=DIRECTION('center_axis',(0.,1.,0.));
#22019=DIRECTION('ref_axis',(0.711979844231347,0.,0.702199901316076));
#22020=DIRECTION('center_axis',(0.,-1.,0.));
#22021=DIRECTION('ref_axis',(0.711979844231347,0.,0.702199901316076));
#22022=DIRECTION('',(0.,-1.,0.));
#22023=DIRECTION('center_axis',(0.711979844231338,0.,0.702199901316085));
#22024=DIRECTION('ref_axis',(-0.702199901316085,0.,0.711979844231338));
#22025=DIRECTION('',(-0.702199901316085,0.,0.711979844231338));
#22026=DIRECTION('',(0.,-1.,0.));
#22027=DIRECTION('center_axis',(0.,1.,0.));
#22028=DIRECTION('ref_axis',(-0.711979844231317,0.,-0.702199901316106));
#22029=DIRECTION('center_axis',(0.,1.,0.));
#22030=DIRECTION('ref_axis',(-0.711979844231317,0.,-0.702199901316106));
#22031=DIRECTION('',(0.,-1.,0.));
#22032=DIRECTION('center_axis',(1.,0.,-1.18143967662125E-14));
#22033=DIRECTION('ref_axis',(1.18143967662125E-14,0.,1.));
#22034=DIRECTION('',(1.18143967662125E-14,0.,1.));
#22035=DIRECTION('',(0.,-1.,0.));
#22036=DIRECTION('center_axis',(0.,1.,0.));
#22037=DIRECTION('ref_axis',(-1.,0.,-7.19001577852613E-14));
#22038=DIRECTION('center_axis',(0.,1.,0.));
#22039=DIRECTION('ref_axis',(-1.,0.,-7.19001577852613E-14));
#22040=DIRECTION('',(0.,-1.,0.));
#22041=DIRECTION('center_axis',(0.709478283082607,0.,-0.70472729891367));
#22042=DIRECTION('ref_axis',(0.70472729891367,0.,0.709478283082607));
#22043=DIRECTION('',(0.70472729891367,0.,0.709478283082607));
#22044=DIRECTION('',(0.,-1.,0.));
#22045=DIRECTION('center_axis',(0.,0.,-1.));
#22046=DIRECTION('ref_axis',(1.,0.,0.));
#22047=DIRECTION('',(1.,0.,0.));
#22048=DIRECTION('',(0.,-1.,0.));
#22049=DIRECTION('center_axis',(-0.707106781186546,0.,-0.707106781186549));
#22050=DIRECTION('ref_axis',(0.707106781186549,0.,-0.707106781186546));
#22051=DIRECTION('',(0.707106781186549,0.,-0.707106781186546));
#22052=DIRECTION('',(0.,-1.,0.));
#22053=DIRECTION('center_axis',(-1.,0.,0.));
#22054=DIRECTION('ref_axis',(0.,0.,-1.));
#22055=DIRECTION('',(0.,0.,-1.));
#22056=DIRECTION('',(0.,-1.,0.));
#22057=DIRECTION('center_axis',(1.,0.,1.60844785188215E-15));
#22058=DIRECTION('ref_axis',(-1.60844785188215E-15,0.,1.));
#22059=DIRECTION('',(0.,-1.,0.));
#22060=DIRECTION('',(-1.60844785188215E-15,0.,1.));
#22061=DIRECTION('',(0.,-1.,0.));
#22062=DIRECTION('center_axis',(0.707106781186546,0.,-0.707106781186549));
#22063=DIRECTION('ref_axis',(0.707106781186549,0.,0.707106781186546));
#22064=DIRECTION('',(0.707106781186549,0.,0.707106781186546));
#22065=DIRECTION('',(0.,-1.,0.));
#22066=DIRECTION('center_axis',(1.55356845212375E-15,0.,-1.));
#22067=DIRECTION('ref_axis',(1.,0.,1.55356845212375E-15));
#22068=DIRECTION('',(1.,0.,1.55356845212375E-15));
#22069=DIRECTION('',(0.,-1.,0.));
#22070=DIRECTION('center_axis',(-0.709478283082608,0.,-0.704727298913668));
#22071=DIRECTION('ref_axis',(0.704727298913668,0.,-0.709478283082608));
#22072=DIRECTION('',(0.704727298913668,0.,-0.709478283082608));
#22073=DIRECTION('',(0.,-1.,0.));
#22074=DIRECTION('center_axis',(0.,1.,0.));
#22075=DIRECTION('ref_axis',(0.709478283082593,0.,0.704727298913683));
#22076=DIRECTION('center_axis',(0.,1.,0.));
#22077=DIRECTION('ref_axis',(0.709478283082593,0.,0.704727298913683));
#22078=DIRECTION('',(0.,-1.,0.));
#22079=DIRECTION('center_axis',(-0.707106781186548,0.,0.707106781186548));
#22080=DIRECTION('ref_axis',(-0.707106781186548,0.,-0.707106781186548));
#22081=DIRECTION('',(-0.707106781186548,0.,-0.707106781186548));
#22082=DIRECTION('',(0.,-1.,0.));
#22083=DIRECTION('center_axis',(0.,0.,1.));
#22084=DIRECTION('ref_axis',(-1.,0.,0.));
#22085=DIRECTION('',(-1.,0.,0.));
#22086=DIRECTION('',(0.,-1.,0.));
#22087=DIRECTION('center_axis',(0.707106781186544,0.,0.707106781186551));
#22088=DIRECTION('ref_axis',(-0.707106781186551,0.,0.707106781186544));
#22089=DIRECTION('',(-0.707106781186551,0.,0.707106781186544));
#22090=DIRECTION('center_axis',(-1.,0.,0.));
#22091=DIRECTION('ref_axis',(0.,0.,-1.));
#22092=DIRECTION('',(0.,0.,-1.));
#22093=DIRECTION('',(0.,1.,0.));
#22094=DIRECTION('center_axis',(6.14369354430926E-16,0.,-1.));
#22095=DIRECTION('ref_axis',(1.,0.,6.14369354430926E-16));
#22096=DIRECTION('',(0.,-1.,0.));
#22097=DIRECTION('',(1.,0.,6.14369354430926E-16));
#22098=DIRECTION('center_axis',(-0.710729249896223,0.,-0.703465658964212));
#22099=DIRECTION('ref_axis',(0.703465658964212,0.,-0.710729249896223));
#22100=DIRECTION('',(0.,-1.,0.));
#22101=DIRECTION('',(0.703465658964212,0.,-0.710729249896223));
#22102=DIRECTION('center_axis',(0.,1.,0.));
#22103=DIRECTION('ref_axis',(-0.710729249896308,0.,-0.703465658964126));
#22104=DIRECTION('',(0.,-1.,0.));
#22105=DIRECTION('center_axis',(0.,-1.,0.));
#22106=DIRECTION('ref_axis',(-0.710729249896308,0.,-0.703465658964126));
#22107=DIRECTION('center_axis',(0.,1.,0.));
#22108=DIRECTION('ref_axis',(0.295138112194494,0.,0.955454601082788));
#22109=DIRECTION('',(0.,-1.,0.));
#22110=DIRECTION('center_axis',(0.,1.,0.));
#22111=DIRECTION('ref_axis',(0.295138112194494,0.,0.955454601082788));
#22112=DIRECTION('center_axis',(0.,1.,0.));
#22113=DIRECTION('ref_axis',(-0.295138112194515,0.,-0.955454601082782));
#22114=DIRECTION('',(0.,-1.,0.));
#22115=DIRECTION('center_axis',(0.,-1.,0.));
#22116=DIRECTION('ref_axis',(-0.295138112194515,0.,-0.955454601082782));
#22117=DIRECTION('center_axis',(-1.,0.,-1.93287220490857E-14));
#22118=DIRECTION('ref_axis',(1.93287220490857E-14,0.,-1.));
#22119=DIRECTION('',(0.,-1.,0.));
#22120=DIRECTION('',(1.93287220490857E-14,0.,-1.));
#22121=DIRECTION('center_axis',(0.,1.,0.));
#22122=DIRECTION('ref_axis',(-1.,0.,-1.48029736616691E-14));
#22123=DIRECTION('',(0.,-1.,0.));
#22124=DIRECTION('center_axis',(0.,-1.,0.));
#22125=DIRECTION('ref_axis',(-1.,0.,-1.48029736616691E-14));
#22126=DIRECTION('center_axis',(0.,1.,0.));
#22127=DIRECTION('ref_axis',(0.951733868867033,0.,-0.306924490471823));
#22128=DIRECTION('',(0.,-1.,0.));
#22129=DIRECTION('center_axis',(0.,1.,0.));
#22130=DIRECTION('ref_axis',(0.951733868867033,0.,-0.306924490471823));
#22131=DIRECTION('center_axis',(0.,1.,0.));
#22132=DIRECTION('ref_axis',(-0.951733868867053,0.,0.306924490471762));
#22133=DIRECTION('',(0.,-1.,0.));
#22134=DIRECTION('center_axis',(0.,-1.,0.));
#22135=DIRECTION('ref_axis',(-0.951733868867053,0.,0.306924490471762));
#22136=DIRECTION('center_axis',(-0.711979844231348,0.,0.702199901316075));
#22137=DIRECTION('ref_axis',(-0.702199901316075,0.,-0.711979844231348));
#22138=DIRECTION('',(0.,-1.,0.));
#22139=DIRECTION('',(-0.702199901316075,0.,-0.711979844231348));
#22140=DIRECTION('center_axis',(0.,1.,0.));
#22141=DIRECTION('ref_axis',(1.,0.,0.));
#22142=DIRECTION('center_axis',(0.,1.,0.));
#22143=DIRECTION('ref_axis',(1.,0.,0.));
#22144=DIRECTION('center_axis',(0.,1.,0.));
#22145=DIRECTION('ref_axis',(-1.,0.,0.));
#22146=DIRECTION('center_axis',(0.710729249896204,0.,-0.703465658964231));
#22147=DIRECTION('ref_axis',(0.703465658964231,0.,0.710729249896204));
#22148=DIRECTION('',(0.703465658964231,0.,0.710729249896204));
#22149=DIRECTION('',(0.,-1.,0.));
#22150=DIRECTION('',(0.703465658964231,0.,0.710729249896204));
#22151=DIRECTION('',(0.,-1.,0.));
#22152=DIRECTION('center_axis',(0.,1.,0.));
#22153=DIRECTION('ref_axis',(0.963381374692962,0.,-0.26813490428271));
#22154=DIRECTION('center_axis',(0.,-1.,0.));
#22155=DIRECTION('ref_axis',(0.963381374692962,0.,-0.26813490428271));
#22156=DIRECTION('',(0.,-1.,0.));
#22157=DIRECTION('center_axis',(0.,-1.,0.));
#22158=DIRECTION('ref_axis',(0.963381374692962,0.,-0.26813490428271));
#22159=DIRECTION('center_axis',(0.,1.,0.));
#22160=DIRECTION('ref_axis',(-0.963381374692976,0.,0.268134904282661));
#22161=DIRECTION('center_axis',(0.,1.,0.));
#22162=DIRECTION('ref_axis',(-0.963381374692976,0.,0.268134904282661));
#22163=DIRECTION('',(0.,-1.,0.));
#22164=DIRECTION('center_axis',(0.,1.,0.));
#22165=DIRECTION('ref_axis',(-0.963381374692976,0.,0.268134904282661));
#22166=DIRECTION('center_axis',(0.,1.,0.));
#22167=DIRECTION('ref_axis',(1.,0.,0.));
#22168=DIRECTION('center_axis',(0.,-1.,0.));
#22169=DIRECTION('ref_axis',(1.,0.,0.));
#22170=DIRECTION('',(0.,-1.,0.));
#22171=DIRECTION('center_axis',(0.,-1.,0.));
#22172=DIRECTION('ref_axis',(1.,0.,0.));
#22173=DIRECTION('center_axis',(1.,0.,0.));
#22174=DIRECTION('ref_axis',(0.,0.,1.));
#22175=DIRECTION('',(0.,0.,1.));
#22176=DIRECTION('',(0.,-1.,0.));
#22177=DIRECTION('',(0.,0.,1.));
#22178=DIRECTION('center_axis',(0.,1.,0.));
#22179=DIRECTION('ref_axis',(0.245760053518526,0.,0.969330694909932));
#22180=DIRECTION('center_axis',(0.,-1.,0.));
#22181=DIRECTION('ref_axis',(0.245760053518526,0.,0.969330694909932));
#22182=DIRECTION('',(0.,-1.,0.));
#22183=DIRECTION('center_axis',(0.,-1.,0.));
#22184=DIRECTION('ref_axis',(0.245760053518526,0.,0.969330694909932));
#22185=DIRECTION('center_axis',(0.,1.,0.));
#22186=DIRECTION('ref_axis',(-0.245760053518557,0.,-0.969330694909924));
#22187=DIRECTION('center_axis',(0.,1.,0.));
#22188=DIRECTION('ref_axis',(-0.245760053518557,0.,-0.969330694909924));
#22189=DIRECTION('',(0.,-1.,0.));
#22190=DIRECTION('center_axis',(0.,1.,0.));
#22191=DIRECTION('ref_axis',(-0.245760053518557,0.,-0.969330694909924));
#22192=DIRECTION('center_axis',(0.,1.,0.));
#22193=DIRECTION('ref_axis',(-1.,0.,0.));
#22194=DIRECTION('',(0.707106781186554,0.,-0.707106781186541));
#22195=DIRECTION('',(0.,0.,-1.));
#22196=DIRECTION('',(0.707106781186549,0.,-0.707106781186546));
#22197=DIRECTION('',(1.,0.,0.));
#22198=DIRECTION('',(0.70472729891367,0.,0.709478283082607));
#22199=DIRECTION('center_axis',(0.,1.,0.));
#22200=DIRECTION('ref_axis',(-1.,0.,-7.19001577852613E-14));
#22201=DIRECTION('',(1.18143967662125E-14,0.,1.));
#22202=DIRECTION('center_axis',(0.,1.,0.));
#22203=DIRECTION('ref_axis',(-0.711979844231317,0.,-0.702199901316106));
#22204=DIRECTION('',(-0.702199901316085,0.,0.711979844231338));
#22205=DIRECTION('center_axis',(0.,-1.,0.));
#22206=DIRECTION('ref_axis',(0.711979844231347,0.,0.702199901316076));
#22207=DIRECTION('',(1.,0.,6.14369354430926E-16));
#22208=DIRECTION('',(0.703465658964212,0.,-0.710729249896223));
#22209=DIRECTION('center_axis',(0.,-1.,0.));
#22210=DIRECTION('ref_axis',(-0.710729249896308,0.,-0.703465658964126));
#22211=DIRECTION('center_axis',(0.,1.,0.));
#22212=DIRECTION('ref_axis',(0.295138112194494,0.,0.955454601082788));
#22213=DIRECTION('center_axis',(0.,-1.,0.));
#22214=DIRECTION('ref_axis',(-0.295138112194515,0.,-0.955454601082782));
#22215=DIRECTION('',(1.93287220490857E-14,0.,-1.));
#22216=DIRECTION('center_axis',(0.,-1.,0.));
#22217=DIRECTION('ref_axis',(-1.,0.,-1.48029736616691E-14));
#22218=DIRECTION('center_axis',(0.,1.,0.));
#22219=DIRECTION('ref_axis',(0.951733868867033,0.,-0.306924490471823));
#22220=DIRECTION('center_axis',(0.,-1.,0.));
#22221=DIRECTION('ref_axis',(-0.951733868867053,0.,0.306924490471762));
#22222=DIRECTION('',(-0.702199901316075,0.,-0.711979844231348));
#22223=DIRECTION('center_axis',(0.,1.,0.));
#22224=DIRECTION('ref_axis',(1.,0.,0.));
#22225=DIRECTION('',(0.,0.,-1.));
#22226=DIRECTION('center_axis',(0.,1.,0.));
#22227=DIRECTION('ref_axis',(0.709478283082593,0.,0.704727298913683));
#22228=DIRECTION('',(0.704727298913668,0.,-0.709478283082608));
#22229=DIRECTION('',(1.,0.,1.55356845212375E-15));
#22230=DIRECTION('',(0.707106781186549,0.,0.707106781186546));
#22231=DIRECTION('',(-1.60844785188215E-15,0.,1.));
#22232=DIRECTION('',(-0.707106781186556,0.,-0.707106781186539));
#22233=DIRECTION('',(-2.63040290597841E-15,0.,-1.));
#22234=DIRECTION('',(0.707106781186546,0.,-0.707106781186549));
#22235=DIRECTION('',(1.,0.,-2.63040290597841E-15));
#22236=DIRECTION('center_axis',(0.,1.,0.));
#22237=DIRECTION('ref_axis',(-1.37675000001205E-14,0.,1.));
#22238=DIRECTION('',(-1.,0.,0.));
#22239=DIRECTION('center_axis',(0.,-1.,0.));
#22240=DIRECTION('ref_axis',(1.63979029060989E-14,0.,1.));
#22241=DIRECTION('',(-1.,0.,0.));
#22242=DIRECTION('',(-0.707106781186548,0.,-0.707106781186548));
#22243=DIRECTION('',(0.,0.,-1.));
#22244=DIRECTION('center_axis',(-0.707106781186541,0.,-0.707106781186554));
#22245=DIRECTION('ref_axis',(0.707106781186554,0.,-0.707106781186541));
#22246=DIRECTION('',(0.,-1.,0.));
#22247=DIRECTION('',(-0.707106781186554,0.,0.707106781186541));
#22248=DIRECTION('',(0.,-1.,0.));
#22249=DIRECTION('center_axis',(-1.,0.,0.));
#22250=DIRECTION('ref_axis',(0.,0.,-1.));
#22251=DIRECTION('',(0.,-1.,0.));
#22252=DIRECTION('',(0.,0.,1.));
#22253=DIRECTION('center_axis',(-0.707106781186548,0.,0.707106781186548));
#22254=DIRECTION('ref_axis',(-0.707106781186548,0.,-0.707106781186548));
#22255=DIRECTION('',(0.,-1.,0.));
#22256=DIRECTION('',(0.707106781186548,0.,0.707106781186548));
#22257=DIRECTION('center_axis',(0.,0.,1.));
#22258=DIRECTION('ref_axis',(-1.,0.,0.));
#22259=DIRECTION('',(0.,-1.,0.));
#22260=DIRECTION('',(1.,0.,0.));
#22261=DIRECTION('center_axis',(0.,0.,-1.));
#22262=DIRECTION('ref_axis',(-1.,0.,0.));
#22263=DIRECTION('center_axis',(0.,0.,-1.));
#22264=DIRECTION('ref_axis',(-1.,0.,0.));
#22265=DIRECTION('center_axis',(0.,1.,0.));
#22266=DIRECTION('ref_axis',(1.63979029060989E-14,0.,1.));
#22267=DIRECTION('',(0.,-1.,0.));
#22268=DIRECTION('center_axis',(0.,1.,0.));
#22269=DIRECTION('ref_axis',(1.63979029060989E-14,0.,1.));
#22270=DIRECTION('center_axis',(0.,0.,1.));
#22271=DIRECTION('ref_axis',(-1.,0.,0.));
#22272=DIRECTION('',(0.,-1.,0.));
#22273=DIRECTION('',(-1.,0.,2.63040290597841E-15));
#22274=DIRECTION('center_axis',(0.,1.,0.));
#22275=DIRECTION('ref_axis',(-1.,0.,0.));
#22276=DIRECTION('center_axis',(0.,-1.,0.));
#22277=DIRECTION('ref_axis',(-1.37675000001205E-14,0.,1.));
#22278=DIRECTION('',(-1.,0.,2.63040290597841E-15));
#22279=DIRECTION('',(-0.707106781186546,0.,0.707106781186549));
#22280=DIRECTION('',(2.63040290597841E-15,0.,1.));
#22281=DIRECTION('',(0.707106781186556,0.,0.707106781186539));
#22282=DIRECTION('',(-1.60844785188215E-15,0.,1.));
#22283=DIRECTION('',(0.707106781186549,0.,0.707106781186546));
#22284=DIRECTION('',(1.,0.,1.55356845212375E-15));
#22285=DIRECTION('',(0.704727298913668,0.,-0.709478283082608));
#22286=DIRECTION('center_axis',(0.,1.,0.));
#22287=DIRECTION('ref_axis',(0.709478283082593,0.,0.704727298913683));
#22288=DIRECTION('',(0.,0.,-1.));
#22289=DIRECTION('center_axis',(0.,1.,0.));
#22290=DIRECTION('ref_axis',(1.,0.,0.));
#22291=DIRECTION('',(-0.702199901316075,0.,-0.711979844231348));
#22292=DIRECTION('center_axis',(0.,-1.,0.));
#22293=DIRECTION('ref_axis',(-0.951733868867053,0.,0.306924490471762));
#22294=DIRECTION('center_axis',(0.,1.,0.));
#22295=DIRECTION('ref_axis',(0.951733868867033,0.,-0.306924490471823));
#22296=DIRECTION('center_axis',(0.,-1.,0.));
#22297=DIRECTION('ref_axis',(-1.,0.,-1.48029736616691E-14));
#22298=DIRECTION('',(1.93287220490857E-14,0.,-1.));
#22299=DIRECTION('center_axis',(0.,-1.,0.));
#22300=DIRECTION('ref_axis',(-0.295138112194515,0.,-0.955454601082782));
#22301=DIRECTION('center_axis',(0.,1.,0.));
#22302=DIRECTION('ref_axis',(0.295138112194494,0.,0.955454601082788));
#22303=DIRECTION('center_axis',(0.,-1.,0.));
#22304=DIRECTION('ref_axis',(-0.710729249896308,0.,-0.703465658964126));
#22305=DIRECTION('',(0.703465658964212,0.,-0.710729249896223));
#22306=DIRECTION('',(1.,0.,6.14369354430926E-16));
#22307=DIRECTION('center_axis',(0.,-1.,0.));
#22308=DIRECTION('ref_axis',(0.711979844231347,0.,0.702199901316076));
#22309=DIRECTION('',(-0.702199901316085,0.,0.711979844231338));
#22310=DIRECTION('center_axis',(0.,1.,0.));
#22311=DIRECTION('ref_axis',(-0.711979844231317,0.,-0.702199901316106));
#22312=DIRECTION('',(1.18143967662125E-14,0.,1.));
#22313=DIRECTION('center_axis',(0.,1.,0.));
#22314=DIRECTION('ref_axis',(-1.,0.,-7.19001577852613E-14));
#22315=DIRECTION('',(0.70472729891367,0.,0.709478283082607));
#22316=DIRECTION('',(1.,0.,0.));
#22317=DIRECTION('',(0.707106781186549,0.,-0.707106781186546));
#22318=DIRECTION('',(0.,0.,-1.));
#22319=DIRECTION('center_axis',(-0.707106781186539,0.,0.707106781186556));
#22320=DIRECTION('ref_axis',(-0.707106781186556,0.,-0.707106781186539));
#22321=DIRECTION('',(0.,-1.,0.));
#22322=DIRECTION('',(0.,1.,0.));
#22323=DIRECTION('center_axis',(-1.,0.,2.63040290597841E-15));
#22324=DIRECTION('ref_axis',(-2.63040290597841E-15,0.,-1.));
#22325=DIRECTION('',(0.,-1.,0.));
#22326=DIRECTION('center_axis',(-0.707106781186549,0.,-0.707106781186546));
#22327=DIRECTION('ref_axis',(0.707106781186546,0.,-0.707106781186549));
#22328=DIRECTION('',(0.,-1.,0.));
#22329=DIRECTION('center_axis',(-2.63040290597841E-15,0.,-1.));
#22330=DIRECTION('ref_axis',(1.,0.,-2.63040290597841E-15));
#22331=DIRECTION('',(0.,-1.,0.));
#22332=DIRECTION('center_axis',(-2.63040290597841E-15,0.,-1.));
#22333=DIRECTION('ref_axis',(-1.,0.,0.));
#22334=DIRECTION('center_axis',(-2.63040290597841E-15,0.,-1.));
#22335=DIRECTION('ref_axis',(-1.,0.,0.));
#22336=DIRECTION('center_axis',(0.,-1.,0.));
#22337=DIRECTION('ref_axis',(-1.37675000001205E-14,0.,1.));
#22338=DIRECTION('center_axis',(0.,0.,-1.));
#22339=DIRECTION('ref_axis',(-1.,0.,0.));
#22340=DIRECTION('',(0.,0.,1.));
#22341=DIRECTION('center_axis',(0.,0.,1.));
#22342=DIRECTION('ref_axis',(-1.,0.,0.));
#22343=DIRECTION('center_axis',(0.,0.,-1.));
#22344=DIRECTION('ref_axis',(-1.,0.,0.));
#22345=DIRECTION('',(0.,0.,1.));
#22346=DIRECTION('center_axis',(-1.55356845212375E-15,0.,1.));
#22347=DIRECTION('ref_axis',(-1.,0.,0.));
#22348=DIRECTION('center_axis',(0.,0.,-1.));
#22349=DIRECTION('ref_axis',(-1.,0.,0.));
#22350=DIRECTION('',(0.,0.,1.));
#22351=DIRECTION('center_axis',(0.,0.,1.));
#22352=DIRECTION('ref_axis',(-1.,0.,0.));
#22353=DIRECTION('center_axis',(0.,0.,-1.));
#22354=DIRECTION('ref_axis',(-1.,0.,0.));
#22355=DIRECTION('',(0.,0.,1.));
#22356=DIRECTION('center_axis',(-1.55356845212375E-15,0.,1.));
#22357=DIRECTION('ref_axis',(-1.,0.,0.));
#22358=DIRECTION('center_axis',(-1.,0.,0.));
#22359=DIRECTION('ref_axis',(0.,0.,-1.));
#22360=DIRECTION('',(0.,-1.,0.));
#22361=DIRECTION('center_axis',(-0.707106781186546,0.,-0.707106781186549));
#22362=DIRECTION('ref_axis',(0.707106781186549,0.,-0.707106781186546));
#22363=DIRECTION('',(0.,-1.,0.));
#22364=DIRECTION('center_axis',(0.,0.,-1.));
#22365=DIRECTION('ref_axis',(1.,0.,0.));
#22366=DIRECTION('',(0.,-1.,0.));
#22367=DIRECTION('center_axis',(0.709478283082607,0.,-0.70472729891367));
#22368=DIRECTION('ref_axis',(0.70472729891367,0.,0.709478283082607));
#22369=DIRECTION('',(0.,-1.,0.));
#22370=DIRECTION('center_axis',(0.,1.,0.));
#22371=DIRECTION('ref_axis',(-1.,0.,-7.19001577852613E-14));
#22372=DIRECTION('',(0.,-1.,0.));
#22373=DIRECTION('center_axis',(1.,0.,-1.18143967662125E-14));
#22374=DIRECTION('ref_axis',(1.18143967662125E-14,0.,1.));
#22375=DIRECTION('',(0.,-1.,0.));
#22376=DIRECTION('center_axis',(0.,1.,0.));
#22377=DIRECTION('ref_axis',(-0.711979844231317,0.,-0.702199901316106));
#22378=DIRECTION('',(0.,-1.,0.));
#22379=DIRECTION('center_axis',(0.711979844231338,0.,0.702199901316085));
#22380=DIRECTION('ref_axis',(-0.702199901316085,0.,0.711979844231338));
#22381=DIRECTION('',(0.,-1.,0.));
#22382=DIRECTION('center_axis',(0.,1.,0.));
#22383=DIRECTION('ref_axis',(0.711979844231347,0.,0.702199901316076));
#22384=DIRECTION('center_axis',(1.,0.,1.60844785188215E-15));
#22385=DIRECTION('ref_axis',(-1.60844785188215E-15,0.,1.));
#22386=DIRECTION('',(0.,-1.,0.));
#22387=DIRECTION('center_axis',(0.707106781186546,0.,-0.707106781186549));
#22388=DIRECTION('ref_axis',(0.707106781186549,0.,0.707106781186546));
#22389=DIRECTION('',(0.,-1.,0.));
#22390=DIRECTION('center_axis',(1.55356845212375E-15,0.,-1.));
#22391=DIRECTION('ref_axis',(1.,0.,1.55356845212375E-15));
#22392=DIRECTION('',(0.,-1.,0.));
#22393=DIRECTION('center_axis',(-0.709478283082608,0.,-0.704727298913668));
#22394=DIRECTION('ref_axis',(0.704727298913668,0.,-0.709478283082608));
#22395=DIRECTION('',(0.,-1.,0.));
#22396=DIRECTION('center_axis',(0.,1.,0.));
#22397=DIRECTION('ref_axis',(0.709478283082593,0.,0.704727298913683));
#22398=DIRECTION('',(0.,-1.,0.));
#22399=DIRECTION('center_axis',(-1.,0.,0.));
#22400=DIRECTION('ref_axis',(0.,0.,-1.));
#22401=DIRECTION('',(0.,1.,0.));
#22402=DIRECTION('center_axis',(0.,1.,0.));
#22403=DIRECTION('ref_axis',(1.,0.,0.));
#22404=DIRECTION('',(0.,-1.,0.));
#22405=DIRECTION('center_axis',(-0.711979844231348,0.,0.702199901316075));
#22406=DIRECTION('ref_axis',(-0.702199901316075,0.,-0.711979844231348));
#22407=DIRECTION('',(0.,-1.,0.));
#22408=DIRECTION('center_axis',(0.,1.,0.));
#22409=DIRECTION('ref_axis',(-0.951733868867053,0.,0.306924490471762));
#22410=DIRECTION('',(0.,-1.,0.));
#22411=DIRECTION('center_axis',(0.,1.,0.));
#22412=DIRECTION('ref_axis',(0.951733868867033,0.,-0.306924490471823));
#22413=DIRECTION('',(0.,-1.,0.));
#22414=DIRECTION('center_axis',(0.,1.,0.));
#22415=DIRECTION('ref_axis',(-1.,0.,-1.48029736616691E-14));
#22416=DIRECTION('',(0.,-1.,0.));
#22417=DIRECTION('center_axis',(-1.,0.,-1.93287220490857E-14));
#22418=DIRECTION('ref_axis',(1.93287220490857E-14,0.,-1.));
#22419=DIRECTION('',(0.,-1.,0.));
#22420=DIRECTION('center_axis',(0.,1.,0.));
#22421=DIRECTION('ref_axis',(-0.295138112194515,0.,-0.955454601082782));
#22422=DIRECTION('',(0.,-1.,0.));
#22423=DIRECTION('center_axis',(0.,1.,0.));
#22424=DIRECTION('ref_axis',(0.295138112194494,0.,0.955454601082788));
#22425=DIRECTION('',(0.,-1.,0.));
#22426=DIRECTION('center_axis',(0.,1.,0.));
#22427=DIRECTION('ref_axis',(-0.710729249896308,0.,-0.703465658964126));
#22428=DIRECTION('',(0.,-1.,0.));
#22429=DIRECTION('center_axis',(-0.710729249896223,0.,-0.703465658964212));
#22430=DIRECTION('ref_axis',(0.703465658964212,0.,-0.710729249896223));
#22431=DIRECTION('',(0.,-1.,0.));
#22432=DIRECTION('center_axis',(6.14369354430926E-16,0.,-1.));
#22433=DIRECTION('ref_axis',(1.,0.,6.14369354430926E-16));
#22434=DIRECTION('center_axis',(0.,1.,0.));
#22435=DIRECTION('ref_axis',(0.711979844231347,0.,0.702199901316076));
#22436=DIRECTION('center_axis',(0.,-1.,0.));
#22437=DIRECTION('ref_axis',(0.711979844231347,0.,0.702199901316076));
#22438=DIRECTION('',(0.,-1.,0.));
#22439=DIRECTION('center_axis',(0.,1.,0.));
#22440=DIRECTION('ref_axis',(0.711979844231347,0.,0.702199901316076));
#22441=DIRECTION('',(0.,-1.,0.));
#22442=DIRECTION('center_axis',(0.711979844231338,0.,0.702199901316085));
#22443=DIRECTION('ref_axis',(-0.702199901316085,0.,0.711979844231338));
#22444=DIRECTION('',(-0.702199901316085,0.,0.711979844231338));
#22445=DIRECTION('',(0.,-1.,0.));
#22446=DIRECTION('',(0.702199901316085,0.,-0.711979844231338));
#22447=DIRECTION('center_axis',(0.,1.,0.));
#22448=DIRECTION('ref_axis',(-0.711979844231317,0.,-0.702199901316106));
#22449=DIRECTION('center_axis',(0.,1.,0.));
#22450=DIRECTION('ref_axis',(-0.711979844231317,0.,-0.702199901316106));
#22451=DIRECTION('',(0.,-1.,0.));
#22452=DIRECTION('center_axis',(0.,-1.,0.));
#22453=DIRECTION('ref_axis',(-0.711979844231317,0.,-0.702199901316106));
#22454=DIRECTION('center_axis',(1.,0.,-1.18143967662125E-14));
#22455=DIRECTION('ref_axis',(1.18143967662125E-14,0.,1.));
#22456=DIRECTION('',(1.18143967662125E-14,0.,1.));
#22457=DIRECTION('',(0.,-1.,0.));
#22458=DIRECTION('',(-1.18143967662125E-14,0.,-1.));
#22459=DIRECTION('center_axis',(0.,1.,0.));
#22460=DIRECTION('ref_axis',(-1.,0.,-7.19001577852613E-14));
#22461=DIRECTION('center_axis',(0.,1.,0.));
#22462=DIRECTION('ref_axis',(-1.,0.,-7.19001577852613E-14));
#22463=DIRECTION('',(0.,-1.,0.));
#22464=DIRECTION('center_axis',(0.,-1.,0.));
#22465=DIRECTION('ref_axis',(-1.,0.,-7.19001577852613E-14));
#22466=DIRECTION('center_axis',(0.709478283082607,0.,-0.70472729891367));
#22467=DIRECTION('ref_axis',(0.70472729891367,0.,0.709478283082607));
#22468=DIRECTION('',(0.70472729891367,0.,0.709478283082607));
#22469=DIRECTION('',(0.,-1.,0.));
#22470=DIRECTION('',(-0.70472729891367,0.,-0.709478283082607));
#22471=DIRECTION('center_axis',(0.,0.,-1.));
#22472=DIRECTION('ref_axis',(1.,0.,0.));
#22473=DIRECTION('',(1.,0.,0.));
#22474=DIRECTION('',(0.,-1.,0.));
#22475=DIRECTION('',(-1.,0.,0.));
#22476=DIRECTION('center_axis',(-0.707106781186546,0.,-0.707106781186549));
#22477=DIRECTION('ref_axis',(0.707106781186549,0.,-0.707106781186546));
#22478=DIRECTION('',(0.707106781186549,0.,-0.707106781186546));
#22479=DIRECTION('',(0.,-1.,0.));
#22480=DIRECTION('',(-0.707106781186549,0.,0.707106781186546));
#22481=DIRECTION('center_axis',(-0.707106781186548,0.,0.707106781186548));
#22482=DIRECTION('ref_axis',(-0.707106781186548,0.,-0.707106781186548));
#22483=DIRECTION('',(0.707106781186548,0.,0.707106781186548));
#22484=DIRECTION('',(0.,-1.,0.));
#22485=DIRECTION('',(0.707106781186548,0.,0.707106781186548));
#22486=DIRECTION('',(0.,-1.,0.));
#22487=DIRECTION('center_axis',(0.,0.,1.));
#22488=DIRECTION('ref_axis',(-1.,0.,0.));
#22489=DIRECTION('',(1.,0.,0.));
#22490=DIRECTION('',(0.,-1.,0.));
#22491=DIRECTION('',(1.,0.,0.));
#22492=DIRECTION('center_axis',(0.707106781186544,0.,0.707106781186551));
#22493=DIRECTION('ref_axis',(-0.707106781186551,0.,0.707106781186544));
#22494=DIRECTION('',(0.707106781186551,0.,-0.707106781186544));
#22495=DIRECTION('',(0.,-1.,0.));
#22496=DIRECTION('',(0.707106781186551,0.,-0.707106781186544));
#22497=DIRECTION('center_axis',(1.,0.,1.60844785188215E-15));
#22498=DIRECTION('ref_axis',(-1.60844785188215E-15,0.,1.));
#22499=DIRECTION('',(-1.60844785188215E-15,0.,1.));
#22500=DIRECTION('',(0.,-1.,0.));
#22501=DIRECTION('',(1.60844785188215E-15,0.,-1.));
#22502=DIRECTION('center_axis',(0.707106781186546,0.,-0.707106781186549));
#22503=DIRECTION('ref_axis',(0.707106781186549,0.,0.707106781186546));
#22504=DIRECTION('',(0.707106781186549,0.,0.707106781186546));
#22505=DIRECTION('',(0.,-1.,0.));
#22506=DIRECTION('',(-0.707106781186549,0.,-0.707106781186546));
#22507=DIRECTION('center_axis',(1.55356845212375E-15,0.,-1.));
#22508=DIRECTION('ref_axis',(1.,0.,1.55356845212375E-15));
#22509=DIRECTION('',(1.,0.,1.55356845212375E-15));
#22510=DIRECTION('',(0.,-1.,0.));
#22511=DIRECTION('',(-1.,0.,-1.55356845212375E-15));
#22512=DIRECTION('center_axis',(-0.709478283082608,0.,-0.704727298913668));
#22513=DIRECTION('ref_axis',(0.704727298913668,0.,-0.709478283082608));
#22514=DIRECTION('',(0.704727298913668,0.,-0.709478283082608));
#22515=DIRECTION('',(0.,-1.,0.));
#22516=DIRECTION('',(-0.704727298913668,0.,0.709478283082608));
#22517=DIRECTION('center_axis',(0.,1.,0.));
#22518=DIRECTION('ref_axis',(0.709478283082593,0.,0.704727298913683));
#22519=DIRECTION('center_axis',(0.,1.,0.));
#22520=DIRECTION('ref_axis',(0.709478283082593,0.,0.704727298913683));
#22521=DIRECTION('',(0.,-1.,0.));
#22522=DIRECTION('center_axis',(0.,-1.,0.));
#22523=DIRECTION('ref_axis',(0.709478283082593,0.,0.704727298913683));
#22524=DIRECTION('center_axis',(0.,1.,0.));
#22525=DIRECTION('ref_axis',(-1.,0.,0.));
#22526=DIRECTION('center_axis',(0.,-1.,0.));
#22527=DIRECTION('ref_axis',(1.,0.,0.));
#22528=DIRECTION('',(0.702199901316075,0.,0.711979844231348));
#22529=DIRECTION('center_axis',(0.,1.,0.));
#22530=DIRECTION('ref_axis',(-0.951733868867053,0.,0.306924490471762));
#22531=DIRECTION('center_axis',(0.,-1.,0.));
#22532=DIRECTION('ref_axis',(0.951733868867033,0.,-0.306924490471823));
#22533=DIRECTION('center_axis',(0.,1.,0.));
#22534=DIRECTION('ref_axis',(-1.,0.,-1.48029736616691E-14));
#22535=DIRECTION('',(-1.93287220490857E-14,0.,1.));
#22536=DIRECTION('center_axis',(0.,1.,0.));
#22537=DIRECTION('ref_axis',(-0.295138112194515,0.,-0.955454601082782));
#22538=DIRECTION('center_axis',(0.,-1.,0.));
#22539=DIRECTION('ref_axis',(0.295138112194494,0.,0.955454601082788));
#22540=DIRECTION('center_axis',(0.,1.,0.));
#22541=DIRECTION('ref_axis',(-0.710729249896308,0.,-0.703465658964126));
#22542=DIRECTION('',(-0.703465658964212,0.,0.710729249896223));
#22543=DIRECTION('',(-1.,0.,-6.14369354430926E-16));
#22544=DIRECTION('',(-0.703465658964231,0.,-0.710729249896204));
#22545=DIRECTION('center_axis',(0.,1.,0.));
#22546=DIRECTION('ref_axis',(0.963381374692962,0.,-0.26813490428271));
#22547=DIRECTION('center_axis',(0.,-1.,0.));
#22548=DIRECTION('ref_axis',(-0.963381374692976,0.,0.268134904282661));
#22549=DIRECTION('center_axis',(0.,1.,0.));
#22550=DIRECTION('ref_axis',(1.,0.,0.));
#22551=DIRECTION('',(0.,0.,-1.));
#22552=DIRECTION('center_axis',(0.,1.,0.));
#22553=DIRECTION('ref_axis',(0.245760053518526,0.,0.969330694909932));
#22554=DIRECTION('center_axis',(0.,-1.,0.));
#22555=DIRECTION('ref_axis',(-0.245760053518557,0.,-0.969330694909924));
#22556=DIRECTION('',(0.,0.,1.));
#22557=DIRECTION('',(0.,0.,1.));
#22558=DIRECTION('center_axis',(-1.,0.,0.));
#22559=DIRECTION('ref_axis',(0.,0.,-1.));
#22560=DIRECTION('',(0.,0.,-1.));
#22561=DIRECTION('center_axis',(-1.,0.,0.));
#22562=DIRECTION('ref_axis',(0.,0.,-1.));
#22563=DIRECTION('',(0.,0.,-1.));
#22564=DIRECTION('',(0.,1.,0.));
#22565=DIRECTION('center_axis',(0.,1.,0.));
#22566=DIRECTION('ref_axis',(1.,0.,0.));
#22567=DIRECTION('center_axis',(0.,1.,0.));
#22568=DIRECTION('ref_axis',(1.,0.,0.));
#22569=DIRECTION('',(0.,-1.,0.));
#22570=DIRECTION('center_axis',(-0.711979844231348,0.,0.702199901316075));
#22571=DIRECTION('ref_axis',(-0.702199901316075,0.,-0.711979844231348));
#22572=DIRECTION('',(-0.702199901316075,0.,-0.711979844231348));
#22573=DIRECTION('',(0.,-1.,0.));
#22574=DIRECTION('center_axis',(0.,1.,0.));
#22575=DIRECTION('ref_axis',(-0.951733868867053,0.,0.306924490471762));
#22576=DIRECTION('center_axis',(0.,-1.,0.));
#22577=DIRECTION('ref_axis',(-0.951733868867053,0.,0.306924490471762));
#22578=DIRECTION('',(0.,-1.,0.));
#22579=DIRECTION('center_axis',(0.,1.,0.));
#22580=DIRECTION('ref_axis',(0.951733868867033,0.,-0.306924490471823));
#22581=DIRECTION('center_axis',(0.,1.,0.));
#22582=DIRECTION('ref_axis',(0.951733868867033,0.,-0.306924490471823));
#22583=DIRECTION('',(0.,-1.,0.));
#22584=DIRECTION('center_axis',(0.,1.,0.));
#22585=DIRECTION('ref_axis',(-1.,0.,-1.48029736616691E-14));
#22586=DIRECTION('center_axis',(0.,-1.,0.));
#22587=DIRECTION('ref_axis',(-1.,0.,-1.48029736616691E-14));
#22588=DIRECTION('',(0.,-1.,0.));
#22589=DIRECTION('center_axis',(-1.,0.,-1.93287220490857E-14));
#22590=DIRECTION('ref_axis',(1.93287220490857E-14,0.,-1.));
#22591=DIRECTION('',(1.93287220490857E-14,0.,-1.));
#22592=DIRECTION('',(0.,-1.,0.));
#22593=DIRECTION('center_axis',(0.,1.,0.));
#22594=DIRECTION('ref_axis',(-0.295138112194515,0.,-0.955454601082782));
#22595=DIRECTION('center_axis',(0.,-1.,0.));
#22596=DIRECTION('ref_axis',(-0.295138112194515,0.,-0.955454601082782));
#22597=DIRECTION('',(0.,-1.,0.));
#22598=DIRECTION('center_axis',(0.,1.,0.));
#22599=DIRECTION('ref_axis',(0.295138112194494,0.,0.955454601082788));
#22600=DIRECTION('center_axis',(0.,1.,0.));
#22601=DIRECTION('ref_axis',(0.295138112194494,0.,0.955454601082788));
#22602=DIRECTION('',(0.,-1.,0.));
#22603=DIRECTION('center_axis',(0.,1.,0.));
#22604=DIRECTION('ref_axis',(-0.710729249896308,0.,-0.703465658964126));
#22605=DIRECTION('center_axis',(0.,-1.,0.));
#22606=DIRECTION('ref_axis',(-0.710729249896308,0.,-0.703465658964126));
#22607=DIRECTION('',(0.,-1.,0.));
#22608=DIRECTION('center_axis',(-0.710729249896223,0.,-0.703465658964212));
#22609=DIRECTION('ref_axis',(0.703465658964212,0.,-0.710729249896223));
#22610=DIRECTION('',(0.703465658964212,0.,-0.710729249896223));
#22611=DIRECTION('',(0.,-1.,0.));
#22612=DIRECTION('center_axis',(6.14369354430926E-16,0.,-1.));
#22613=DIRECTION('ref_axis',(1.,0.,6.14369354430926E-16));
#22614=DIRECTION('',(1.,0.,6.14369354430926E-16));
#22615=DIRECTION('',(0.,-1.,0.));
#22616=DIRECTION('center_axis',(0.710729249896204,0.,-0.703465658964231));
#22617=DIRECTION('ref_axis',(0.703465658964231,0.,0.710729249896204));
#22618=DIRECTION('',(0.703465658964231,0.,0.710729249896204));
#22619=DIRECTION('',(0.,-1.,0.));
#22620=DIRECTION('center_axis',(0.,1.,0.));
#22621=DIRECTION('ref_axis',(0.963381374692962,0.,-0.26813490428271));
#22622=DIRECTION('center_axis',(0.,-1.,0.));
#22623=DIRECTION('ref_axis',(0.963381374692962,0.,-0.26813490428271));
#22624=DIRECTION('',(0.,-1.,0.));
#22625=DIRECTION('center_axis',(0.,1.,0.));
#22626=DIRECTION('ref_axis',(-0.963381374692976,0.,0.268134904282661));
#22627=DIRECTION('center_axis',(0.,1.,0.));
#22628=DIRECTION('ref_axis',(-0.963381374692976,0.,0.268134904282661));
#22629=DIRECTION('',(0.,-1.,0.));
#22630=DIRECTION('center_axis',(0.,1.,0.));
#22631=DIRECTION('ref_axis',(1.,0.,0.));
#22632=DIRECTION('center_axis',(0.,-1.,0.));
#22633=DIRECTION('ref_axis',(1.,0.,0.));
#22634=DIRECTION('',(0.,-1.,0.));
#22635=DIRECTION('center_axis',(1.,0.,0.));
#22636=DIRECTION('ref_axis',(0.,0.,1.));
#22637=DIRECTION('',(0.,0.,1.));
#22638=DIRECTION('',(0.,-1.,0.));
#22639=DIRECTION('center_axis',(0.,1.,0.));
#22640=DIRECTION('ref_axis',(0.245760053518526,0.,0.969330694909932));
#22641=DIRECTION('center_axis',(0.,-1.,0.));
#22642=DIRECTION('ref_axis',(0.245760053518526,0.,0.969330694909932));
#22643=DIRECTION('',(0.,-1.,0.));
#22644=DIRECTION('center_axis',(0.,1.,0.));
#22645=DIRECTION('ref_axis',(-0.245760053518557,0.,-0.969330694909924));
#22646=DIRECTION('center_axis',(0.,1.,0.));
#22647=DIRECTION('ref_axis',(-0.245760053518557,0.,-0.969330694909924));
#22648=DIRECTION('center_axis',(0.,1.,0.));
#22649=DIRECTION('ref_axis',(1.,0.,0.));
#22650=DIRECTION('axis',(0.,0.,1.));
#22651=DIRECTION('refdir',(1.,0.,0.));
#22652=DIRECTION('center_axis',(0.,-1.,0.));
#22653=DIRECTION('ref_axis',(1.,0.,0.));
#22654=DIRECTION('',(-1.60844785188215E-15,0.,-1.));
#22655=DIRECTION('',(-0.707106781186551,0.,-0.707106781186544));
#22656=DIRECTION('',(-1.,0.,0.));
#22657=DIRECTION('',(-0.707106781186548,0.,0.707106781186548));
#22658=DIRECTION('',(0.,0.,1.));
#22659=DIRECTION('',(0.707106781186549,0.,0.707106781186546));
#22660=DIRECTION('',(1.,0.,0.));
#22661=DIRECTION('',(0.70472729891367,0.,-0.709478283082607));
#22662=DIRECTION('center_axis',(0.,-1.,0.));
#22663=DIRECTION('ref_axis',(-1.,0.,7.19001577852613E-14));
#22664=DIRECTION('',(1.18143967662125E-14,0.,-1.));
#22665=DIRECTION('center_axis',(0.,-1.,0.));
#22666=DIRECTION('ref_axis',(-0.711979844231317,0.,0.702199901316106));
#22667=DIRECTION('',(-0.702199901316085,0.,-0.711979844231338));
#22668=DIRECTION('center_axis',(0.,1.,0.));
#22669=DIRECTION('ref_axis',(0.711979844231347,0.,-0.702199901316076));
#22670=DIRECTION('center_axis',(0.,-1.,0.));
#22671=DIRECTION('ref_axis',(-0.245760053518557,0.,0.969330694909924));
#22672=DIRECTION('center_axis',(0.,1.,0.));
#22673=DIRECTION('ref_axis',(0.245760053518526,0.,-0.969330694909932));
#22674=DIRECTION('',(0.,0.,-1.));
#22675=DIRECTION('center_axis',(0.,1.,0.));
#22676=DIRECTION('ref_axis',(1.,0.,0.));
#22677=DIRECTION('center_axis',(0.,-1.,0.));
#22678=DIRECTION('ref_axis',(-0.963381374692976,0.,-0.268134904282661));
#22679=DIRECTION('center_axis',(0.,1.,0.));
#22680=DIRECTION('ref_axis',(0.963381374692962,0.,0.26813490428271));
#22681=DIRECTION('',(0.703465658964231,0.,-0.710729249896204));
#22682=DIRECTION('',(1.,0.,-6.14369354430926E-16));
#22683=DIRECTION('',(0.703465658964212,0.,0.710729249896223));
#22684=DIRECTION('center_axis',(0.,1.,0.));
#22685=DIRECTION('ref_axis',(-0.710729249896308,0.,0.703465658964126));
#22686=DIRECTION('center_axis',(0.,-1.,0.));
#22687=DIRECTION('ref_axis',(0.295138112194494,0.,-0.955454601082788));
#22688=DIRECTION('center_axis',(0.,1.,0.));
#22689=DIRECTION('ref_axis',(-0.295138112194515,0.,0.955454601082782));
#22690=DIRECTION('',(1.93287220490857E-14,0.,1.));
#22691=DIRECTION('center_axis',(0.,1.,0.));
#22692=DIRECTION('ref_axis',(-1.,0.,1.48029736616691E-14));
#22693=DIRECTION('center_axis',(0.,-1.,0.));
#22694=DIRECTION('ref_axis',(0.951733868867033,0.,0.306924490471823));
#22695=DIRECTION('center_axis',(0.,1.,0.));
#22696=DIRECTION('ref_axis',(-0.951733868867053,0.,-0.306924490471762));
#22697=DIRECTION('',(-0.702199901316075,0.,0.711979844231348));
#22698=DIRECTION('center_axis',(0.,-1.,0.));
#22699=DIRECTION('ref_axis',(1.,0.,0.));
#22700=DIRECTION('',(0.,0.,1.));
#22701=DIRECTION('center_axis',(0.,-1.,0.));
#22702=DIRECTION('ref_axis',(0.709478283082593,0.,-0.704727298913683));
#22703=DIRECTION('',(0.704727298913668,0.,0.709478283082608));
#22704=DIRECTION('',(1.,0.,-1.55356845212375E-15));
#22705=DIRECTION('',(0.707106781186549,0.,-0.707106781186546));
#22706=DIRECTION('center_axis',(-0.710729249896204,0.,-0.703465658964231));
#22707=DIRECTION('ref_axis',(0.703465658964231,0.,-0.710729249896204));
#22708=DIRECTION('',(0.,-1.,0.));
#22709=DIRECTION('',(0.703465658964231,0.,-0.710729249896204));
#22710=DIRECTION('',(0.,-1.,0.));
#22711=DIRECTION('center_axis',(0.,-1.,0.));
#22712=DIRECTION('ref_axis',(0.963381374692962,0.,0.26813490428271));
#22713=DIRECTION('',(0.,-1.,0.));
#22714=DIRECTION('center_axis',(0.,1.,0.));
#22715=DIRECTION('ref_axis',(0.963381374692962,0.,0.26813490428271));
#22716=DIRECTION('center_axis',(0.,-1.,0.));
#22717=DIRECTION('ref_axis',(-0.963381374692976,0.,-0.268134904282661));
#22718=DIRECTION('',(0.,-1.,0.));
#22719=DIRECTION('center_axis',(0.,-1.,0.));
#22720=DIRECTION('ref_axis',(-0.963381374692976,0.,-0.268134904282661));
#22721=DIRECTION('center_axis',(0.,-1.,0.));
#22722=DIRECTION('ref_axis',(1.,0.,0.));
#22723=DIRECTION('',(0.,-1.,0.));
#22724=DIRECTION('center_axis',(0.,1.,0.));
#22725=DIRECTION('ref_axis',(1.,0.,0.));
#22726=DIRECTION('center_axis',(-1.,0.,0.));
#22727=DIRECTION('ref_axis',(0.,0.,-1.));
#22728=DIRECTION('',(0.,-1.,0.));
#22729=DIRECTION('',(0.,0.,-1.));
#22730=DIRECTION('center_axis',(0.,-1.,0.));
#22731=DIRECTION('ref_axis',(0.245760053518526,0.,-0.969330694909932));
#22732=DIRECTION('',(0.,-1.,0.));
#22733=DIRECTION('center_axis',(0.,1.,0.));
#22734=DIRECTION('ref_axis',(0.245760053518526,0.,-0.969330694909932));
#22735=DIRECTION('center_axis',(0.,-1.,0.));
#22736=DIRECTION('ref_axis',(-0.245760053518557,0.,0.969330694909924));
#22737=DIRECTION('',(0.,-1.,0.));
#22738=DIRECTION('center_axis',(0.,-1.,0.));
#22739=DIRECTION('ref_axis',(-0.245760053518557,0.,0.969330694909924));
#22740=DIRECTION('center_axis',(0.,-1.,0.));
#22741=DIRECTION('ref_axis',(0.711979844231347,0.,-0.702199901316076));
#22742=DIRECTION('',(0.,-1.,0.));
#22743=DIRECTION('center_axis',(0.,1.,0.));
#22744=DIRECTION('ref_axis',(0.711979844231347,0.,-0.702199901316076));
#22745=DIRECTION('center_axis',(-0.711979844231338,0.,0.702199901316085));
#22746=DIRECTION('ref_axis',(-0.702199901316085,0.,-0.711979844231338));
#22747=DIRECTION('',(0.,-1.,0.));
#22748=DIRECTION('',(-0.702199901316085,0.,-0.711979844231338));
#22749=DIRECTION('center_axis',(0.,-1.,0.));
#22750=DIRECTION('ref_axis',(-0.711979844231317,0.,0.702199901316106));
#22751=DIRECTION('',(0.,-1.,0.));
#22752=DIRECTION('center_axis',(0.,-1.,0.));
#22753=DIRECTION('ref_axis',(-0.711979844231317,0.,0.702199901316106));
#22754=DIRECTION('center_axis',(-1.,0.,-1.18143967662125E-14));
#22755=DIRECTION('ref_axis',(1.18143967662125E-14,0.,-1.));
#22756=DIRECTION('',(0.,-1.,0.));
#22757=DIRECTION('',(1.18143967662125E-14,0.,-1.));
#22758=DIRECTION('center_axis',(0.,-1.,0.));
#22759=DIRECTION('ref_axis',(-1.,0.,7.19001577852613E-14));
#22760=DIRECTION('',(0.,-1.,0.));
#22761=DIRECTION('center_axis',(0.,-1.,0.));
#22762=DIRECTION('ref_axis',(-1.,0.,7.19001577852613E-14));
#22763=DIRECTION('center_axis',(-0.709478283082607,0.,-0.70472729891367));
#22764=DIRECTION('ref_axis',(0.70472729891367,0.,-0.709478283082607));
#22765=DIRECTION('',(0.,-1.,0.));
#22766=DIRECTION('',(0.70472729891367,0.,-0.709478283082607));
#22767=DIRECTION('center_axis',(0.,0.,-1.));
#22768=DIRECTION('ref_axis',(1.,0.,0.));
#22769=DIRECTION('',(0.,-1.,0.));
#22770=DIRECTION('',(1.,0.,0.));
#22771=DIRECTION('center_axis',(0.707106781186546,0.,-0.707106781186549));
#22772=DIRECTION('ref_axis',(0.707106781186549,0.,0.707106781186546));
#22773=DIRECTION('',(0.,-1.,0.));
#22774=DIRECTION('',(0.707106781186549,0.,0.707106781186546));
#22775=DIRECTION('center_axis',(1.,0.,0.));
#22776=DIRECTION('ref_axis',(0.,0.,1.));
#22777=DIRECTION('',(0.,-1.,0.));
#22778=DIRECTION('',(0.,0.,1.));
#22779=DIRECTION('center_axis',(-1.,0.,1.60844785188215E-15));
#22780=DIRECTION('ref_axis',(-1.60844785188215E-15,0.,-1.));
#22781=DIRECTION('',(0.,-1.,0.));
#22782=DIRECTION('',(-1.60844785188215E-15,0.,-1.));
#22783=DIRECTION('',(0.,-1.,0.));
#22784=DIRECTION('center_axis',(-0.707106781186546,0.,-0.707106781186549));
#22785=DIRECTION('ref_axis',(0.707106781186549,0.,-0.707106781186546));
#22786=DIRECTION('',(0.,-1.,0.));
#22787=DIRECTION('',(0.707106781186549,0.,-0.707106781186546));
#22788=DIRECTION('center_axis',(-1.55356845212375E-15,0.,-1.));
#22789=DIRECTION('ref_axis',(1.,0.,-1.55356845212375E-15));
#22790=DIRECTION('',(0.,-1.,0.));
#22791=DIRECTION('',(1.,0.,-1.55356845212375E-15));
#22792=DIRECTION('center_axis',(0.709478283082608,0.,-0.704727298913668));
#22793=DIRECTION('ref_axis',(0.704727298913668,0.,0.709478283082608));
#22794=DIRECTION('',(0.,-1.,0.));
#22795=DIRECTION('',(0.704727298913668,0.,0.709478283082608));
#22796=DIRECTION('center_axis',(0.,-1.,0.));
#22797=DIRECTION('ref_axis',(0.709478283082593,0.,-0.704727298913683));
#22798=DIRECTION('',(0.,-1.,0.));
#22799=DIRECTION('center_axis',(0.,-1.,0.));
#22800=DIRECTION('ref_axis',(0.709478283082593,0.,-0.704727298913683));
#22801=DIRECTION('center_axis',(0.707106781186548,0.,0.707106781186548));
#22802=DIRECTION('ref_axis',(-0.707106781186548,0.,0.707106781186548));
#22803=DIRECTION('',(0.,-1.,0.));
#22804=DIRECTION('',(-0.707106781186548,0.,0.707106781186548));
#22805=DIRECTION('center_axis',(0.,0.,1.));
#22806=DIRECTION('ref_axis',(-1.,0.,0.));
#22807=DIRECTION('',(0.,-1.,0.));
#22808=DIRECTION('',(-1.,0.,0.));
#22809=DIRECTION('center_axis',(-0.707106781186544,0.,0.707106781186551));
#22810=DIRECTION('ref_axis',(-0.707106781186551,0.,-0.707106781186544));
#22811=DIRECTION('',(-0.707106781186551,0.,-0.707106781186544));
#22812=DIRECTION('center_axis',(1.,0.,0.));
#22813=DIRECTION('ref_axis',(0.,0.,1.));
#22814=DIRECTION('',(0.,1.,0.));
#22815=DIRECTION('',(0.,0.,1.));
#22816=DIRECTION('center_axis',(-6.14369354430926E-16,0.,-1.));
#22817=DIRECTION('ref_axis',(1.,0.,-6.14369354430926E-16));
#22818=DIRECTION('',(1.,0.,-6.14369354430926E-16));
#22819=DIRECTION('',(0.,-1.,0.));
#22820=DIRECTION('center_axis',(0.710729249896223,0.,-0.703465658964212));
#22821=DIRECTION('ref_axis',(0.703465658964212,0.,0.710729249896223));
#22822=DIRECTION('',(0.703465658964212,0.,0.710729249896223));
#22823=DIRECTION('',(0.,-1.,0.));
#22824=DIRECTION('center_axis',(0.,-1.,0.));
#22825=DIRECTION('ref_axis',(-0.710729249896308,0.,0.703465658964126));
#22826=DIRECTION('center_axis',(0.,1.,0.));
#22827=DIRECTION('ref_axis',(-0.710729249896308,0.,0.703465658964126));
#22828=DIRECTION('',(0.,-1.,0.));
#22829=DIRECTION('center_axis',(0.,-1.,0.));
#22830=DIRECTION('ref_axis',(0.295138112194494,0.,-0.955454601082788));
#22831=DIRECTION('center_axis',(0.,-1.,0.));
#22832=DIRECTION('ref_axis',(0.295138112194494,0.,-0.955454601082788));
#22833=DIRECTION('',(0.,-1.,0.));
#22834=DIRECTION('center_axis',(0.,-1.,0.));
#22835=DIRECTION('ref_axis',(-0.295138112194515,0.,0.955454601082782));
#22836=DIRECTION('center_axis',(0.,1.,0.));
#22837=DIRECTION('ref_axis',(-0.295138112194515,0.,0.955454601082782));
#22838=DIRECTION('',(0.,-1.,0.));
#22839=DIRECTION('center_axis',(1.,0.,-1.93287220490857E-14));
#22840=DIRECTION('ref_axis',(1.93287220490857E-14,0.,1.));
#22841=DIRECTION('',(1.93287220490857E-14,0.,1.));
#22842=DIRECTION('',(0.,-1.,0.));
#22843=DIRECTION('center_axis',(0.,-1.,0.));
#22844=DIRECTION('ref_axis',(-1.,0.,1.48029736616691E-14));
#22845=DIRECTION('center_axis',(0.,1.,0.));
#22846=DIRECTION('ref_axis',(-1.,0.,1.48029736616691E-14));
#22847=DIRECTION('',(0.,-1.,0.));
#22848=DIRECTION('center_axis',(0.,-1.,0.));
#22849=DIRECTION('ref_axis',(0.951733868867033,0.,0.306924490471823));
#22850=DIRECTION('center_axis',(0.,-1.,0.));
#22851=DIRECTION('ref_axis',(0.951733868867033,0.,0.306924490471823));
#22852=DIRECTION('',(0.,-1.,0.));
#22853=DIRECTION('center_axis',(0.,-1.,0.));
#22854=DIRECTION('ref_axis',(-0.951733868867053,0.,-0.306924490471762));
#22855=DIRECTION('center_axis',(0.,1.,0.));
#22856=DIRECTION('ref_axis',(-0.951733868867053,0.,-0.306924490471762));
#22857=DIRECTION('',(0.,-1.,0.));
#22858=DIRECTION('center_axis',(0.711979844231348,0.,0.702199901316075));
#22859=DIRECTION('ref_axis',(-0.702199901316075,0.,0.711979844231348));
#22860=DIRECTION('',(-0.702199901316075,0.,0.711979844231348));
#22861=DIRECTION('',(0.,-1.,0.));
#22862=DIRECTION('center_axis',(0.,-1.,0.));
#22863=DIRECTION('ref_axis',(1.,0.,0.));
#22864=DIRECTION('center_axis',(0.,-1.,0.));
#22865=DIRECTION('ref_axis',(1.,0.,0.));
#22866=DIRECTION('center_axis',(0.,-1.,0.));
#22867=DIRECTION('ref_axis',(-1.,0.,0.));
#22868=DIRECTION('center_axis',(-0.710729249896204,0.,-0.703465658964231));
#22869=DIRECTION('ref_axis',(0.703465658964231,0.,-0.710729249896204));
#22870=DIRECTION('',(0.703465658964231,0.,-0.710729249896204));
#22871=DIRECTION('',(0.,-1.,0.));
#22872=DIRECTION('',(0.703465658964231,0.,-0.710729249896204));
#22873=DIRECTION('',(0.,-1.,0.));
#22874=DIRECTION('center_axis',(0.,-1.,0.));
#22875=DIRECTION('ref_axis',(0.963381374692962,0.,0.26813490428271));
#22876=DIRECTION('center_axis',(0.,1.,0.));
#22877=DIRECTION('ref_axis',(0.963381374692962,0.,0.26813490428271));
#22878=DIRECTION('center_axis',(0.,1.,0.));
#22879=DIRECTION('ref_axis',(0.963381374692962,0.,0.26813490428271));
#22880=DIRECTION('',(0.,-1.,0.));
#22881=DIRECTION('center_axis',(0.,-1.,0.));
#22882=DIRECTION('ref_axis',(-0.963381374692976,0.,-0.268134904282661));
#22883=DIRECTION('center_axis',(0.,-1.,0.));
#22884=DIRECTION('ref_axis',(-0.963381374692976,0.,-0.268134904282661));
#22885=DIRECTION('center_axis',(0.,-1.,0.));
#22886=DIRECTION('ref_axis',(-0.963381374692976,0.,-0.268134904282661));
#22887=DIRECTION('',(0.,-1.,0.));
#22888=DIRECTION('center_axis',(0.,-1.,0.));
#22889=DIRECTION('ref_axis',(1.,0.,0.));
#22890=DIRECTION('center_axis',(0.,1.,0.));
#22891=DIRECTION('ref_axis',(1.,0.,0.));
#22892=DIRECTION('center_axis',(0.,1.,0.));
#22893=DIRECTION('ref_axis',(1.,0.,0.));
#22894=DIRECTION('',(0.,-1.,0.));
#22895=DIRECTION('center_axis',(-1.,0.,0.));
#22896=DIRECTION('ref_axis',(0.,0.,-1.));
#22897=DIRECTION('',(0.,0.,-1.));
#22898=DIRECTION('',(0.,0.,-1.));
#22899=DIRECTION('',(0.,-1.,0.));
#22900=DIRECTION('center_axis',(0.,-1.,0.));
#22901=DIRECTION('ref_axis',(0.245760053518526,0.,-0.969330694909932));
#22902=DIRECTION('center_axis',(0.,1.,0.));
#22903=DIRECTION('ref_axis',(0.245760053518526,0.,-0.969330694909932));
#22904=DIRECTION('center_axis',(0.,1.,0.));
#22905=DIRECTION('ref_axis',(0.245760053518526,0.,-0.969330694909932));
#22906=DIRECTION('',(0.,-1.,0.));
#22907=DIRECTION('center_axis',(0.,-1.,0.));
#22908=DIRECTION('ref_axis',(-0.245760053518557,0.,0.969330694909924));
#22909=DIRECTION('center_axis',(0.,-1.,0.));
#22910=DIRECTION('ref_axis',(-0.245760053518557,0.,0.969330694909924));
#22911=DIRECTION('center_axis',(0.,-1.,0.));
#22912=DIRECTION('ref_axis',(-0.245760053518557,0.,0.969330694909924));
#22913=DIRECTION('',(0.,-1.,0.));
#22914=DIRECTION('center_axis',(0.,-1.,0.));
#22915=DIRECTION('ref_axis',(-1.,0.,0.));
#22916=DIRECTION('',(0.707106781186554,0.,0.707106781186541));
#22917=DIRECTION('',(0.,0.,1.));
#22918=DIRECTION('',(-0.707106781186548,0.,0.707106781186548));
#22919=DIRECTION('',(-1.,0.,0.));
#22920=DIRECTION('center_axis',(0.,1.,0.));
#22921=DIRECTION('ref_axis',(1.63979029060989E-14,0.,-1.));
#22922=DIRECTION('',(-1.,0.,0.));
#22923=DIRECTION('center_axis',(0.,-1.,0.));
#22924=DIRECTION('ref_axis',(-1.37675000001205E-14,0.,-1.));
#22925=DIRECTION('',(1.,0.,2.63040290597841E-15));
#22926=DIRECTION('',(0.707106781186546,0.,0.707106781186549));
#22927=DIRECTION('',(-2.63040290597841E-15,0.,1.));
#22928=DIRECTION('',(-0.707106781186556,0.,0.707106781186539));
#22929=DIRECTION('',(-1.60844785188215E-15,0.,-1.));
#22930=DIRECTION('',(0.707106781186549,0.,-0.707106781186546));
#22931=DIRECTION('',(1.,0.,-1.55356845212375E-15));
#22932=DIRECTION('',(0.704727298913668,0.,0.709478283082608));
#22933=DIRECTION('center_axis',(0.,-1.,0.));
#22934=DIRECTION('ref_axis',(0.709478283082593,0.,-0.704727298913683));
#22935=DIRECTION('',(0.,0.,1.));
#22936=DIRECTION('center_axis',(0.,-1.,0.));
#22937=DIRECTION('ref_axis',(1.,0.,0.));
#22938=DIRECTION('',(-0.702199901316075,0.,0.711979844231348));
#22939=DIRECTION('center_axis',(0.,1.,0.));
#22940=DIRECTION('ref_axis',(-0.951733868867053,0.,-0.306924490471762));
#22941=DIRECTION('center_axis',(0.,-1.,0.));
#22942=DIRECTION('ref_axis',(0.951733868867033,0.,0.306924490471823));
#22943=DIRECTION('center_axis',(0.,1.,0.));
#22944=DIRECTION('ref_axis',(-1.,0.,1.48029736616691E-14));
#22945=DIRECTION('',(1.93287220490857E-14,0.,1.));
#22946=DIRECTION('center_axis',(0.,1.,0.));
#22947=DIRECTION('ref_axis',(-0.295138112194515,0.,0.955454601082782));
#22948=DIRECTION('center_axis',(0.,-1.,0.));
#22949=DIRECTION('ref_axis',(0.295138112194494,0.,-0.955454601082788));
#22950=DIRECTION('center_axis',(0.,1.,0.));
#22951=DIRECTION('ref_axis',(-0.710729249896308,0.,0.703465658964126));
#22952=DIRECTION('',(0.703465658964212,0.,0.710729249896223));
#22953=DIRECTION('',(1.,0.,-6.14369354430926E-16));
#22954=DIRECTION('center_axis',(0.,1.,0.));
#22955=DIRECTION('ref_axis',(0.711979844231347,0.,-0.702199901316076));
#22956=DIRECTION('',(-0.702199901316085,0.,-0.711979844231338));
#22957=DIRECTION('center_axis',(0.,-1.,0.));
#22958=DIRECTION('ref_axis',(-0.711979844231317,0.,0.702199901316106));
#22959=DIRECTION('',(1.18143967662125E-14,0.,-1.));
#22960=DIRECTION('center_axis',(0.,-1.,0.));
#22961=DIRECTION('ref_axis',(-1.,0.,7.19001577852613E-14));
#22962=DIRECTION('',(0.70472729891367,0.,-0.709478283082607));
#22963=DIRECTION('',(1.,0.,0.));
#22964=DIRECTION('',(0.707106781186549,0.,0.707106781186546));
#22965=DIRECTION('',(0.,0.,1.));
#22966=DIRECTION('center_axis',(0.707106781186541,0.,-0.707106781186554));
#22967=DIRECTION('ref_axis',(0.707106781186554,0.,0.707106781186541));
#22968=DIRECTION('',(0.,-1.,0.));
#22969=DIRECTION('',(0.,-1.,0.));
#22970=DIRECTION('',(-0.707106781186554,0.,-0.707106781186541));
#22971=DIRECTION('center_axis',(1.,0.,0.));
#22972=DIRECTION('ref_axis',(0.,0.,1.));
#22973=DIRECTION('',(0.,-1.,0.));
#22974=DIRECTION('',(0.,0.,-1.));
#22975=DIRECTION('center_axis',(0.707106781186548,0.,0.707106781186548));
#22976=DIRECTION('ref_axis',(-0.707106781186548,0.,0.707106781186548));
#22977=DIRECTION('',(0.,-1.,0.));
#22978=DIRECTION('',(0.707106781186548,0.,-0.707106781186548));
#22979=DIRECTION('center_axis',(0.,0.,1.));
#22980=DIRECTION('ref_axis',(-1.,0.,0.));
#22981=DIRECTION('',(0.,-1.,0.));
#22982=DIRECTION('',(1.,0.,0.));
#22983=DIRECTION('center_axis',(0.,0.,-1.));
#22984=DIRECTION('ref_axis',(-1.,0.,0.));
#22985=DIRECTION('center_axis',(0.,0.,-1.));
#22986=DIRECTION('ref_axis',(-1.,0.,0.));
#22987=DIRECTION('center_axis',(0.,-1.,0.));
#22988=DIRECTION('ref_axis',(1.63979029060989E-14,0.,-1.));
#22989=DIRECTION('',(0.,-1.,0.));
#22990=DIRECTION('center_axis',(0.,-1.,0.));
#22991=DIRECTION('ref_axis',(1.63979029060989E-14,0.,-1.));
#22992=DIRECTION('center_axis',(0.,0.,1.));
#22993=DIRECTION('ref_axis',(-1.,0.,0.));
#22994=DIRECTION('',(-1.,0.,-2.63040290597841E-15));
#22995=DIRECTION('',(0.,-1.,0.));
#22996=DIRECTION('center_axis',(0.,-1.,0.));
#22997=DIRECTION('ref_axis',(-1.,0.,0.));
#22998=DIRECTION('',(0.,0.,1.));
#22999=DIRECTION('',(0.707106781186549,0.,0.707106781186546));
#23000=DIRECTION('',(1.,0.,0.));
#23001=DIRECTION('',(0.70472729891367,0.,-0.709478283082607));
#23002=DIRECTION('center_axis',(0.,-1.,0.));
#23003=DIRECTION('ref_axis',(-1.,0.,7.19001577852613E-14));
#23004=DIRECTION('',(1.18143967662125E-14,0.,-1.));
#23005=DIRECTION('center_axis',(0.,-1.,0.));
#23006=DIRECTION('ref_axis',(-0.711979844231317,0.,0.702199901316106));
#23007=DIRECTION('',(-0.702199901316085,0.,-0.711979844231338));
#23008=DIRECTION('center_axis',(0.,1.,0.));
#23009=DIRECTION('ref_axis',(0.711979844231347,0.,-0.702199901316076));
#23010=DIRECTION('',(1.,0.,-6.14369354430926E-16));
#23011=DIRECTION('',(0.703465658964212,0.,0.710729249896223));
#23012=DIRECTION('center_axis',(0.,1.,0.));
#23013=DIRECTION('ref_axis',(-0.710729249896308,0.,0.703465658964126));
#23014=DIRECTION('center_axis',(0.,-1.,0.));
#23015=DIRECTION('ref_axis',(0.295138112194494,0.,-0.955454601082788));
#23016=DIRECTION('center_axis',(0.,1.,0.));
#23017=DIRECTION('ref_axis',(-0.295138112194515,0.,0.955454601082782));
#23018=DIRECTION('',(1.93287220490857E-14,0.,1.));
#23019=DIRECTION('center_axis',(0.,1.,0.));
#23020=DIRECTION('ref_axis',(-1.,0.,1.48029736616691E-14));
#23021=DIRECTION('center_axis',(0.,-1.,0.));
#23022=DIRECTION('ref_axis',(0.951733868867033,0.,0.306924490471823));
#23023=DIRECTION('center_axis',(0.,1.,0.));
#23024=DIRECTION('ref_axis',(-0.951733868867053,0.,-0.306924490471762));
#23025=DIRECTION('',(-0.702199901316075,0.,0.711979844231348));
#23026=DIRECTION('center_axis',(0.,-1.,0.));
#23027=DIRECTION('ref_axis',(1.,0.,0.));
#23028=DIRECTION('',(0.,0.,1.));
#23029=DIRECTION('center_axis',(0.,-1.,0.));
#23030=DIRECTION('ref_axis',(0.709478283082593,0.,-0.704727298913683));
#23031=DIRECTION('',(0.704727298913668,0.,0.709478283082608));
#23032=DIRECTION('',(1.,0.,-1.55356845212375E-15));
#23033=DIRECTION('',(0.707106781186549,0.,-0.707106781186546));
#23034=DIRECTION('',(-1.60844785188215E-15,0.,-1.));
#23035=DIRECTION('',(0.707106781186556,0.,-0.707106781186539));
#23036=DIRECTION('',(2.63040290597841E-15,0.,-1.));
#23037=DIRECTION('',(-0.707106781186546,0.,-0.707106781186549));
#23038=DIRECTION('',(-1.,0.,-2.63040290597841E-15));
#23039=DIRECTION('center_axis',(0.,1.,0.));
#23040=DIRECTION('ref_axis',(-1.37675000001205E-14,0.,-1.));
#23041=DIRECTION('center_axis',(0.707106781186539,0.,0.707106781186556));
#23042=DIRECTION('ref_axis',(-0.707106781186556,0.,0.707106781186539));
#23043=DIRECTION('',(0.,-1.,0.));
#23044=DIRECTION('',(0.,1.,0.));
#23045=DIRECTION('center_axis',(1.,0.,2.63040290597841E-15));
#23046=DIRECTION('ref_axis',(-2.63040290597841E-15,0.,1.));
#23047=DIRECTION('',(0.,-1.,0.));
#23048=DIRECTION('center_axis',(0.707106781186549,0.,-0.707106781186546));
#23049=DIRECTION('ref_axis',(0.707106781186546,0.,0.707106781186549));
#23050=DIRECTION('',(0.,-1.,0.));
#23051=DIRECTION('center_axis',(2.63040290597841E-15,0.,-1.));
#23052=DIRECTION('ref_axis',(1.,0.,2.63040290597841E-15));
#23053=DIRECTION('',(0.,-1.,0.));
#23054=DIRECTION('center_axis',(2.63040290597841E-15,0.,-1.));
#23055=DIRECTION('ref_axis',(-1.,0.,0.));
#23056=DIRECTION('center_axis',(2.63040290597841E-15,0.,-1.));
#23057=DIRECTION('ref_axis',(-1.,0.,0.));
#23058=DIRECTION('center_axis',(0.,1.,0.));
#23059=DIRECTION('ref_axis',(-1.37675000001205E-14,0.,-1.));
#23060=DIRECTION('center_axis',(0.,0.,-1.));
#23061=DIRECTION('ref_axis',(-1.,0.,0.));
#23062=DIRECTION('',(0.,0.,-1.));
#23063=DIRECTION('center_axis',(0.,0.,1.));
#23064=DIRECTION('ref_axis',(-1.,0.,0.));
#23065=DIRECTION('center_axis',(0.,0.,-1.));
#23066=DIRECTION('ref_axis',(-1.,0.,0.));
#23067=DIRECTION('',(0.,0.,-1.));
#23068=DIRECTION('center_axis',(1.55356845212375E-15,0.,1.));
#23069=DIRECTION('ref_axis',(-1.,0.,0.));
#23070=DIRECTION('center_axis',(0.,0.,-1.));
#23071=DIRECTION('ref_axis',(-1.,0.,0.));
#23072=DIRECTION('',(0.,0.,-1.));
#23073=DIRECTION('center_axis',(0.,0.,1.));
#23074=DIRECTION('ref_axis',(-1.,0.,0.));
#23075=DIRECTION('center_axis',(0.,0.,-1.));
#23076=DIRECTION('ref_axis',(-1.,0.,0.));
#23077=DIRECTION('',(0.,0.,-1.));
#23078=DIRECTION('center_axis',(1.55356845212375E-15,0.,1.));
#23079=DIRECTION('ref_axis',(-1.,0.,0.));
#23080=DIRECTION('center_axis',(1.,0.,0.));
#23081=DIRECTION('ref_axis',(0.,0.,1.));
#23082=DIRECTION('',(0.,-1.,0.));
#23083=DIRECTION('center_axis',(0.707106781186546,0.,-0.707106781186549));
#23084=DIRECTION('ref_axis',(0.707106781186549,0.,0.707106781186546));
#23085=DIRECTION('',(0.,-1.,0.));
#23086=DIRECTION('center_axis',(0.,0.,-1.));
#23087=DIRECTION('ref_axis',(1.,0.,0.));
#23088=DIRECTION('',(0.,-1.,0.));
#23089=DIRECTION('center_axis',(-0.709478283082607,0.,-0.70472729891367));
#23090=DIRECTION('ref_axis',(0.70472729891367,0.,-0.709478283082607));
#23091=DIRECTION('',(0.,-1.,0.));
#23092=DIRECTION('center_axis',(0.,-1.,0.));
#23093=DIRECTION('ref_axis',(-1.,0.,7.19001577852613E-14));
#23094=DIRECTION('',(0.,-1.,0.));
#23095=DIRECTION('center_axis',(-1.,0.,-1.18143967662125E-14));
#23096=DIRECTION('ref_axis',(1.18143967662125E-14,0.,-1.));
#23097=DIRECTION('',(0.,-1.,0.));
#23098=DIRECTION('center_axis',(0.,-1.,0.));
#23099=DIRECTION('ref_axis',(-0.711979844231317,0.,0.702199901316106));
#23100=DIRECTION('',(0.,-1.,0.));
#23101=DIRECTION('center_axis',(-0.711979844231338,0.,0.702199901316085));
#23102=DIRECTION('ref_axis',(-0.702199901316085,0.,-0.711979844231338));
#23103=DIRECTION('',(0.,-1.,0.));
#23104=DIRECTION('center_axis',(0.,-1.,0.));
#23105=DIRECTION('ref_axis',(0.711979844231347,0.,-0.702199901316076));
#23106=DIRECTION('center_axis',(-1.,0.,1.60844785188215E-15));
#23107=DIRECTION('ref_axis',(-1.60844785188215E-15,0.,-1.));
#23108=DIRECTION('',(0.,-1.,0.));
#23109=DIRECTION('center_axis',(-0.707106781186546,0.,-0.707106781186549));
#23110=DIRECTION('ref_axis',(0.707106781186549,0.,-0.707106781186546));
#23111=DIRECTION('',(0.,-1.,0.));
#23112=DIRECTION('center_axis',(-1.55356845212375E-15,0.,-1.));
#23113=DIRECTION('ref_axis',(1.,0.,-1.55356845212375E-15));
#23114=DIRECTION('',(0.,-1.,0.));
#23115=DIRECTION('center_axis',(0.709478283082608,0.,-0.704727298913668));
#23116=DIRECTION('ref_axis',(0.704727298913668,0.,0.709478283082608));
#23117=DIRECTION('',(0.,-1.,0.));
#23118=DIRECTION('center_axis',(0.,-1.,0.));
#23119=DIRECTION('ref_axis',(0.709478283082593,0.,-0.704727298913683));
#23120=DIRECTION('',(0.,-1.,0.));
#23121=DIRECTION('center_axis',(1.,0.,0.));
#23122=DIRECTION('ref_axis',(0.,0.,1.));
#23123=DIRECTION('',(0.,1.,0.));
#23124=DIRECTION('center_axis',(0.,-1.,0.));
#23125=DIRECTION('ref_axis',(1.,0.,0.));
#23126=DIRECTION('',(0.,-1.,0.));
#23127=DIRECTION('center_axis',(0.711979844231348,0.,0.702199901316075));
#23128=DIRECTION('ref_axis',(-0.702199901316075,0.,0.711979844231348));
#23129=DIRECTION('',(0.,-1.,0.));
#23130=DIRECTION('center_axis',(0.,-1.,0.));
#23131=DIRECTION('ref_axis',(-0.951733868867053,0.,-0.306924490471762));
#23132=DIRECTION('',(0.,-1.,0.));
#23133=DIRECTION('center_axis',(0.,-1.,0.));
#23134=DIRECTION('ref_axis',(0.951733868867033,0.,0.306924490471823));
#23135=DIRECTION('',(0.,-1.,0.));
#23136=DIRECTION('center_axis',(0.,-1.,0.));
#23137=DIRECTION('ref_axis',(-1.,0.,1.48029736616691E-14));
#23138=DIRECTION('',(0.,-1.,0.));
#23139=DIRECTION('center_axis',(1.,0.,-1.93287220490857E-14));
#23140=DIRECTION('ref_axis',(1.93287220490857E-14,0.,1.));
#23141=DIRECTION('',(0.,-1.,0.));
#23142=DIRECTION('center_axis',(0.,-1.,0.));
#23143=DIRECTION('ref_axis',(-0.295138112194515,0.,0.955454601082782));
#23144=DIRECTION('',(0.,-1.,0.));
#23145=DIRECTION('center_axis',(0.,-1.,0.));
#23146=DIRECTION('ref_axis',(0.295138112194494,0.,-0.955454601082788));
#23147=DIRECTION('',(0.,-1.,0.));
#23148=DIRECTION('center_axis',(0.,-1.,0.));
#23149=DIRECTION('ref_axis',(-0.710729249896308,0.,0.703465658964126));
#23150=DIRECTION('',(0.,-1.,0.));
#23151=DIRECTION('center_axis',(0.710729249896223,0.,-0.703465658964212));
#23152=DIRECTION('ref_axis',(0.703465658964212,0.,0.710729249896223));
#23153=DIRECTION('',(0.,-1.,0.));
#23154=DIRECTION('center_axis',(-6.14369354430926E-16,0.,-1.));
#23155=DIRECTION('ref_axis',(1.,0.,-6.14369354430926E-16));
#23156=DIRECTION('center_axis',(0.,-1.,0.));
#23157=DIRECTION('ref_axis',(0.711979844231347,0.,-0.702199901316076));
#23158=DIRECTION('center_axis',(0.,1.,0.));
#23159=DIRECTION('ref_axis',(0.711979844231347,0.,-0.702199901316076));
#23160=DIRECTION('',(0.,-1.,0.));
#23161=DIRECTION('center_axis',(0.,-1.,0.));
#23162=DIRECTION('ref_axis',(0.711979844231347,0.,-0.702199901316076));
#23163=DIRECTION('',(0.,-1.,0.));
#23164=DIRECTION('center_axis',(-0.711979844231338,0.,0.702199901316085));
#23165=DIRECTION('ref_axis',(-0.702199901316085,0.,-0.711979844231338));
#23166=DIRECTION('',(-0.702199901316085,0.,-0.711979844231338));
#23167=DIRECTION('',(0.702199901316085,0.,0.711979844231338));
#23168=DIRECTION('',(0.,-1.,0.));
#23169=DIRECTION('center_axis',(0.,-1.,0.));
#23170=DIRECTION('ref_axis',(-0.711979844231317,0.,0.702199901316106));
#23171=DIRECTION('center_axis',(0.,-1.,0.));
#23172=DIRECTION('ref_axis',(-0.711979844231317,0.,0.702199901316106));
#23173=DIRECTION('center_axis',(0.,1.,0.));
#23174=DIRECTION('ref_axis',(-0.711979844231317,0.,0.702199901316106));
#23175=DIRECTION('',(0.,-1.,0.));
#23176=DIRECTION('center_axis',(-1.,0.,-1.18143967662125E-14));
#23177=DIRECTION('ref_axis',(1.18143967662125E-14,0.,-1.));
#23178=DIRECTION('',(1.18143967662125E-14,0.,-1.));
#23179=DIRECTION('',(-1.18143967662125E-14,0.,1.));
#23180=DIRECTION('',(0.,-1.,0.));
#23181=DIRECTION('center_axis',(0.,-1.,0.));
#23182=DIRECTION('ref_axis',(-1.,0.,7.19001577852613E-14));
#23183=DIRECTION('center_axis',(0.,-1.,0.));
#23184=DIRECTION('ref_axis',(-1.,0.,7.19001577852613E-14));
#23185=DIRECTION('center_axis',(0.,1.,0.));
#23186=DIRECTION('ref_axis',(-1.,0.,7.19001577852613E-14));
#23187=DIRECTION('',(0.,-1.,0.));
#23188=DIRECTION('center_axis',(-0.709478283082607,0.,-0.70472729891367));
#23189=DIRECTION('ref_axis',(0.70472729891367,0.,-0.709478283082607));
#23190=DIRECTION('',(0.70472729891367,0.,-0.709478283082607));
#23191=DIRECTION('',(-0.70472729891367,0.,0.709478283082607));
#23192=DIRECTION('',(0.,-1.,0.));
#23193=DIRECTION('center_axis',(0.,0.,-1.));
#23194=DIRECTION('ref_axis',(1.,0.,0.));
#23195=DIRECTION('',(1.,0.,0.));
#23196=DIRECTION('',(-1.,0.,0.));
#23197=DIRECTION('',(0.,-1.,0.));
#23198=DIRECTION('center_axis',(0.707106781186546,0.,-0.707106781186549));
#23199=DIRECTION('ref_axis',(0.707106781186549,0.,0.707106781186546));
#23200=DIRECTION('',(0.707106781186549,0.,0.707106781186546));
#23201=DIRECTION('',(-0.707106781186549,0.,-0.707106781186546));
#23202=DIRECTION('',(0.,-1.,0.));
#23203=DIRECTION('center_axis',(0.707106781186548,0.,0.707106781186548));
#23204=DIRECTION('ref_axis',(-0.707106781186548,0.,0.707106781186548));
#23205=DIRECTION('',(0.707106781186548,0.,-0.707106781186548));
#23206=DIRECTION('',(0.,-1.,0.));
#23207=DIRECTION('',(0.707106781186548,0.,-0.707106781186548));
#23208=DIRECTION('',(0.,-1.,0.));
#23209=DIRECTION('center_axis',(0.,0.,1.));
#23210=DIRECTION('ref_axis',(-1.,0.,0.));
#23211=DIRECTION('',(1.,0.,0.));
#23212=DIRECTION('',(1.,0.,0.));
#23213=DIRECTION('',(0.,-1.,0.));
#23214=DIRECTION('center_axis',(-0.707106781186544,0.,0.707106781186551));
#23215=DIRECTION('ref_axis',(-0.707106781186551,0.,-0.707106781186544));
#23216=DIRECTION('',(0.707106781186551,0.,0.707106781186544));
#23217=DIRECTION('',(0.707106781186551,0.,0.707106781186544));
#23218=DIRECTION('',(0.,-1.,0.));
#23219=DIRECTION('center_axis',(-1.,0.,1.60844785188215E-15));
#23220=DIRECTION('ref_axis',(-1.60844785188215E-15,0.,-1.));
#23221=DIRECTION('',(-1.60844785188215E-15,0.,-1.));
#23222=DIRECTION('',(1.60844785188215E-15,0.,1.));
#23223=DIRECTION('',(0.,-1.,0.));
#23224=DIRECTION('center_axis',(-0.707106781186546,0.,-0.707106781186549));
#23225=DIRECTION('ref_axis',(0.707106781186549,0.,-0.707106781186546));
#23226=DIRECTION('',(0.707106781186549,0.,-0.707106781186546));
#23227=DIRECTION('',(-0.707106781186549,0.,0.707106781186546));
#23228=DIRECTION('',(0.,-1.,0.));
#23229=DIRECTION('center_axis',(-1.55356845212375E-15,0.,-1.));
#23230=DIRECTION('ref_axis',(1.,0.,-1.55356845212375E-15));
#23231=DIRECTION('',(1.,0.,-1.55356845212375E-15));
#23232=DIRECTION('',(-1.,0.,1.55356845212375E-15));
#23233=DIRECTION('',(0.,-1.,0.));
#23234=DIRECTION('center_axis',(0.709478283082608,0.,-0.704727298913668));
#23235=DIRECTION('ref_axis',(0.704727298913668,0.,0.709478283082608));
#23236=DIRECTION('',(0.704727298913668,0.,0.709478283082608));
#23237=DIRECTION('',(-0.704727298913668,0.,-0.709478283082608));
#23238=DIRECTION('',(0.,-1.,0.));
#23239=DIRECTION('center_axis',(0.,-1.,0.));
#23240=DIRECTION('ref_axis',(0.709478283082593,0.,-0.704727298913683));
#23241=DIRECTION('center_axis',(0.,-1.,0.));
#23242=DIRECTION('ref_axis',(0.709478283082593,0.,-0.704727298913683));
#23243=DIRECTION('center_axis',(0.,1.,0.));
#23244=DIRECTION('ref_axis',(0.709478283082593,0.,-0.704727298913683));
#23245=DIRECTION('',(0.,-1.,0.));
#23246=DIRECTION('center_axis',(0.,-1.,0.));
#23247=DIRECTION('ref_axis',(-1.,0.,0.));
#23248=DIRECTION('center_axis',(0.,1.,0.));
#23249=DIRECTION('ref_axis',(1.,0.,0.));
#23250=DIRECTION('',(0.,0.,-1.));
#23251=DIRECTION('',(0.,0.,-1.));
#23252=DIRECTION('center_axis',(0.,1.,0.));
#23253=DIRECTION('ref_axis',(-0.245760053518557,0.,0.969330694909924));
#23254=DIRECTION('center_axis',(0.,-1.,0.));
#23255=DIRECTION('ref_axis',(0.245760053518526,0.,-0.969330694909932));
#23256=DIRECTION('',(0.,0.,1.));
#23257=DIRECTION('center_axis',(0.,-1.,0.));
#23258=DIRECTION('ref_axis',(1.,0.,0.));
#23259=DIRECTION('center_axis',(0.,1.,0.));
#23260=DIRECTION('ref_axis',(-0.963381374692976,0.,-0.268134904282661));
#23261=DIRECTION('center_axis',(0.,-1.,0.));
#23262=DIRECTION('ref_axis',(0.963381374692962,0.,0.26813490428271));
#23263=DIRECTION('',(-0.703465658964231,0.,0.710729249896204));
#23264=DIRECTION('',(-1.,0.,6.14369354430926E-16));
#23265=DIRECTION('',(-0.703465658964212,0.,-0.710729249896223));
#23266=DIRECTION('center_axis',(0.,-1.,0.));
#23267=DIRECTION('ref_axis',(-0.710729249896308,0.,0.703465658964126));
#23268=DIRECTION('center_axis',(0.,1.,0.));
#23269=DIRECTION('ref_axis',(0.295138112194494,0.,-0.955454601082788));
#23270=DIRECTION('center_axis',(0.,-1.,0.));
#23271=DIRECTION('ref_axis',(-0.295138112194515,0.,0.955454601082782));
#23272=DIRECTION('',(-1.93287220490857E-14,0.,-1.));
#23273=DIRECTION('center_axis',(0.,-1.,0.));
#23274=DIRECTION('ref_axis',(-1.,0.,1.48029736616691E-14));
#23275=DIRECTION('center_axis',(0.,1.,0.));
#23276=DIRECTION('ref_axis',(0.951733868867033,0.,0.306924490471823));
#23277=DIRECTION('center_axis',(0.,-1.,0.));
#23278=DIRECTION('ref_axis',(-0.951733868867053,0.,-0.306924490471762));
#23279=DIRECTION('',(0.702199901316075,0.,-0.711979844231348));
#23280=DIRECTION('center_axis',(1.,0.,0.));
#23281=DIRECTION('ref_axis',(0.,0.,1.));
#23282=DIRECTION('',(0.,0.,1.));
#23283=DIRECTION('center_axis',(1.,0.,0.));
#23284=DIRECTION('ref_axis',(0.,0.,1.));
#23285=DIRECTION('',(0.,0.,1.));
#23286=DIRECTION('',(0.,1.,0.));
#23287=DIRECTION('center_axis',(0.,-1.,0.));
#23288=DIRECTION('ref_axis',(1.,0.,0.));
#23289=DIRECTION('center_axis',(0.,-1.,0.));
#23290=DIRECTION('ref_axis',(1.,0.,0.));
#23291=DIRECTION('',(0.,-1.,0.));
#23292=DIRECTION('center_axis',(0.711979844231348,0.,0.702199901316075));
#23293=DIRECTION('ref_axis',(-0.702199901316075,0.,0.711979844231348));
#23294=DIRECTION('',(-0.702199901316075,0.,0.711979844231348));
#23295=DIRECTION('',(0.,-1.,0.));
#23296=DIRECTION('center_axis',(0.,-1.,0.));
#23297=DIRECTION('ref_axis',(-0.951733868867053,0.,-0.306924490471762));
#23298=DIRECTION('center_axis',(0.,1.,0.));
#23299=DIRECTION('ref_axis',(-0.951733868867053,0.,-0.306924490471762));
#23300=DIRECTION('',(0.,-1.,0.));
#23301=DIRECTION('center_axis',(0.,-1.,0.));
#23302=DIRECTION('ref_axis',(0.951733868867033,0.,0.306924490471823));
#23303=DIRECTION('center_axis',(0.,-1.,0.));
#23304=DIRECTION('ref_axis',(0.951733868867033,0.,0.306924490471823));
#23305=DIRECTION('',(0.,-1.,0.));
#23306=DIRECTION('center_axis',(0.,-1.,0.));
#23307=DIRECTION('ref_axis',(-1.,0.,1.48029736616691E-14));
#23308=DIRECTION('center_axis',(0.,1.,0.));
#23309=DIRECTION('ref_axis',(-1.,0.,1.48029736616691E-14));
#23310=DIRECTION('',(0.,-1.,0.));
#23311=DIRECTION('center_axis',(1.,0.,-1.93287220490857E-14));
#23312=DIRECTION('ref_axis',(1.93287220490857E-14,0.,1.));
#23313=DIRECTION('',(1.93287220490857E-14,0.,1.));
#23314=DIRECTION('',(0.,-1.,0.));
#23315=DIRECTION('center_axis',(0.,-1.,0.));
#23316=DIRECTION('ref_axis',(-0.295138112194515,0.,0.955454601082782));
#23317=DIRECTION('center_axis',(0.,1.,0.));
#23318=DIRECTION('ref_axis',(-0.295138112194515,0.,0.955454601082782));
#23319=DIRECTION('',(0.,-1.,0.));
#23320=DIRECTION('center_axis',(0.,-1.,0.));
#23321=DIRECTION('ref_axis',(0.295138112194494,0.,-0.955454601082788));
#23322=DIRECTION('center_axis',(0.,-1.,0.));
#23323=DIRECTION('ref_axis',(0.295138112194494,0.,-0.955454601082788));
#23324=DIRECTION('',(0.,-1.,0.));
#23325=DIRECTION('center_axis',(0.,-1.,0.));
#23326=DIRECTION('ref_axis',(-0.710729249896308,0.,0.703465658964126));
#23327=DIRECTION('center_axis',(0.,1.,0.));
#23328=DIRECTION('ref_axis',(-0.710729249896308,0.,0.703465658964126));
#23329=DIRECTION('',(0.,-1.,0.));
#23330=DIRECTION('center_axis',(0.710729249896223,0.,-0.703465658964212));
#23331=DIRECTION('ref_axis',(0.703465658964212,0.,0.710729249896223));
#23332=DIRECTION('',(0.703465658964212,0.,0.710729249896223));
#23333=DIRECTION('',(0.,-1.,0.));
#23334=DIRECTION('center_axis',(-6.14369354430926E-16,0.,-1.));
#23335=DIRECTION('ref_axis',(1.,0.,-6.14369354430926E-16));
#23336=DIRECTION('',(1.,0.,-6.14369354430926E-16));
#23337=DIRECTION('',(0.,-1.,0.));
#23338=DIRECTION('center_axis',(-0.710729249896204,0.,-0.703465658964231));
#23339=DIRECTION('ref_axis',(0.703465658964231,0.,-0.710729249896204));
#23340=DIRECTION('',(0.703465658964231,0.,-0.710729249896204));
#23341=DIRECTION('',(0.,-1.,0.));
#23342=DIRECTION('center_axis',(0.,-1.,0.));
#23343=DIRECTION('ref_axis',(0.963381374692962,0.,0.26813490428271));
#23344=DIRECTION('center_axis',(0.,1.,0.));
#23345=DIRECTION('ref_axis',(0.963381374692962,0.,0.26813490428271));
#23346=DIRECTION('',(0.,-1.,0.));
#23347=DIRECTION('center_axis',(0.,-1.,0.));
#23348=DIRECTION('ref_axis',(-0.963381374692976,0.,-0.268134904282661));
#23349=DIRECTION('center_axis',(0.,-1.,0.));
#23350=DIRECTION('ref_axis',(-0.963381374692976,0.,-0.268134904282661));
#23351=DIRECTION('',(0.,-1.,0.));
#23352=DIRECTION('center_axis',(0.,-1.,0.));
#23353=DIRECTION('ref_axis',(1.,0.,0.));
#23354=DIRECTION('center_axis',(0.,1.,0.));
#23355=DIRECTION('ref_axis',(1.,0.,0.));
#23356=DIRECTION('',(0.,-1.,0.));
#23357=DIRECTION('center_axis',(-1.,0.,0.));
#23358=DIRECTION('ref_axis',(0.,0.,-1.));
#23359=DIRECTION('',(0.,0.,-1.));
#23360=DIRECTION('',(0.,-1.,0.));
#23361=DIRECTION('center_axis',(0.,-1.,0.));
#23362=DIRECTION('ref_axis',(0.245760053518526,0.,-0.969330694909932));
#23363=DIRECTION('center_axis',(0.,1.,0.));
#23364=DIRECTION('ref_axis',(0.245760053518526,0.,-0.969330694909932));
#23365=DIRECTION('',(0.,-1.,0.));
#23366=DIRECTION('center_axis',(0.,-1.,0.));
#23367=DIRECTION('ref_axis',(-0.245760053518557,0.,0.969330694909924));
#23368=DIRECTION('center_axis',(0.,-1.,0.));
#23369=DIRECTION('ref_axis',(-0.245760053518557,0.,0.969330694909924));
#23370=DIRECTION('center_axis',(0.,-1.,0.));
#23371=DIRECTION('ref_axis',(1.,0.,0.));
#23372=DIRECTION('axis',(0.,0.,1.));
#23373=DIRECTION('refdir',(1.,0.,0.));
#23374=DIRECTION('center_axis',(0.,0.,1.));
#23375=DIRECTION('ref_axis',(-1.,0.,0.));
#23376=DIRECTION('center_axis',(0.,0.,-1.));
#23377=DIRECTION('ref_axis',(-1.,0.,0.));
#23378=DIRECTION('',(0.,0.,1.));
#23379=DIRECTION('center_axis',(0.,0.,-1.));
#23380=DIRECTION('ref_axis',(-1.,0.,0.));
#23381=DIRECTION('center_axis',(0.,0.,1.));
#23382=DIRECTION('ref_axis',(-1.,0.,0.));
#23383=DIRECTION('center_axis',(0.,0.,-1.));
#23384=DIRECTION('ref_axis',(-1.,0.,0.));
#23385=DIRECTION('center_axis',(-1.22464679914735E-16,1.,0.));
#23386=DIRECTION('ref_axis',(1.,1.22464679914735E-16,0.));
#23387=DIRECTION('center_axis',(0.,0.,1.));
#23388=DIRECTION('ref_axis',(-1.,0.,0.));
#23389=DIRECTION('center_axis',(0.,0.,-1.));
#23390=DIRECTION('ref_axis',(-1.,0.,0.));
#23391=DIRECTION('center_axis',(-1.22464679914735E-16,1.,0.));
#23392=DIRECTION('ref_axis',(1.,1.22464679914735E-16,0.));
#23393=DIRECTION('center_axis',(0.,0.,-1.));
#23394=DIRECTION('ref_axis',(-1.,0.,0.));
#23395=DIRECTION('center_axis',(0.,0.,1.));
#23396=DIRECTION('ref_axis',(-1.,0.,0.));
#23397=DIRECTION('center_axis',(0.,0.,-1.));
#23398=DIRECTION('ref_axis',(-1.,0.,0.));
#23399=DIRECTION('',(-0.777743299254268,-9.52460841990042E-17,-0.628582023657284));
#23400=DIRECTION('center_axis',(0.,0.,1.));
#23401=DIRECTION('ref_axis',(-1.,0.,0.));
#23402=DIRECTION('center_axis',(0.,0.,-1.));
#23403=DIRECTION('ref_axis',(-1.04744440165294E-14,-1.,0.));
#23404=DIRECTION('center_axis',(0.,0.,-1.));
#23405=DIRECTION('ref_axis',(-1.,0.,0.));
#23406=DIRECTION('center_axis',(0.,0.,-1.));
#23407=DIRECTION('ref_axis',(-0.707106781186556,-0.707106781186539,0.));
#23408=DIRECTION('center_axis',(0.,0.,-1.));
#23409=DIRECTION('ref_axis',(-1.,0.,0.));
#23410=DIRECTION('center_axis',(0.,0.,-1.));
#23411=DIRECTION('ref_axis',(-1.,0.,0.));
#23412=DIRECTION('center_axis',(0.,0.,-1.));
#23413=DIRECTION('ref_axis',(-1.,0.,0.));
#23414=DIRECTION('center_axis',(0.,0.,-1.));
#23415=DIRECTION('ref_axis',(-0.707106781186546,0.707106781186549,0.));
#23416=DIRECTION('center_axis',(0.,0.,-1.));
#23417=DIRECTION('ref_axis',(-1.,0.,0.));
#23418=DIRECTION('center_axis',(0.,0.,-1.));
#23419=DIRECTION('ref_axis',(3.49148133884313E-15,1.,0.));
#23420=DIRECTION('center_axis',(1.22464679914735E-16,-1.,0.));
#23421=DIRECTION('ref_axis',(1.,1.22464679914735E-16,0.));
#23422=DIRECTION('center_axis',(0.,0.,-1.));
#23423=DIRECTION('ref_axis',(3.49148133884313E-15,1.,0.));
#23424=DIRECTION('center_axis',(0.,0.,-1.));
#23425=DIRECTION('ref_axis',(-1.,0.,0.));
#23426=DIRECTION('center_axis',(0.,0.,-1.));
#23427=DIRECTION('ref_axis',(0.707106781186551,0.707106781186544,0.));
#23428=DIRECTION('center_axis',(0.,0.,-1.));
#23429=DIRECTION('ref_axis',(-1.,0.,0.));
#23430=DIRECTION('center_axis',(0.,0.,-1.));
#23431=DIRECTION('ref_axis',(1.,0.,0.));
#23432=DIRECTION('center_axis',(0.,0.,-1.));
#23433=DIRECTION('ref_axis',(-1.,0.,0.));
#23434=DIRECTION('center_axis',(0.,0.,-1.));
#23435=DIRECTION('ref_axis',(0.707106781186541,-0.707106781186554,0.));
#23436=DIRECTION('center_axis',(0.,0.,-1.));
#23437=DIRECTION('ref_axis',(-1.,0.,0.));
#23438=DIRECTION('center_axis',(0.,0.,1.));
#23439=DIRECTION('ref_axis',(-1.,0.,0.));
#23440=DIRECTION('center_axis',(0.,0.,-1.));
#23441=DIRECTION('ref_axis',(-1.,0.,0.));
#23442=DIRECTION('',(0.777743299254267,9.5246084199004E-17,0.628582023657285));
#23443=DIRECTION('center_axis',(0.,0.,-1.));
#23444=DIRECTION('ref_axis',(-1.,0.,0.));
#23445=DIRECTION('center_axis',(0.,0.,1.));
#23446=DIRECTION('ref_axis',(-1.,0.,0.));
#23447=DIRECTION('center_axis',(0.,0.,-1.));
#23448=DIRECTION('ref_axis',(-1.,0.,0.));
#23449=DIRECTION('center_axis',(1.22464679914735E-16,-1.,0.));
#23450=DIRECTION('ref_axis',(1.,1.22464679914735E-16,0.));
#23451=DIRECTION('center_axis',(0.,0.,1.));
#23452=DIRECTION('ref_axis',(-1.,0.,0.));
#23453=DIRECTION('center_axis',(-1.22464679914735E-16,1.,0.));
#23454=DIRECTION('ref_axis',(1.,1.22464679914735E-16,0.));
#23455=DIRECTION('center_axis',(0.,0.,1.));
#23456=DIRECTION('ref_axis',(-3.21581820271403E-13,1.,0.));
#23457=DIRECTION('center_axis',(-2.65449697024962E-14,-1.,1.84854068675772E-14));
#23458=DIRECTION('ref_axis',(0.945228043453424,-3.1125259244975E-14,-0.326410701217364));
#23459=DIRECTION('center_axis',(0.,0.,-1.));
#23460=DIRECTION('ref_axis',(-1.,0.,0.));
#23461=DIRECTION('center_axis',(-0.707106781186532,0.707106781186563,-1.36879902392314E-14));
#23462=DIRECTION('ref_axis',(0.241837082303472,0.241837082303443,-0.939696574031161));
#23463=DIRECTION('center_axis',(0.,0.,1.));
#23464=DIRECTION('ref_axis',(-0.707106781186489,0.707106781186606,0.));
#23465=DIRECTION('center_axis',(0.707106781186527,-0.707106781186568,2.46702181021724E-14));
#23466=DIRECTION('ref_axis',(0.668377159293632,0.668377159293584,-0.326410701217368));
#23467=DIRECTION('center_axis',(0.,0.,-1.));
#23468=DIRECTION('ref_axis',(-1.,0.,0.));
#23469=DIRECTION('center_axis',(-1.,-1.65009199484293E-15,1.71165480509254E-15));
#23470=DIRECTION('ref_axis',(-2.1746906207308E-15,0.342009281678289,-0.939696574031161));
#23471=DIRECTION('center_axis',(0.,0.,1.));
#23472=DIRECTION('ref_axis',(-1.,8.08242361927114E-14,0.));
#23473=DIRECTION('center_axis',(1.,-1.15612551933786E-14,1.13714767015716E-14));
#23474=DIRECTION('ref_axis',(1.46383861165231E-14,0.945228043453423,-0.326410701217368));
#23475=DIRECTION('center_axis',(0.,0.,-1.));
#23476=DIRECTION('ref_axis',(-1.,0.,0.));
#23477=DIRECTION('center_axis',(-0.707106781186545,-0.70710678118655,1.49612916568344E-14));
#23478=DIRECTION('ref_axis',(-0.24183708230347,0.241837082303447,-0.939696574031161));
#23479=DIRECTION('center_axis',(0.,0.,1.));
#23480=DIRECTION('ref_axis',(-0.707106781186613,-0.707106781186482,0.));
#23481=DIRECTION('center_axis',(0.707106781186564,0.707106781186531,1.16188769126359E-14));
#23482=DIRECTION('ref_axis',(-0.66837715929359,0.668377159293628,-0.326410701217364));
#23483=DIRECTION('center_axis',(0.,0.,-1.));
#23484=DIRECTION('ref_axis',(-1.,0.,0.));
#23485=DIRECTION('center_axis',(-1.0700730164861E-14,-1.,-6.44787115032575E-17));
#23486=DIRECTION('ref_axis',(-0.342009281678279,3.72415768800159E-15,-0.939696574031164));
#23487=DIRECTION('center_axis',(0.,0.,1.));
#23488=DIRECTION('ref_axis',(-4.98084396431898E-13,-1.,0.));
#23489=DIRECTION('center_axis',(1.02700574112875E-14,1.,-4.88525407613946E-17));
#23490=DIRECTION('ref_axis',(-0.945228043453422,9.69096499636107E-15,-0.326410701217372));
#23491=DIRECTION('center_axis',(0.,0.,-1.));
#23492=DIRECTION('ref_axis',(-1.,0.,0.));
#23493=DIRECTION('center_axis',(0.707106781186529,-0.707106781186566,-1.90995212640436E-14));
#23494=DIRECTION('ref_axis',(-0.241837082303473,-0.241837082303435,-0.939696574031163));
#23495=DIRECTION('center_axis',(0.,0.,1.));
#23496=DIRECTION('ref_axis',(0.707106781186484,-0.707106781186611,0.));
#23497=DIRECTION('center_axis',(-0.707106781186538,0.707106781186557,4.77488092300106E-15));
#23498=DIRECTION('ref_axis',(-0.668377159293619,-0.6683771592936,-0.326410701217363));
#23499=DIRECTION('center_axis',(0.,0.,-1.));
#23500=DIRECTION('ref_axis',(-1.,0.,0.));
#23501=DIRECTION('center_axis',(1.,1.79398764678015E-15,1.76453926386396E-15));
#23502=DIRECTION('ref_axis',(2.26983333538778E-15,-0.342009281678289,-0.939696574031161));
#23503=DIRECTION('center_axis',(0.,0.,1.));
#23504=DIRECTION('ref_axis',(1.,-8.08242361927114E-14,0.));
#23505=DIRECTION('center_axis',(-1.,-7.91804511680167E-15,-7.69942093215295E-15));
#23506=DIRECTION('ref_axis',(1.00035767704373E-14,-0.945228043453423,-0.326410701217368));
#23507=DIRECTION('center_axis',(0.,0.,-1.));
#23508=DIRECTION('ref_axis',(-1.,0.,0.));
#23509=DIRECTION('center_axis',(0.707106781186536,0.707106781186559,1.97361719728453E-14));
#23510=DIRECTION('ref_axis',(0.241837082303476,-0.241837082303441,-0.939696574031161));
#23511=DIRECTION('center_axis',(0.,0.,1.));
#23512=DIRECTION('ref_axis',(0.707106781186608,0.707106781186487,0.));
#23513=DIRECTION('center_axis',(-0.707106781186538,-0.707106781186557,-2.18052895483717E-14));
#23514=DIRECTION('ref_axis',(0.668377159293621,-0.668377159293593,-0.326410701217372));
#23515=DIRECTION('center_axis',(0.,0.,-1.));
#23516=DIRECTION('ref_axis',(-1.,0.,0.));
#23517=DIRECTION('center_axis',(-6.13527734841807E-15,1.,1.38135285440519E-14));
#23518=DIRECTION('ref_axis',(0.342009281678287,1.50733243649404E-14,-0.939696574031162));
#23519=DIRECTION('center_axis',(0.,0.,1.));
#23520=DIRECTION('ref_axis',(-3.21581820271403E-13,1.,0.));
#23521=DIRECTION('center_axis',(0.,0.,1.));
#23522=DIRECTION('ref_axis',(-1.,0.,0.));
#23523=DIRECTION('',(0.664464832747924,-0.664464832747934,0.34201311682819));
#23524=DIRECTION('center_axis',(0.,0.,-1.));
#23525=DIRECTION('ref_axis',(-1.,0.,0.));
#23526=DIRECTION('',(-0.93969517819209,3.34165038880862E-15,-0.342013116828193));
#23527=DIRECTION('center_axis',(0.,0.,1.));
#23528=DIRECTION('ref_axis',(-1.,0.,0.));
#23529=DIRECTION('center_axis',(0.,0.,-1.));
#23530=DIRECTION('ref_axis',(-1.,0.,0.));
#23531=DIRECTION('',(-0.664464832747918,-0.664464832747939,-0.342013116828193));
#23532=DIRECTION('',(0.93969517819209,-3.2601467207889E-15,0.342013116828193));
#23533=DIRECTION('center_axis',(0.,0.,1.));
#23534=DIRECTION('ref_axis',(-1.,0.,0.));
#23535=DIRECTION('',(8.15036680197226E-17,-0.93969517819209,0.342013116828193));
#23536=DIRECTION('center_axis',(0.,0.,-1.));
#23537=DIRECTION('ref_axis',(-1.,0.,0.));
#23538=DIRECTION('',(-0.664464832747928,0.664464832747928,-0.342013116828193));
#23539=DIRECTION('center_axis',(0.,0.,1.));
#23540=DIRECTION('ref_axis',(-1.,0.,0.));
#23541=DIRECTION('',(-0.66446483274794,-0.664464832747919,0.342013116828188));
#23542=DIRECTION('center_axis',(0.,0.,-1.));
#23543=DIRECTION('ref_axis',(-1.,0.,0.));
#23544=DIRECTION('',(8.15036680197226E-17,0.93969517819209,-0.342013116828193));
#23545=DIRECTION('center_axis',(0.,0.,1.));
#23546=DIRECTION('ref_axis',(-1.,0.,0.));
#23547=DIRECTION('',(-0.93969517819209,9.78044016236671E-15,0.342013116828193));
#23548=DIRECTION('center_axis',(0.,0.,-1.));
#23549=DIRECTION('ref_axis',(-1.,0.,0.));
#23550=DIRECTION('',(0.664464832747934,0.664464832747924,-0.34201311682819));
#23551=DIRECTION('center_axis',(0.,0.,1.));
#23552=DIRECTION('ref_axis',(-1.,0.,0.));
#23553=DIRECTION('',(-0.664464832747918,0.664464832747939,0.342013116828193));
#23554=DIRECTION('center_axis',(0.,0.,-1.));
#23555=DIRECTION('ref_axis',(-1.,0.,0.));
#23556=DIRECTION('',(0.939695178192092,-9.94344749840606E-15,-0.34201311682819));
#23557=DIRECTION('center_axis',(0.,0.,1.));
#23558=DIRECTION('ref_axis',(-1.,0.,0.));
#23559=DIRECTION('',(-8.15036680197226E-17,0.93969517819209,0.342013116828193));
#23560=DIRECTION('center_axis',(0.,0.,-1.));
#23561=DIRECTION('ref_axis',(-1.,0.,0.));
#23562=DIRECTION('',(0.664464832747918,-0.664464832747939,-0.342013116828193));
#23563=DIRECTION('center_axis',(0.,0.,1.));
#23564=DIRECTION('ref_axis',(-1.,0.,0.));
#23565=DIRECTION('center_axis',(0.,0.,-1.));
#23566=DIRECTION('ref_axis',(-1.,0.,0.));
#23567=DIRECTION('',(-8.15036680197226E-17,-0.93969517819209,-0.342013116828193));
#23568=DIRECTION('',(0.664464832747934,0.664464832747924,0.34201311682819));
#23569=DIRECTION('center_axis',(0.,0.,-1.));
#23570=DIRECTION('ref_axis',(1.,0.,0.));
#23571=DIRECTION('',(0.241849828089742,-0.241849828089742,-0.939690013411829));
#23572=DIRECTION('center_axis',(0.,0.,-1.));
#23573=DIRECTION('ref_axis',(-1.,0.,0.));
#23574=DIRECTION('',(-0.342027306942117,1.29765967489722E-15,0.939690013411829));
#23575=DIRECTION('center_axis',(0.,0.,-1.));
#23576=DIRECTION('ref_axis',(1.,0.,0.));
#23577=DIRECTION('center_axis',(0.,0.,-1.));
#23578=DIRECTION('ref_axis',(-1.,0.,0.));
#23579=DIRECTION('',(-0.241849828089751,-0.241849828089742,0.939690013411827));
#23580=DIRECTION('',(0.342027306942117,-1.08138306241435E-15,-0.939690013411829));
#23581=DIRECTION('center_axis',(0.,0.,-1.));
#23582=DIRECTION('ref_axis',(1.,0.,0.));
#23583=DIRECTION('',(7.20922041609565E-17,-0.342027306942117,-0.939690013411829));
#23584=DIRECTION('center_axis',(0.,0.,-1.));
#23585=DIRECTION('ref_axis',(-1.,0.,0.));
#23586=DIRECTION('',(-0.241849828089734,0.241849828089743,0.939690013411832));
#23587=DIRECTION('center_axis',(0.,0.,-1.));
#23588=DIRECTION('ref_axis',(1.,0.,0.));
#23589=DIRECTION('',(-0.241849828089734,-0.241849828089743,-0.939690013411832));
#23590=DIRECTION('center_axis',(0.,0.,-1.));
#23591=DIRECTION('ref_axis',(-1.,0.,0.));
#23592=DIRECTION('',(7.20922041609565E-17,0.342027306942117,0.939690013411829));
#23593=DIRECTION('center_axis',(0.,0.,-1.));
#23594=DIRECTION('ref_axis',(1.,0.,0.));
#23595=DIRECTION('',(-0.342027306942125,3.4604257997259E-15,-0.939690013411826));
#23596=DIRECTION('center_axis',(0.,0.,-1.));
#23597=DIRECTION('ref_axis',(-1.,0.,0.));
#23598=DIRECTION('',(0.241849828089751,0.241849828089742,0.939690013411827));
#23599=DIRECTION('center_axis',(0.,0.,-1.));
#23600=DIRECTION('ref_axis',(1.,0.,0.));
#23601=DIRECTION('',(-0.241849828089742,0.241849828089751,-0.939690013411827));
#23602=DIRECTION('center_axis',(0.,0.,-1.));
#23603=DIRECTION('ref_axis',(-1.,0.,0.));
#23604=DIRECTION('',(0.342027306942117,-3.74879461636974E-15,0.939690013411829));
#23605=DIRECTION('center_axis',(0.,0.,-1.));
#23606=DIRECTION('ref_axis',(1.,0.,0.));
#23607=DIRECTION('',(-7.20922041609565E-17,0.342027306942117,-0.939690013411829));
#23608=DIRECTION('center_axis',(0.,0.,-1.));
#23609=DIRECTION('ref_axis',(-1.,0.,0.));
#23610=DIRECTION('',(0.241849828089733,-0.241849828089752,0.939690013411829));
#23611=DIRECTION('center_axis',(0.,0.,-1.));
#23612=DIRECTION('ref_axis',(1.,0.,0.));
#23613=DIRECTION('center_axis',(0.,0.,-1.));
#23614=DIRECTION('ref_axis',(-1.,0.,0.));
#23615=DIRECTION('',(-7.20922041609565E-17,-0.342027306942117,0.939690013411829));
#23616=DIRECTION('',(0.241849828089734,0.241849828089743,-0.939690013411832));
#23617=DIRECTION('center_axis',(0.,0.,1.));
#23618=DIRECTION('ref_axis',(-1.,0.,0.));
#23619=DIRECTION('',(-0.405586087801291,0.405586087801293,-0.819145805558501));
#23620=DIRECTION('',(0.573585346078431,-2.07701987415471E-15,0.819145805558501));
#23621=DIRECTION('center_axis',(0.,0.,1.));
#23622=DIRECTION('ref_axis',(-1.,0.,0.));
#23623=DIRECTION('',(0.405586087801295,0.405586087801293,0.819145805558499));
#23624=DIRECTION('',(-0.573585346078431,1.91898575329511E-15,-0.819145805558501));
#23625=DIRECTION('center_axis',(0.,0.,1.));
#23626=DIRECTION('ref_axis',(-1.,0.,0.));
#23627=DIRECTION('',(-6.77289089398275E-17,0.573585346078431,-0.819145805558501));
#23628=DIRECTION('',(0.405586087801291,-0.405586087801293,0.819145805558501));
#23629=DIRECTION('center_axis',(0.,0.,1.));
#23630=DIRECTION('ref_axis',(-1.,0.,0.));
#23631=DIRECTION('',(0.405586087801294,0.405586087801288,-0.819145805558502));
#23632=DIRECTION('',(-9.030521191977E-17,-0.573585346078431,0.819145805558501));
#23633=DIRECTION('center_axis',(0.,0.,1.));
#23634=DIRECTION('ref_axis',(-1.,0.,0.));
#23635=DIRECTION('',(0.573585346078431,-5.93756768372488E-15,-0.819145805558501));
#23636=DIRECTION('',(-0.405586087801298,-0.40558608780129,0.819145805558499));
#23637=DIRECTION('center_axis',(0.,0.,1.));
#23638=DIRECTION('ref_axis',(-1.,0.,0.));
#23639=DIRECTION('',(0.405586087801288,-0.405586087801296,-0.819145805558501));
#23640=DIRECTION('',(-0.573585346078433,6.11817810756441E-15,0.8191458055585));
#23641=DIRECTION('center_axis',(0.,0.,1.));
#23642=DIRECTION('ref_axis',(-1.,0.,0.));
#23643=DIRECTION('',(6.77289089398275E-17,-0.573585346078431,-0.819145805558501));
#23644=DIRECTION('',(-0.405586087801287,0.405586087801299,0.8191458055585));
#23645=DIRECTION('center_axis',(0.,0.,1.));
#23646=DIRECTION('ref_axis',(-1.,0.,0.));
#23647=DIRECTION('',(9.030521191977E-17,0.573585346078431,0.819145805558501));
#23648=DIRECTION('',(-0.405586087801294,-0.405586087801288,-0.819145805558502));
#23649=DIRECTION('center_axis',(0.,0.,-1.));
#23650=DIRECTION('ref_axis',(1.,0.,0.));
#23651=DIRECTION('center_axis',(0.,0.,1.));
#23652=DIRECTION('ref_axis',(-1.,0.,0.));
#23653=DIRECTION('center_axis',(-1.,1.27191845719472E-16,0.));
#23654=DIRECTION('ref_axis',(-1.27191845719472E-16,-1.,0.));
#23655=DIRECTION('',(1.27191845719472E-16,1.,0.));
#23656=DIRECTION('center_axis',(1.,1.27191845719472E-16,0.));
#23657=DIRECTION('ref_axis',(-1.27191845719472E-16,1.,0.));
#23658=DIRECTION('',(1.27191845719472E-16,-1.,0.));
#23659=DIRECTION('center_axis',(0.,0.,1.));
#23660=DIRECTION('ref_axis',(-1.,0.,0.));
#23661=DIRECTION('center_axis',(-0.707106781186546,0.707106781186549,0.));
#23662=DIRECTION('ref_axis',(-0.707106781186549,-0.707106781186546,0.));
#23663=DIRECTION('',(0.707106781186549,0.707106781186546,0.));
#23664=DIRECTION('center_axis',(0.707106781186546,-0.707106781186549,0.));
#23665=DIRECTION('ref_axis',(0.707106781186549,0.707106781186546,0.));
#23666=DIRECTION('',(-0.707106781186549,-0.707106781186546,0.));
#23667=DIRECTION('center_axis',(0.,0.,1.));
#23668=DIRECTION('ref_axis',(-0.707106781186546,0.707106781186549,0.));
#23669=DIRECTION('center_axis',(-0.707106781186556,-0.707106781186539,0.));
#23670=DIRECTION('ref_axis',(0.707106781186539,-0.707106781186556,0.));
#23671=DIRECTION('',(-0.707106781186539,0.707106781186556,0.));
#23672=DIRECTION('center_axis',(0.707106781186556,0.707106781186539,0.));
#23673=DIRECTION('ref_axis',(-0.707106781186539,0.707106781186556,0.));
#23674=DIRECTION('',(0.707106781186539,-0.707106781186556,0.));
#23675=DIRECTION('center_axis',(0.,0.,1.));
#23676=DIRECTION('ref_axis',(-0.707106781186556,-0.707106781186539,0.));
#23677=DIRECTION('center_axis',(-1.06016358622489E-14,-1.,0.));
#23678=DIRECTION('ref_axis',(1.,-1.06016358622489E-14,0.));
#23679=DIRECTION('',(-1.,1.06016358622489E-14,0.));
#23680=DIRECTION('center_axis',(1.03472521708099E-14,1.,0.));
#23681=DIRECTION('ref_axis',(-1.,1.03472521708099E-14,0.));
#23682=DIRECTION('',(1.,-1.03472521708099E-14,0.));
#23683=DIRECTION('center_axis',(0.,0.,1.));
#23684=DIRECTION('ref_axis',(-1.04744440165294E-14,-1.,0.));
#23685=DIRECTION('center_axis',(0.707106781186541,-0.707106781186554,0.));
#23686=DIRECTION('ref_axis',(0.707106781186554,0.707106781186541,0.));
#23687=DIRECTION('',(-0.707106781186554,-0.707106781186541,0.));
#23688=DIRECTION('center_axis',(-0.707106781186541,0.707106781186554,0.));
#23689=DIRECTION('ref_axis',(-0.707106781186554,-0.707106781186541,0.));
#23690=DIRECTION('',(0.707106781186554,0.707106781186541,0.));
#23691=DIRECTION('center_axis',(0.,0.,1.));
#23692=DIRECTION('ref_axis',(0.707106781186541,-0.707106781186554,0.));
#23693=DIRECTION('center_axis',(1.,-1.27191845719472E-16,0.));
#23694=DIRECTION('ref_axis',(1.27191845719472E-16,1.,0.));
#23695=DIRECTION('',(-1.27191845719472E-16,-1.,0.));
#23696=DIRECTION('center_axis',(-1.,-1.27191845719472E-16,0.));
#23697=DIRECTION('ref_axis',(1.27191845719472E-16,-1.,0.));
#23698=DIRECTION('',(-1.27191845719472E-16,1.,0.));
#23699=DIRECTION('center_axis',(0.,0.,1.));
#23700=DIRECTION('ref_axis',(1.,0.,0.));
#23701=DIRECTION('center_axis',(0.707106781186551,0.707106781186544,0.));
#23702=DIRECTION('ref_axis',(-0.707106781186544,0.707106781186551,0.));
#23703=DIRECTION('',(0.707106781186544,-0.707106781186551,0.));
#23704=DIRECTION('center_axis',(-0.707106781186551,-0.707106781186544,0.));
#23705=DIRECTION('ref_axis',(0.707106781186544,-0.707106781186551,0.));
#23706=DIRECTION('',(-0.707106781186544,0.707106781186551,0.));
#23707=DIRECTION('center_axis',(0.,0.,1.));
#23708=DIRECTION('ref_axis',(0.707106781186551,0.707106781186544,0.));
#23709=DIRECTION('center_axis',(3.61867318456261E-15,1.,0.));
#23710=DIRECTION('ref_axis',(-1.,3.61867318456261E-15,0.));
#23711=DIRECTION('',(1.,-3.61867318456261E-15,0.));
#23712=DIRECTION('center_axis',(-3.36428949312366E-15,-1.,0.));
#23713=DIRECTION('ref_axis',(1.,-3.36428949312366E-15,0.));
#23714=DIRECTION('',(-1.,3.36428949312366E-15,0.));
#23715=DIRECTION('center_axis',(0.,0.,1.));
#23716=DIRECTION('ref_axis',(3.49148133884313E-15,1.,0.));
#23717=DIRECTION('center_axis',(1.,0.,6.12323399573677E-17));
#23718=DIRECTION('ref_axis',(0.,0.,1.));
#23719=DIRECTION('center_axis',(0.,1.,0.));
#23720=DIRECTION('ref_axis',(0.,0.,-1.));
#23721=DIRECTION('center_axis',(0.,0.,1.));
#23722=DIRECTION('ref_axis',(1.,0.,0.));
#23723=DIRECTION('center_axis',(0.,0.,-1.));
#23724=DIRECTION('ref_axis',(-1.,0.,0.));
#23725=DIRECTION('center_axis',(-1.22464679914735E-16,1.,0.));
#23726=DIRECTION('ref_axis',(-1.,-1.22464679914735E-16,0.));
#23727=DIRECTION('center_axis',(0.,0.,1.));
#23728=DIRECTION('ref_axis',(1.,0.,0.));
#23729=DIRECTION('center_axis',(0.,0.,1.));
#23730=DIRECTION('ref_axis',(1.,0.,0.));
#23731=DIRECTION('center_axis',(0.,0.,1.));
#23732=DIRECTION('ref_axis',(1.,0.,0.));
#23733=DIRECTION('center_axis',(1.22464679914735E-16,-1.,0.));
#23734=DIRECTION('ref_axis',(-1.,-1.22464679914735E-16,0.));
#23735=DIRECTION('center_axis',(0.,0.,1.));
#23736=DIRECTION('ref_axis',(1.,0.,0.));
#23737=DIRECTION('center_axis',(0.,0.,1.));
#23738=DIRECTION('ref_axis',(1.,0.,0.));
#23739=DIRECTION('center_axis',(0.,0.,-1.));
#23740=DIRECTION('ref_axis',(-1.,0.,0.));
#23741=DIRECTION('center_axis',(0.,0.,1.));
#23742=DIRECTION('ref_axis',(1.,0.,0.));
#23743=DIRECTION('',(0.12186934340514,-1.49246901315294E-17,-0.992546151641323));
#23744=DIRECTION('center_axis',(0.,0.,1.));
#23745=DIRECTION('ref_axis',(1.,0.,0.));
#23746=DIRECTION('center_axis',(0.,0.,1.));
#23747=DIRECTION('ref_axis',(1.,0.,0.));
#23748=DIRECTION('',(0.,0.,1.));
#23749=DIRECTION('center_axis',(0.,0.,1.));
#23750=DIRECTION('ref_axis',(1.,0.,0.));
#23751=DIRECTION('center_axis',(0.,0.,1.));
#23752=DIRECTION('ref_axis',(1.,0.,0.));
#23753=DIRECTION('',(-0.12186934340514,-1.49246901315294E-17,0.992546151641323));
#23754=DIRECTION('center_axis',(0.,0.,1.));
#23755=DIRECTION('ref_axis',(1.,0.,0.));
#23756=DIRECTION('center_axis',(0.,0.,1.));
#23757=DIRECTION('ref_axis',(1.,0.,0.));
#23758=DIRECTION('center_axis',(1.22464679914735E-16,-1.,0.));
#23759=DIRECTION('ref_axis',(-1.,-1.22464679914735E-16,0.));
#23760=DIRECTION('center_axis',(0.,0.,1.));
#23761=DIRECTION('ref_axis',(1.,0.,0.));
#23762=DIRECTION('center_axis',(0.,0.,1.));
#23763=DIRECTION('ref_axis',(1.,0.,0.));
#23764=DIRECTION('center_axis',(0.,0.,1.));
#23765=DIRECTION('ref_axis',(1.,0.,0.));
#23766=DIRECTION('center_axis',(1.22464679914735E-16,-1.,0.));
#23767=DIRECTION('ref_axis',(-1.,-1.22464679914735E-16,0.));
#23768=DIRECTION('center_axis',(0.,0.,1.));
#23769=DIRECTION('ref_axis',(1.,0.,0.));
#23770=DIRECTION('center_axis',(0.,0.,1.));
#23771=DIRECTION('ref_axis',(1.,0.,0.));
#23772=DIRECTION('center_axis',(0.,0.,1.));
#23773=DIRECTION('ref_axis',(1.,0.,0.));
#23774=DIRECTION('center_axis',(1.22464679914735E-16,-1.,0.));
#23775=DIRECTION('ref_axis',(-1.,-1.22464679914735E-16,0.));
#23776=DIRECTION('center_axis',(0.,0.,1.));
#23777=DIRECTION('ref_axis',(1.,0.,0.));
#23778=DIRECTION('center_axis',(0.,0.,1.));
#23779=DIRECTION('ref_axis',(1.,0.,0.));
#23780=DIRECTION('',(0.,0.,-1.));
#23781=DIRECTION('center_axis',(0.,0.,1.));
#23782=DIRECTION('ref_axis',(1.,0.,0.));
#23783=DIRECTION('',(0.,0.,-1.));
#23784=DIRECTION('center_axis',(0.,0.,-1.));
#23785=DIRECTION('ref_axis',(-1.,0.,0.));
#23786=DIRECTION('center_axis',(0.,0.,1.));
#23787=DIRECTION('ref_axis',(1.,0.,0.));
#23788=DIRECTION('center_axis',(0.,0.,1.));
#23789=DIRECTION('ref_axis',(1.,0.,0.));
#23790=DIRECTION('center_axis',(0.,0.,-1.));
#23791=DIRECTION('ref_axis',(1.,0.,0.));
#23792=DIRECTION('center_axis',(-1.22464679914735E-16,1.,0.));
#23793=DIRECTION('ref_axis',(-1.,-1.22464679914735E-16,0.));
#23794=DIRECTION('center_axis',(0.,0.,1.));
#23795=DIRECTION('ref_axis',(-1.,0.,0.));
#23796=DIRECTION('center_axis',(0.,0.,1.));
#23797=DIRECTION('ref_axis',(1.,0.,0.));
#23798=DIRECTION('center_axis',(0.,0.,1.));
#23799=DIRECTION('ref_axis',(1.,0.,0.));
#23800=DIRECTION('',(0.,0.,-1.));
#23801=DIRECTION('center_axis',(0.,0.,1.));
#23802=DIRECTION('ref_axis',(1.,0.,0.));
#23803=DIRECTION('center_axis',(0.,0.,1.));
#23804=DIRECTION('ref_axis',(1.,0.,0.));
#23805=DIRECTION('center_axis',(1.22464679914735E-16,-1.,0.));
#23806=DIRECTION('ref_axis',(-1.,-1.22464679914735E-16,0.));
#23807=DIRECTION('center_axis',(0.,0.,1.));
#23808=DIRECTION('ref_axis',(1.,0.,0.));
#23809=DIRECTION('center_axis',(0.,0.,1.));
#23810=DIRECTION('ref_axis',(1.,0.,0.));
#23811=DIRECTION('',(0.992546151641321,1.21551846761357E-16,-0.121869343405157));
#23812=DIRECTION('center_axis',(0.,0.,1.));
#23813=DIRECTION('ref_axis',(1.,0.,0.));
#23814=DIRECTION('center_axis',(0.,0.,-1.));
#23815=DIRECTION('ref_axis',(-1.,0.,0.));
#23816=DIRECTION('center_axis',(0.,0.,1.));
#23817=DIRECTION('ref_axis',(1.,0.,0.));
#23818=DIRECTION('',(-0.992546151641322,1.21551846761357E-16,0.121869343405149));
#23819=DIRECTION('center_axis',(0.,0.,1.));
#23820=DIRECTION('ref_axis',(1.,0.,0.));
#23821=DIRECTION('center_axis',(0.,0.,1.));
#23822=DIRECTION('ref_axis',(1.,0.,0.));
#23823=DIRECTION('center_axis',(0.,0.,1.));
#23824=DIRECTION('ref_axis',(1.,0.,0.));
#23825=DIRECTION('center_axis',(1.22464679914735E-16,-1.,0.));
#23826=DIRECTION('ref_axis',(-1.,-1.22464679914735E-16,0.));
#23827=DIRECTION('center_axis',(0.,0.,1.));
#23828=DIRECTION('ref_axis',(1.,0.,0.));
#23829=DIRECTION('center_axis',(0.,0.,1.));
#23830=DIRECTION('ref_axis',(1.,0.,0.));
#23831=DIRECTION('',(0.,0.,1.));
#23832=DIRECTION('center_axis',(0.,0.,1.));
#23833=DIRECTION('ref_axis',(1.,0.,0.));
#23834=DIRECTION('',(0.,0.,1.));
#23835=DIRECTION('center_axis',(0.,0.,1.));
#23836=DIRECTION('ref_axis',(1.,0.,0.));
#23837=DIRECTION('center_axis',(0.,0.,-1.));
#23838=DIRECTION('ref_axis',(-1.,0.,0.));
#23839=DIRECTION('center_axis',(0.,0.,1.));
#23840=DIRECTION('ref_axis',(1.,0.,0.));
#23841=DIRECTION('center_axis',(0.707106781186546,-0.707106781186549,6.12323399573677E-17));
#23842=DIRECTION('ref_axis',(0.,0.,1.));
#23843=DIRECTION('center_axis',(0.707106781186549,0.707106781186546,0.));
#23844=DIRECTION('ref_axis',(0.,0.,-1.));
#23845=DIRECTION('center_axis',(-3.71222327254256E-15,-1.,6.12323399573677E-17));
#23846=DIRECTION('ref_axis',(0.,0.,1.));
#23847=DIRECTION('center_axis',(1.,-3.49148133884313E-15,0.));
#23848=DIRECTION('ref_axis',(0.,0.,-1.));
#23849=DIRECTION('center_axis',(-0.707106781186551,-0.707106781186544,6.12323399573676E-17));
#23850=DIRECTION('ref_axis',(0.,0.,1.));
#23851=DIRECTION('center_axis',(0.707106781186544,-0.707106781186551,0.));
#23852=DIRECTION('ref_axis',(0.,0.,-1.));
#23853=DIRECTION('center_axis',(-1.,0.,6.12323399573677E-17));
#23854=DIRECTION('ref_axis',(0.,0.,1.));
#23855=DIRECTION('center_axis',(0.,-1.,0.));
#23856=DIRECTION('ref_axis',(0.,0.,-1.));
#23857=DIRECTION('center_axis',(-0.707106781186541,0.707106781186554,6.12323399573677E-17));
#23858=DIRECTION('ref_axis',(0.,0.,1.));
#23859=DIRECTION('center_axis',(-0.707106781186554,-0.707106781186541,0.));
#23860=DIRECTION('ref_axis',(0.,0.,-1.));
#23861=DIRECTION('center_axis',(1.06726419085599E-14,1.,6.12323399573677E-17));
#23862=DIRECTION('ref_axis',(0.,0.,1.));
#23863=DIRECTION('center_axis',(-1.,1.04744440165294E-14,0.));
#23864=DIRECTION('ref_axis',(0.,0.,-1.));
#23865=DIRECTION('center_axis',(0.707106781186556,0.707106781186539,6.12323399573677E-17));
#23866=DIRECTION('ref_axis',(0.,0.,1.));
#23867=DIRECTION('center_axis',(-0.707106781186539,0.707106781186556,0.));
#23868=DIRECTION('ref_axis',(0.,0.,-1.));
#23869=DIRECTION('center_axis',(0.,0.,1.));
#23870=DIRECTION('ref_axis',(1.,0.,0.));
#23871=DIRECTION('center_axis',(0.,0.,1.));
#23872=DIRECTION('ref_axis',(-1.,0.,0.));
#23873=DIRECTION('center_axis',(0.,0.,1.));
#23874=DIRECTION('ref_axis',(-1.,0.,0.));
#23875=DIRECTION('center_axis',(-1.22464679914735E-16,1.,0.));
#23876=DIRECTION('ref_axis',(-1.,-1.22464679914735E-16,0.));
#23877=DIRECTION('center_axis',(0.,0.,-1.));
#23878=DIRECTION('ref_axis',(-1.,0.,0.));
#23879=DIRECTION('center_axis',(0.,0.,-1.));
#23880=DIRECTION('ref_axis',(-1.,0.,0.));
#23881=DIRECTION('center_axis',(0.,0.,-1.));
#23882=DIRECTION('ref_axis',(-1.,0.,0.));
#23883=DIRECTION('center_axis',(0.,0.,-1.));
#23884=DIRECTION('ref_axis',(-1.,0.,0.));
#23885=DIRECTION('',(0.,0.,-1.));
#23886=DIRECTION('center_axis',(0.,0.,-1.));
#23887=DIRECTION('ref_axis',(-1.,0.,0.));
#23888=DIRECTION('center_axis',(0.,0.,-1.));
#23889=DIRECTION('ref_axis',(-1.,0.,0.));
#23890=DIRECTION('center_axis',(0.,0.,-1.));
#23891=DIRECTION('ref_axis',(-1.,0.,0.));
#23892=DIRECTION('center_axis',(-1.22464679914735E-16,-1.,0.));
#23893=DIRECTION('ref_axis',(1.,-1.22464679914735E-16,0.));
#23894=DIRECTION('center_axis',(0.,0.,-1.));
#23895=DIRECTION('ref_axis',(-1.,0.,0.));
#23896=DIRECTION('center_axis',(0.,0.,-1.));
#23897=DIRECTION('ref_axis',(-1.,0.,0.));
#23898=DIRECTION('center_axis',(-1.22464679914735E-16,-1.,0.));
#23899=DIRECTION('ref_axis',(1.,-1.22464679914735E-16,0.));
#23900=DIRECTION('center_axis',(0.,0.,-1.));
#23901=DIRECTION('ref_axis',(-1.,0.,0.));
#23902=DIRECTION('center_axis',(0.,0.,-1.));
#23903=DIRECTION('ref_axis',(-1.,0.,0.));
#23904=DIRECTION('center_axis',(0.,0.,-1.));
#23905=DIRECTION('ref_axis',(-1.,0.,0.));
#23906=DIRECTION('',(-0.777743299254268,9.52460841990042E-17,0.628582023657284));
#23907=DIRECTION('center_axis',(0.,0.,-1.));
#23908=DIRECTION('ref_axis',(-1.,0.,0.));
#23909=DIRECTION('center_axis',(0.,0.,-1.));
#23910=DIRECTION('ref_axis',(-1.04744440165294E-14,-1.,0.));
#23911=DIRECTION('center_axis',(0.,0.,-1.));
#23912=DIRECTION('ref_axis',(-1.,0.,0.));
#23913=DIRECTION('center_axis',(0.,0.,-1.));
#23914=DIRECTION('ref_axis',(0.707106781186541,-0.707106781186554,0.));
#23915=DIRECTION('center_axis',(0.,0.,-1.));
#23916=DIRECTION('ref_axis',(-1.,0.,0.));
#23917=DIRECTION('center_axis',(0.,0.,-1.));
#23918=DIRECTION('ref_axis',(1.,0.,0.));
#23919=DIRECTION('center_axis',(0.,0.,-1.));
#23920=DIRECTION('ref_axis',(-1.,0.,0.));
#23921=DIRECTION('center_axis',(0.,0.,-1.));
#23922=DIRECTION('ref_axis',(0.707106781186551,0.707106781186544,0.));
#23923=DIRECTION('center_axis',(0.,0.,-1.));
#23924=DIRECTION('ref_axis',(-1.,0.,0.));
#23925=DIRECTION('center_axis',(0.,0.,-1.));
#23926=DIRECTION('ref_axis',(3.49148133884313E-15,1.,0.));
#23927=DIRECTION('center_axis',(1.22464679914735E-16,1.,0.));
#23928=DIRECTION('ref_axis',(1.,-1.22464679914735E-16,0.));
#23929=DIRECTION('center_axis',(0.,0.,-1.));
#23930=DIRECTION('ref_axis',(3.49148133884313E-15,1.,0.));
#23931=DIRECTION('center_axis',(0.,0.,-1.));
#23932=DIRECTION('ref_axis',(-1.,0.,0.));
#23933=DIRECTION('center_axis',(0.,0.,-1.));
#23934=DIRECTION('ref_axis',(-0.707106781186546,0.707106781186549,0.));
#23935=DIRECTION('center_axis',(0.,0.,-1.));
#23936=DIRECTION('ref_axis',(-1.,0.,0.));
#23937=DIRECTION('center_axis',(0.,0.,-1.));
#23938=DIRECTION('ref_axis',(-1.,0.,0.));
#23939=DIRECTION('center_axis',(0.,0.,-1.));
#23940=DIRECTION('ref_axis',(-1.,0.,0.));
#23941=DIRECTION('center_axis',(0.,0.,-1.));
#23942=DIRECTION('ref_axis',(-0.707106781186556,-0.707106781186539,0.));
#23943=DIRECTION('center_axis',(0.,0.,-1.));
#23944=DIRECTION('ref_axis',(-1.,0.,0.));
#23945=DIRECTION('center_axis',(0.,0.,-1.));
#23946=DIRECTION('ref_axis',(-1.,0.,0.));
#23947=DIRECTION('center_axis',(0.,0.,-1.));
#23948=DIRECTION('ref_axis',(-1.,0.,0.));
#23949=DIRECTION('center_axis',(1.22464679914735E-16,1.,0.));
#23950=DIRECTION('ref_axis',(1.,-1.22464679914735E-16,0.));
#23951=DIRECTION('center_axis',(0.,0.,-1.));
#23952=DIRECTION('ref_axis',(-1.,0.,0.));
#23953=DIRECTION('center_axis',(0.,0.,-1.));
#23954=DIRECTION('ref_axis',(-1.,0.,0.));
#23955=DIRECTION('',(0.777743299254267,-9.5246084199004E-17,-0.628582023657285));
#23956=DIRECTION('center_axis',(0.,0.,-1.));
#23957=DIRECTION('ref_axis',(-1.,0.,0.));
#23958=DIRECTION('center_axis',(-1.22464679914735E-16,-1.,0.));
#23959=DIRECTION('ref_axis',(1.,-1.22464679914735E-16,0.));
#23960=DIRECTION('center_axis',(0.,0.,1.));
#23961=DIRECTION('ref_axis',(3.28564782949089E-13,1.,0.));
#23962=DIRECTION('center_axis',(6.13527734841807E-15,-1.,1.38135285440519E-14));
#23963=DIRECTION('ref_axis',(0.342009281678287,1.50733243649404E-14,0.939696574031162));
#23964=DIRECTION('center_axis',(0.,0.,-1.));
#23965=DIRECTION('ref_axis',(-1.,0.,0.));
#23966=DIRECTION('center_axis',(0.707106781186538,0.707106781186557,-2.18052895483717E-14));
#23967=DIRECTION('ref_axis',(0.668377159293621,-0.668377159293593,0.326410701217372));
#23968=DIRECTION('center_axis',(0.,0.,1.));
#23969=DIRECTION('ref_axis',(0.707106781186608,0.707106781186487,0.));
#23970=DIRECTION('center_axis',(-0.707106781186536,-0.707106781186559,1.97361719728453E-14));
#23971=DIRECTION('ref_axis',(0.241837082303476,-0.241837082303441,0.939696574031161));
#23972=DIRECTION('center_axis',(0.,0.,-1.));
#23973=DIRECTION('ref_axis',(-1.,0.,0.));
#23974=DIRECTION('center_axis',(1.,7.91804511680167E-15,-7.69942093215295E-15));
#23975=DIRECTION('ref_axis',(1.00035767704373E-14,-0.945228043453423,0.326410701217368));
#23976=DIRECTION('center_axis',(0.,0.,1.));
#23977=DIRECTION('ref_axis',(1.,-8.08242361927114E-14,0.));
#23978=DIRECTION('center_axis',(-1.,-1.79398764678015E-15,1.76453926386396E-15));
#23979=DIRECTION('ref_axis',(2.26983333538778E-15,-0.342009281678289,0.939696574031161));
#23980=DIRECTION('center_axis',(0.,0.,-1.));
#23981=DIRECTION('ref_axis',(-1.,0.,0.));
#23982=DIRECTION('center_axis',(0.707106781186538,-0.707106781186557,4.77488092300106E-15));
#23983=DIRECTION('ref_axis',(-0.668377159293619,-0.6683771592936,0.326410701217363));
#23984=DIRECTION('center_axis',(0.,0.,1.));
#23985=DIRECTION('ref_axis',(0.707106781186484,-0.707106781186611,0.));
#23986=DIRECTION('center_axis',(-0.707106781186529,0.707106781186566,-1.90995212640436E-14));
#23987=DIRECTION('ref_axis',(-0.241837082303473,-0.241837082303435,0.939696574031163));
#23988=DIRECTION('center_axis',(0.,0.,-1.));
#23989=DIRECTION('ref_axis',(-1.,0.,0.));
#23990=DIRECTION('center_axis',(-1.02700574112875E-14,-1.,-4.88525407613946E-17));
#23991=DIRECTION('ref_axis',(-0.945228043453422,9.69096499636107E-15,0.326410701217372));
#23992=DIRECTION('center_axis',(0.,0.,1.));
#23993=DIRECTION('ref_axis',(3.13710679174016E-13,-1.,0.));
#23994=DIRECTION('center_axis',(1.0700730164861E-14,1.,-6.44787115032575E-17));
#23995=DIRECTION('ref_axis',(-0.342009281678279,3.72415768800159E-15,0.939696574031164));
#23996=DIRECTION('center_axis',(0.,0.,-1.));
#23997=DIRECTION('ref_axis',(-1.,0.,0.));
#23998=DIRECTION('center_axis',(-0.707106781186564,-0.707106781186531,1.16188769126359E-14));
#23999=DIRECTION('ref_axis',(-0.66837715929359,0.668377159293628,0.326410701217364));
#24000=DIRECTION('center_axis',(0.,0.,1.));
#24001=DIRECTION('ref_axis',(-0.707106781186613,-0.707106781186482,0.));
#24002=DIRECTION('center_axis',(0.707106781186545,0.70710678118655,1.49612916568344E-14));
#24003=DIRECTION('ref_axis',(-0.24183708230347,0.241837082303447,0.939696574031161));
#24004=DIRECTION('center_axis',(0.,0.,-1.));
#24005=DIRECTION('ref_axis',(-1.,0.,0.));
#24006=DIRECTION('center_axis',(-1.,1.15612551933786E-14,1.13714767015716E-14));
#24007=DIRECTION('ref_axis',(1.46383861165231E-14,0.945228043453423,0.326410701217368));
#24008=DIRECTION('center_axis',(0.,0.,1.));
#24009=DIRECTION('ref_axis',(-1.,8.08242361927114E-14,0.));
#24010=DIRECTION('center_axis',(1.,1.65009199484293E-15,1.71165480509254E-15));
#24011=DIRECTION('ref_axis',(-2.1746906207308E-15,0.342009281678289,0.939696574031161));
#24012=DIRECTION('center_axis',(0.,0.,-1.));
#24013=DIRECTION('ref_axis',(-1.,0.,0.));
#24014=DIRECTION('center_axis',(-0.707106781186527,0.707106781186568,2.46702181021724E-14));
#24015=DIRECTION('ref_axis',(0.668377159293632,0.668377159293584,0.326410701217368));
#24016=DIRECTION('center_axis',(0.,0.,1.));
#24017=DIRECTION('ref_axis',(-0.707106781186489,0.707106781186606,0.));
#24018=DIRECTION('center_axis',(0.707106781186532,-0.707106781186563,-1.36879902392314E-14));
#24019=DIRECTION('ref_axis',(0.241837082303472,0.241837082303443,0.939696574031161));
#24020=DIRECTION('center_axis',(0.,0.,-1.));
#24021=DIRECTION('ref_axis',(-1.,0.,0.));
#24022=DIRECTION('center_axis',(2.65449697024962E-14,1.,1.84854068675772E-14));
#24023=DIRECTION('ref_axis',(0.945228043453424,-3.1125259244975E-14,0.326410701217364));
#24024=DIRECTION('center_axis',(0.,0.,1.));
#24025=DIRECTION('ref_axis',(3.28564782949089E-13,1.,0.));
#24026=DIRECTION('center_axis',(0.,0.,-1.));
#24027=DIRECTION('ref_axis',(-1.,0.,0.));
#24028=DIRECTION('',(-0.93969517819209,3.34165038880862E-15,0.342013116828193));
#24029=DIRECTION('center_axis',(0.,0.,-1.));
#24030=DIRECTION('ref_axis',(-1.,0.,0.));
#24031=DIRECTION('',(0.664464832747924,-0.664464832747934,-0.34201311682819));
#24032=DIRECTION('center_axis',(0.,0.,-1.));
#24033=DIRECTION('ref_axis',(-1.,0.,0.));
#24034=DIRECTION('center_axis',(0.,0.,-1.));
#24035=DIRECTION('ref_axis',(-1.,0.,0.));
#24036=DIRECTION('',(0.93969517819209,-3.2601467207889E-15,-0.342013116828193));
#24037=DIRECTION('',(-0.664464832747918,-0.664464832747939,0.342013116828193));
#24038=DIRECTION('center_axis',(0.,0.,-1.));
#24039=DIRECTION('ref_axis',(-1.,0.,0.));
#24040=DIRECTION('',(-0.664464832747928,0.664464832747928,0.342013116828193));
#24041=DIRECTION('center_axis',(0.,0.,-1.));
#24042=DIRECTION('ref_axis',(-1.,0.,0.));
#24043=DIRECTION('',(8.15036680197226E-17,-0.93969517819209,-0.342013116828193));
#24044=DIRECTION('center_axis',(0.,0.,-1.));
#24045=DIRECTION('ref_axis',(-1.,0.,0.));
#24046=DIRECTION('',(8.15036680197226E-17,0.93969517819209,0.342013116828193));
#24047=DIRECTION('center_axis',(0.,0.,-1.));
#24048=DIRECTION('ref_axis',(-1.,0.,0.));
#24049=DIRECTION('',(-0.66446483274794,-0.664464832747919,-0.342013116828188));
#24050=DIRECTION('center_axis',(0.,0.,-1.));
#24051=DIRECTION('ref_axis',(-1.,0.,0.));
#24052=DIRECTION('',(0.664464832747934,0.664464832747924,0.34201311682819));
#24053=DIRECTION('center_axis',(0.,0.,-1.));
#24054=DIRECTION('ref_axis',(-1.,0.,0.));
#24055=DIRECTION('',(-0.93969517819209,9.78044016236671E-15,-0.342013116828193));
#24056=DIRECTION('center_axis',(0.,0.,-1.));
#24057=DIRECTION('ref_axis',(-1.,0.,0.));
#24058=DIRECTION('',(0.939695178192092,-9.94344749840606E-15,0.34201311682819));
#24059=DIRECTION('center_axis',(0.,0.,-1.));
#24060=DIRECTION('ref_axis',(-1.,0.,0.));
#24061=DIRECTION('',(-0.664464832747918,0.664464832747939,-0.342013116828193));
#24062=DIRECTION('center_axis',(0.,0.,-1.));
#24063=DIRECTION('ref_axis',(-1.,0.,0.));
#24064=DIRECTION('',(0.664464832747918,-0.664464832747939,0.342013116828193));
#24065=DIRECTION('center_axis',(0.,0.,-1.));
#24066=DIRECTION('ref_axis',(-1.,0.,0.));
#24067=DIRECTION('',(-8.15036680197226E-17,0.93969517819209,-0.342013116828193));
#24068=DIRECTION('center_axis',(0.,0.,-1.));
#24069=DIRECTION('ref_axis',(-1.,0.,0.));
#24070=DIRECTION('center_axis',(0.,0.,-1.));
#24071=DIRECTION('ref_axis',(-1.,0.,0.));
#24072=DIRECTION('',(0.664464832747934,0.664464832747924,-0.34201311682819));
#24073=DIRECTION('',(-8.15036680197226E-17,-0.93969517819209,0.342013116828193));
#24074=DIRECTION('center_axis',(0.,0.,1.));
#24075=DIRECTION('ref_axis',(1.,0.,0.));
#24076=DIRECTION('',(-0.342027306942117,1.29765967489722E-15,-0.939690013411829));
#24077=DIRECTION('center_axis',(0.,0.,-1.));
#24078=DIRECTION('ref_axis',(-1.,0.,0.));
#24079=DIRECTION('',(0.241849828089742,-0.241849828089742,0.939690013411829));
#24080=DIRECTION('center_axis',(0.,0.,1.));
#24081=DIRECTION('ref_axis',(1.,0.,0.));
#24082=DIRECTION('center_axis',(0.,0.,-1.));
#24083=DIRECTION('ref_axis',(-1.,0.,0.));
#24084=DIRECTION('',(0.342027306942117,-1.08138306241435E-15,0.939690013411829));
#24085=DIRECTION('',(-0.241849828089751,-0.241849828089742,-0.939690013411827));
#24086=DIRECTION('center_axis',(0.,0.,1.));
#24087=DIRECTION('ref_axis',(1.,0.,0.));
#24088=DIRECTION('',(-0.241849828089734,0.241849828089743,-0.939690013411832));
#24089=DIRECTION('center_axis',(0.,0.,-1.));
#24090=DIRECTION('ref_axis',(-1.,0.,0.));
#24091=DIRECTION('',(7.20922041609565E-17,-0.342027306942117,0.939690013411829));
#24092=DIRECTION('center_axis',(0.,0.,1.));
#24093=DIRECTION('ref_axis',(1.,0.,0.));
#24094=DIRECTION('',(7.20922041609565E-17,0.342027306942117,-0.939690013411829));
#24095=DIRECTION('center_axis',(0.,0.,-1.));
#24096=DIRECTION('ref_axis',(-1.,0.,0.));
#24097=DIRECTION('',(-0.241849828089734,-0.241849828089743,0.939690013411832));
#24098=DIRECTION('center_axis',(0.,0.,1.));
#24099=DIRECTION('ref_axis',(1.,0.,0.));
#24100=DIRECTION('',(0.241849828089751,0.241849828089742,-0.939690013411827));
#24101=DIRECTION('center_axis',(0.,0.,-1.));
#24102=DIRECTION('ref_axis',(-1.,0.,0.));
#24103=DIRECTION('',(-0.342027306942125,3.4604257997259E-15,0.939690013411826));
#24104=DIRECTION('center_axis',(0.,0.,1.));
#24105=DIRECTION('ref_axis',(1.,0.,0.));
#24106=DIRECTION('',(0.342027306942117,-3.74879461636974E-15,-0.939690013411829));
#24107=DIRECTION('center_axis',(0.,0.,-1.));
#24108=DIRECTION('ref_axis',(-1.,0.,0.));
#24109=DIRECTION('',(-0.241849828089742,0.241849828089751,0.939690013411827));
#24110=DIRECTION('center_axis',(0.,0.,1.));
#24111=DIRECTION('ref_axis',(1.,0.,0.));
#24112=DIRECTION('',(0.241849828089733,-0.241849828089752,-0.939690013411829));
#24113=DIRECTION('center_axis',(0.,0.,-1.));
#24114=DIRECTION('ref_axis',(-1.,0.,0.));
#24115=DIRECTION('',(-7.20922041609565E-17,0.342027306942117,0.939690013411829));
#24116=DIRECTION('center_axis',(0.,0.,1.));
#24117=DIRECTION('ref_axis',(1.,0.,0.));
#24118=DIRECTION('center_axis',(0.,0.,-1.));
#24119=DIRECTION('ref_axis',(-1.,0.,0.));
#24120=DIRECTION('',(0.241849828089734,0.241849828089743,0.939690013411832));
#24121=DIRECTION('',(-7.20922041609565E-17,-0.342027306942117,-0.939690013411829));
#24122=DIRECTION('center_axis',(0.,0.,-1.));
#24123=DIRECTION('ref_axis',(-1.,0.,0.));
#24124=DIRECTION('',(0.573585346078431,-2.07701987415471E-15,-0.819145805558501));
#24125=DIRECTION('',(-0.405586087801291,0.405586087801293,0.819145805558501));
#24126=DIRECTION('center_axis',(0.,0.,-1.));
#24127=DIRECTION('ref_axis',(-1.,0.,0.));
#24128=DIRECTION('',(-0.573585346078431,1.91898575329511E-15,0.819145805558501));
#24129=DIRECTION('',(0.405586087801295,0.405586087801293,-0.819145805558499));
#24130=DIRECTION('center_axis',(0.,0.,-1.));
#24131=DIRECTION('ref_axis',(-1.,0.,0.));
#24132=DIRECTION('',(0.405586087801291,-0.405586087801293,-0.819145805558501));
#24133=DIRECTION('',(-6.77289089398275E-17,0.573585346078431,0.819145805558501));
#24134=DIRECTION('center_axis',(0.,0.,-1.));
#24135=DIRECTION('ref_axis',(-1.,0.,0.));
#24136=DIRECTION('',(-9.030521191977E-17,-0.573585346078431,-0.819145805558501));
#24137=DIRECTION('',(0.405586087801294,0.405586087801288,0.819145805558502));
#24138=DIRECTION('center_axis',(0.,0.,-1.));
#24139=DIRECTION('ref_axis',(-1.,0.,0.));
#24140=DIRECTION('',(-0.405586087801298,-0.40558608780129,-0.819145805558499));
#24141=DIRECTION('',(0.573585346078431,-5.93756768372488E-15,0.819145805558501));
#24142=DIRECTION('center_axis',(0.,0.,-1.));
#24143=DIRECTION('ref_axis',(-1.,0.,0.));
#24144=DIRECTION('',(-0.573585346078433,6.11817810756441E-15,-0.8191458055585));
#24145=DIRECTION('',(0.405586087801288,-0.405586087801296,0.819145805558501));
#24146=DIRECTION('center_axis',(0.,0.,-1.));
#24147=DIRECTION('ref_axis',(-1.,0.,0.));
#24148=DIRECTION('',(-0.405586087801287,0.405586087801299,-0.8191458055585));
#24149=DIRECTION('',(6.77289089398275E-17,-0.573585346078431,0.819145805558501));
#24150=DIRECTION('center_axis',(0.,0.,-1.));
#24151=DIRECTION('ref_axis',(-1.,0.,0.));
#24152=DIRECTION('',(-0.405586087801294,-0.405586087801288,0.819145805558502));
#24153=DIRECTION('',(9.030521191977E-17,0.573585346078431,-0.819145805558501));
#24154=DIRECTION('center_axis',(0.,0.,1.));
#24155=DIRECTION('ref_axis',(1.,0.,0.));
#24156=DIRECTION('center_axis',(0.,0.,-1.));
#24157=DIRECTION('ref_axis',(-1.,0.,0.));
#24158=DIRECTION('center_axis',(-1.,1.27191845719472E-16,0.));
#24159=DIRECTION('ref_axis',(-1.27191845719472E-16,-1.,0.));
#24160=DIRECTION('',(1.27191845719472E-16,1.,0.));
#24161=DIRECTION('center_axis',(1.,1.27191845719472E-16,0.));
#24162=DIRECTION('ref_axis',(-1.27191845719472E-16,1.,0.));
#24163=DIRECTION('',(1.27191845719472E-16,-1.,0.));
#24164=DIRECTION('center_axis',(0.,0.,-1.));
#24165=DIRECTION('ref_axis',(-1.,0.,0.));
#24166=DIRECTION('center_axis',(-0.707106781186546,0.707106781186549,0.));
#24167=DIRECTION('ref_axis',(-0.707106781186549,-0.707106781186546,0.));
#24168=DIRECTION('',(0.707106781186549,0.707106781186546,0.));
#24169=DIRECTION('center_axis',(0.707106781186546,-0.707106781186549,0.));
#24170=DIRECTION('ref_axis',(0.707106781186549,0.707106781186546,0.));
#24171=DIRECTION('',(-0.707106781186549,-0.707106781186546,0.));
#24172=DIRECTION('center_axis',(0.,0.,-1.));
#24173=DIRECTION('ref_axis',(-0.707106781186546,0.707106781186549,0.));
#24174=DIRECTION('center_axis',(-0.707106781186556,-0.707106781186539,0.));
#24175=DIRECTION('ref_axis',(0.707106781186539,-0.707106781186556,0.));
#24176=DIRECTION('',(-0.707106781186539,0.707106781186556,0.));
#24177=DIRECTION('center_axis',(0.707106781186556,0.707106781186539,0.));
#24178=DIRECTION('ref_axis',(-0.707106781186539,0.707106781186556,0.));
#24179=DIRECTION('',(0.707106781186539,-0.707106781186556,0.));
#24180=DIRECTION('center_axis',(0.,0.,-1.));
#24181=DIRECTION('ref_axis',(-0.707106781186556,-0.707106781186539,0.));
#24182=DIRECTION('center_axis',(-1.06016358622489E-14,-1.,0.));
#24183=DIRECTION('ref_axis',(1.,-1.06016358622489E-14,0.));
#24184=DIRECTION('',(-1.,1.06016358622489E-14,0.));
#24185=DIRECTION('center_axis',(1.03472521708099E-14,1.,0.));
#24186=DIRECTION('ref_axis',(-1.,1.03472521708099E-14,0.));
#24187=DIRECTION('',(1.,-1.03472521708099E-14,0.));
#24188=DIRECTION('center_axis',(0.,0.,-1.));
#24189=DIRECTION('ref_axis',(-1.04744440165294E-14,-1.,0.));
#24190=DIRECTION('center_axis',(0.707106781186541,-0.707106781186554,0.));
#24191=DIRECTION('ref_axis',(0.707106781186554,0.707106781186541,0.));
#24192=DIRECTION('',(-0.707106781186554,-0.707106781186541,0.));
#24193=DIRECTION('center_axis',(-0.707106781186541,0.707106781186554,0.));
#24194=DIRECTION('ref_axis',(-0.707106781186554,-0.707106781186541,0.));
#24195=DIRECTION('',(0.707106781186554,0.707106781186541,0.));
#24196=DIRECTION('center_axis',(0.,0.,-1.));
#24197=DIRECTION('ref_axis',(0.707106781186541,-0.707106781186554,0.));
#24198=DIRECTION('center_axis',(1.,-1.27191845719472E-16,0.));
#24199=DIRECTION('ref_axis',(1.27191845719472E-16,1.,0.));
#24200=DIRECTION('',(-1.27191845719472E-16,-1.,0.));
#24201=DIRECTION('center_axis',(-1.,-1.27191845719472E-16,0.));
#24202=DIRECTION('ref_axis',(1.27191845719472E-16,-1.,0.));
#24203=DIRECTION('',(-1.27191845719472E-16,1.,0.));
#24204=DIRECTION('center_axis',(0.,0.,-1.));
#24205=DIRECTION('ref_axis',(1.,0.,0.));
#24206=DIRECTION('center_axis',(0.707106781186551,0.707106781186544,0.));
#24207=DIRECTION('ref_axis',(-0.707106781186544,0.707106781186551,0.));
#24208=DIRECTION('',(0.707106781186544,-0.707106781186551,0.));
#24209=DIRECTION('center_axis',(-0.707106781186551,-0.707106781186544,0.));
#24210=DIRECTION('ref_axis',(0.707106781186544,-0.707106781186551,0.));
#24211=DIRECTION('',(-0.707106781186544,0.707106781186551,0.));
#24212=DIRECTION('center_axis',(0.,0.,-1.));
#24213=DIRECTION('ref_axis',(0.707106781186551,0.707106781186544,0.));
#24214=DIRECTION('center_axis',(3.61867318456261E-15,1.,0.));
#24215=DIRECTION('ref_axis',(-1.,3.61867318456261E-15,0.));
#24216=DIRECTION('',(1.,-3.61867318456261E-15,0.));
#24217=DIRECTION('center_axis',(-3.36428949312366E-15,-1.,0.));
#24218=DIRECTION('ref_axis',(1.,-3.36428949312366E-15,0.));
#24219=DIRECTION('',(-1.,3.36428949312366E-15,0.));
#24220=DIRECTION('center_axis',(0.,0.,-1.));
#24221=DIRECTION('ref_axis',(3.49148133884313E-15,1.,0.));
#24222=DIRECTION('axis',(0.,0.,1.));
#24223=DIRECTION('refdir',(1.,0.,0.));
#24224=DIRECTION('center_axis',(-1.,0.,0.));
#24225=DIRECTION('ref_axis',(0.,0.,1.));
#24226=DIRECTION('',(0.,0.,1.));
#24227=DIRECTION('',(0.,1.,0.));
#24228=DIRECTION('',(0.,0.,1.));
#24229=DIRECTION('',(0.,1.,0.));
#24230=DIRECTION('center_axis',(0.,0.,1.));
#24231=DIRECTION('ref_axis',(1.,0.,0.));
#24232=DIRECTION('',(1.,0.,0.));
#24233=DIRECTION('',(0.,1.,0.));
#24234=DIRECTION('',(1.,0.,0.));
#24235=DIRECTION('center_axis',(-0.710721462348357,0.,0.703473526834815));
#24236=DIRECTION('ref_axis',(0.703473526834815,0.,0.710721462348357));
#24237=DIRECTION('',(0.703473526834815,0.,0.710721462348357));
#24238=DIRECTION('',(0.,1.,0.));
#24239=DIRECTION('',(0.703473526834815,0.,0.710721462348357));
#24240=DIRECTION('center_axis',(1.,0.,0.));
#24241=DIRECTION('ref_axis',(0.,0.,-1.));
#24242=DIRECTION('',(0.,0.,-1.));
#24243=DIRECTION('',(0.,1.,0.));
#24244=DIRECTION('',(0.,0.,-1.));
#24245=DIRECTION('',(0.,1.,0.));
#24246=DIRECTION('center_axis',(0.,0.,-1.));
#24247=DIRECTION('ref_axis',(-1.,0.,0.));
#24248=DIRECTION('',(-1.,0.,0.));
#24249=DIRECTION('',(-1.,0.,0.));
#24250=DIRECTION('',(0.,1.,0.));
#24251=DIRECTION('center_axis',(1.,0.,0.));
#24252=DIRECTION('ref_axis',(0.,0.,-1.));
#24253=DIRECTION('',(0.,0.,-1.));
#24254=DIRECTION('',(0.,0.,-1.));
#24255=DIRECTION('',(0.,1.,0.));
#24256=DIRECTION('center_axis',(0.,0.,1.));
#24257=DIRECTION('ref_axis',(1.,0.,0.));
#24258=DIRECTION('',(1.,0.,0.));
#24259=DIRECTION('',(1.,0.,0.));
#24260=DIRECTION('',(0.,1.,0.));
#24261=DIRECTION('center_axis',(1.,0.,0.));
#24262=DIRECTION('ref_axis',(0.,0.,-1.));
#24263=DIRECTION('',(0.,0.,-1.));
#24264=DIRECTION('',(0.,0.,-1.));
#24265=DIRECTION('',(0.,1.,0.));
#24266=DIRECTION('center_axis',(0.710721462348357,0.,-0.703473526834815));
#24267=DIRECTION('ref_axis',(-0.703473526834815,0.,-0.710721462348357));
#24268=DIRECTION('',(-0.703473526834815,0.,-0.710721462348357));
#24269=DIRECTION('',(-0.703473526834815,0.,-0.710721462348357));
#24270=DIRECTION('',(0.,1.,0.));
#24271=DIRECTION('center_axis',(-1.,0.,0.));
#24272=DIRECTION('ref_axis',(0.,0.,1.));
#24273=DIRECTION('',(0.,0.,1.));
#24274=DIRECTION('',(0.,1.,0.));
#24275=DIRECTION('',(0.,0.,1.));
#24276=DIRECTION('',(0.,1.,0.));
#24277=DIRECTION('center_axis',(0.,0.,-1.));
#24278=DIRECTION('ref_axis',(-1.,0.,0.));
#24279=DIRECTION('',(-1.,0.,0.));
#24280=DIRECTION('',(-1.,0.,0.));
#24281=DIRECTION('',(0.,1.,0.));
#24282=DIRECTION('center_axis',(-0.710721462348357,0.,-0.703473526834815));
#24283=DIRECTION('ref_axis',(-0.703473526834815,0.,0.710721462348357));
#24284=DIRECTION('',(-0.703473526834815,0.,0.710721462348357));
#24285=DIRECTION('',(-0.703473526834815,0.,0.710721462348357));
#24286=DIRECTION('',(0.,1.,0.));
#24287=DIRECTION('center_axis',(0.,0.,1.));
#24288=DIRECTION('ref_axis',(1.,0.,0.));
#24289=DIRECTION('',(1.,0.,0.));
#24290=DIRECTION('',(-1.,0.,0.));
#24291=DIRECTION('',(0.,1.,0.));
#24292=DIRECTION('center_axis',(1.,0.,0.));
#24293=DIRECTION('ref_axis',(0.,0.,-1.));
#24294=DIRECTION('',(0.,0.,-1.));
#24295=DIRECTION('',(0.,1.,0.));
#24296=DIRECTION('',(0.,0.,-1.));
#24297=DIRECTION('',(0.,1.,0.));
#24298=DIRECTION('center_axis',(0.,0.,1.));
#24299=DIRECTION('ref_axis',(1.,0.,0.));
#24300=DIRECTION('',(1.,0.,0.));
#24301=DIRECTION('',(0.,1.,0.));
#24302=DIRECTION('',(1.,0.,0.));
#24303=DIRECTION('center_axis',(1.,0.,0.));
#24304=DIRECTION('ref_axis',(0.,0.,-1.));
#24305=DIRECTION('',(0.,0.,-1.));
#24306=DIRECTION('',(0.,1.,0.));
#24307=DIRECTION('',(0.,0.,-1.));
#24308=DIRECTION('center_axis',(0.,0.,-1.));
#24309=DIRECTION('ref_axis',(-1.,0.,0.));
#24310=DIRECTION('',(-1.,0.,0.));
#24311=DIRECTION('',(0.,1.,0.));
#24312=DIRECTION('',(-1.,0.,0.));
#24313=DIRECTION('center_axis',(1.,0.,0.));
#24314=DIRECTION('ref_axis',(0.,0.,-1.));
#24315=DIRECTION('',(0.,0.,-1.));
#24316=DIRECTION('',(0.,1.,0.));
#24317=DIRECTION('',(0.,0.,-1.));
#24318=DIRECTION('center_axis',(0.710721462348357,0.,0.703473526834815));
#24319=DIRECTION('ref_axis',(0.703473526834815,0.,-0.710721462348357));
#24320=DIRECTION('',(0.703473526834815,0.,-0.710721462348357));
#24321=DIRECTION('',(0.703473526834815,0.,-0.710721462348357));
#24322=DIRECTION('center_axis',(1.,0.,0.));
#24323=DIRECTION('ref_axis',(0.,0.,-1.));
#24324=DIRECTION('',(0.,0.,-1.));
#24325=DIRECTION('',(0.,1.,0.));
#24326=DIRECTION('',(0.,0.,-1.));
#24327=DIRECTION('',(0.,1.,0.));
#24328=DIRECTION('center_axis',(0.,0.,1.));
#24329=DIRECTION('ref_axis',(1.,0.,0.));
#24330=DIRECTION('',(1.,0.,0.));
#24331=DIRECTION('',(1.,0.,0.));
#24332=DIRECTION('',(0.,1.,0.));
#24333=DIRECTION('center_axis',(0.710721462348357,0.,0.703473526834815));
#24334=DIRECTION('ref_axis',(0.703473526834815,0.,-0.710721462348357));
#24335=DIRECTION('',(0.703473526834815,0.,-0.710721462348357));
#24336=DIRECTION('',(0.703473526834815,0.,-0.710721462348357));
#24337=DIRECTION('',(0.,1.,0.));
#24338=DIRECTION('center_axis',(1.,0.,0.));
#24339=DIRECTION('ref_axis',(0.,0.,-1.));
#24340=DIRECTION('',(0.,0.,1.));
#24341=DIRECTION('',(0.,0.,-1.));
#24342=DIRECTION('center_axis',(-1.,0.,0.));
#24343=DIRECTION('ref_axis',(0.,0.,1.));
#24344=DIRECTION('',(0.,0.,1.));
#24345=DIRECTION('',(0.,1.,0.));
#24346=DIRECTION('',(0.,0.,1.));
#24347=DIRECTION('',(0.,1.,0.));
#24348=DIRECTION('center_axis',(0.,0.,-1.));
#24349=DIRECTION('ref_axis',(-1.,0.,0.));
#24350=DIRECTION('',(-1.,0.,0.));
#24351=DIRECTION('',(0.,1.,0.));
#24352=DIRECTION('',(-1.,0.,0.));
#24353=DIRECTION('center_axis',(-1.,0.,0.));
#24354=DIRECTION('ref_axis',(0.,0.,1.));
#24355=DIRECTION('',(0.,0.,1.));
#24356=DIRECTION('',(0.,1.,0.));
#24357=DIRECTION('',(0.,0.,1.));
#24358=DIRECTION('center_axis',(0.,0.,1.));
#24359=DIRECTION('ref_axis',(1.,0.,0.));
#24360=DIRECTION('',(1.,0.,0.));
#24361=DIRECTION('',(0.,1.,0.));
#24362=DIRECTION('',(1.,0.,0.));
#24363=DIRECTION('center_axis',(-1.,0.,0.));
#24364=DIRECTION('ref_axis',(0.,0.,1.));
#24365=DIRECTION('',(0.,0.,1.));
#24366=DIRECTION('',(0.,1.,0.));
#24367=DIRECTION('',(0.,0.,1.));
#24368=DIRECTION('center_axis',(-0.710721462348357,0.,-0.703473526834815));
#24369=DIRECTION('ref_axis',(-0.703473526834815,0.,0.710721462348357));
#24370=DIRECTION('',(-0.703473526834815,0.,0.710721462348357));
#24371=DIRECTION('',(0.,1.,0.));
#24372=DIRECTION('',(-0.703473526834815,0.,0.710721462348357));
#24373=DIRECTION('center_axis',(1.,0.,0.));
#24374=DIRECTION('ref_axis',(0.,0.,-1.));
#24375=DIRECTION('',(0.,0.,-1.));
#24376=DIRECTION('',(0.,1.,0.));
#24377=DIRECTION('',(0.,0.,-1.));
#24378=DIRECTION('',(0.,1.,0.));
#24379=DIRECTION('center_axis',(0.,0.,-1.));
#24380=DIRECTION('ref_axis',(-1.,0.,0.));
#24381=DIRECTION('',(-1.,0.,0.));
#24382=DIRECTION('',(0.,1.,0.));
#24383=DIRECTION('',(-1.,0.,0.));
#24384=DIRECTION('center_axis',(0.710721462348357,0.,-0.703473526834815));
#24385=DIRECTION('ref_axis',(-0.703473526834815,0.,-0.710721462348357));
#24386=DIRECTION('',(-0.703473526834815,0.,-0.710721462348357));
#24387=DIRECTION('',(0.,1.,0.));
#24388=DIRECTION('',(-0.703473526834815,0.,-0.710721462348357));
#24389=DIRECTION('center_axis',(1.,0.,0.));
#24390=DIRECTION('ref_axis',(0.,0.,-1.));
#24391=DIRECTION('',(0.,0.,1.));
#24392=DIRECTION('',(0.,0.,-1.));
#24393=DIRECTION('center_axis',(0.,1.,0.));
#24394=DIRECTION('ref_axis',(1.,0.,0.));
#24395=DIRECTION('center_axis',(0.,1.,0.));
#24396=DIRECTION('ref_axis',(1.,0.,0.));
#24397=DIRECTION('',(0.,-1.,0.));
#24398=DIRECTION('center_axis',(0.,1.,0.));
#24399=DIRECTION('ref_axis',(-1.,0.,0.));
#24400=DIRECTION('center_axis',(0.,0.,1.));
#24401=DIRECTION('ref_axis',(1.,0.,0.));
#24402=DIRECTION('',(1.,0.,0.));
#24403=DIRECTION('',(0.,1.,0.));
#24404=DIRECTION('',(-1.,0.,0.));
#24405=DIRECTION('center_axis',(-1.,0.,0.));
#24406=DIRECTION('ref_axis',(0.,0.,1.));
#24407=DIRECTION('',(0.,0.,1.));
#24408=DIRECTION('',(0.,1.,0.));
#24409=DIRECTION('',(0.,0.,1.));
#24410=DIRECTION('',(0.,1.,0.));
#24411=DIRECTION('center_axis',(0.,0.,1.));
#24412=DIRECTION('ref_axis',(1.,0.,0.));
#24413=DIRECTION('',(1.,0.,0.));
#24414=DIRECTION('',(1.,0.,0.));
#24415=DIRECTION('',(0.,1.,0.));
#24416=DIRECTION('center_axis',(-1.,0.,0.));
#24417=DIRECTION('ref_axis',(0.,0.,1.));
#24418=DIRECTION('',(0.,0.,1.));
#24419=DIRECTION('',(0.,0.,1.));
#24420=DIRECTION('',(0.,1.,0.));
#24421=DIRECTION('center_axis',(0.,0.,-1.));
#24422=DIRECTION('ref_axis',(-1.,0.,0.));
#24423=DIRECTION('',(-1.,0.,0.));
#24424=DIRECTION('',(-1.,0.,0.));
#24425=DIRECTION('',(0.,1.,0.));
#24426=DIRECTION('center_axis',(-1.,0.,0.));
#24427=DIRECTION('ref_axis',(0.,0.,1.));
#24428=DIRECTION('',(0.,0.,1.));
#24429=DIRECTION('',(0.,0.,1.));
#24430=DIRECTION('',(0.,1.,0.));
#24431=DIRECTION('center_axis',(-0.710721462348357,0.,0.703473526834815));
#24432=DIRECTION('ref_axis',(0.703473526834815,0.,0.710721462348357));
#24433=DIRECTION('',(0.703473526834815,0.,0.710721462348357));
#24434=DIRECTION('',(0.703473526834815,0.,0.710721462348357));
#24435=DIRECTION('center_axis',(1.22464679914735E-16,0.,-1.));
#24436=DIRECTION('ref_axis',(-1.,0.,-1.22464679914735E-16));
#24437=DIRECTION('',(-1.,0.,-1.22464679914735E-16));
#24438=DIRECTION('',(0.,1.,0.));
#24439=DIRECTION('',(-1.,0.,-1.22464679914735E-16));
#24440=DIRECTION('',(0.,1.,0.));
#24441=DIRECTION('center_axis',(0.,-1.,0.));
#24442=DIRECTION('ref_axis',(-1.,0.,-1.22464679914735E-16));
#24443=DIRECTION('center_axis',(0.,1.,0.));
#24444=DIRECTION('ref_axis',(-1.,0.,-1.22464679914735E-16));
#24445=DIRECTION('center_axis',(0.,1.,0.));
#24446=DIRECTION('ref_axis',(-1.,0.,-1.22464679914735E-16));
#24447=DIRECTION('',(0.,1.,0.));
#24448=DIRECTION('center_axis',(-1.,0.,2.6449522119078E-16));
#24449=DIRECTION('ref_axis',(2.6449522119078E-16,0.,1.));
#24450=DIRECTION('',(2.6449522119078E-16,0.,1.));
#24451=DIRECTION('',(2.6449522119078E-16,0.,1.));
#24452=DIRECTION('',(0.,1.,0.));
#24453=DIRECTION('center_axis',(0.,-1.,0.));
#24454=DIRECTION('ref_axis',(-1.22464679914735E-16,0.,1.));
#24455=DIRECTION('center_axis',(0.,1.,0.));
#24456=DIRECTION('ref_axis',(-1.22464679914735E-16,0.,1.));
#24457=DIRECTION('center_axis',(0.,1.,0.));
#24458=DIRECTION('ref_axis',(-1.22464679914735E-16,0.,1.));
#24459=DIRECTION('',(0.,1.,0.));
#24460=DIRECTION('center_axis',(-0.710721462348357,0.,-0.703473526834815));
#24461=DIRECTION('ref_axis',(-0.703473526834815,0.,0.710721462348357));
#24462=DIRECTION('',(-0.703473526834815,0.,0.710721462348357));
#24463=DIRECTION('',(0.,1.,0.));
#24464=DIRECTION('',(-0.703473526834815,0.,0.710721462348357));
#24465=DIRECTION('',(0.,1.,0.));
#24466=DIRECTION('center_axis',(-1.,0.,-1.22464679914735E-16));
#24467=DIRECTION('ref_axis',(-1.22464679914735E-16,0.,1.));
#24468=DIRECTION('',(-1.22464679914735E-16,0.,1.));
#24469=DIRECTION('',(-1.22464679914735E-16,0.,1.));
#24470=DIRECTION('',(0.,1.,0.));
#24471=DIRECTION('center_axis',(-1.22464679914735E-16,0.,1.));
#24472=DIRECTION('ref_axis',(1.,0.,1.22464679914735E-16));
#24473=DIRECTION('',(1.,0.,1.22464679914735E-16));
#24474=DIRECTION('',(1.,0.,1.22464679914735E-16));
#24475=DIRECTION('',(0.,1.,0.));
#24476=DIRECTION('center_axis',(-1.,0.,-1.22464679914735E-16));
#24477=DIRECTION('ref_axis',(-1.22464679914735E-16,0.,1.));
#24478=DIRECTION('',(-1.22464679914735E-16,0.,1.));
#24479=DIRECTION('',(-1.22464679914735E-16,0.,1.));
#24480=DIRECTION('',(0.,1.,0.));
#24481=DIRECTION('center_axis',(1.22464679914735E-16,0.,-1.));
#24482=DIRECTION('ref_axis',(-1.,0.,-1.22464679914735E-16));
#24483=DIRECTION('',(-1.,0.,-1.22464679914735E-16));
#24484=DIRECTION('',(-1.,0.,-1.22464679914735E-16));
#24485=DIRECTION('',(0.,1.,0.));
#24486=DIRECTION('center_axis',(-1.,0.,-1.22464679914735E-16));
#24487=DIRECTION('ref_axis',(-1.22464679914735E-16,0.,1.));
#24488=DIRECTION('',(-1.22464679914735E-16,0.,1.));
#24489=DIRECTION('',(-1.22464679914735E-16,0.,1.));
#24490=DIRECTION('',(0.,1.,0.));
#24491=DIRECTION('center_axis',(1.22464679914735E-16,0.,-1.));
#24492=DIRECTION('ref_axis',(-1.,0.,-1.22464679914735E-16));
#24493=DIRECTION('',(1.,0.,0.));
#24494=DIRECTION('',(-1.,0.,-1.22464679914735E-16));
#24495=DIRECTION('center_axis',(-1.22464679914735E-16,0.,1.));
#24496=DIRECTION('ref_axis',(1.,0.,1.22464679914735E-16));
#24497=DIRECTION('',(1.,0.,1.22464679914735E-16));
#24498=DIRECTION('',(-1.,0.,0.));
#24499=DIRECTION('',(0.,1.,0.));
#24500=DIRECTION('center_axis',(1.,0.,1.22464679914735E-16));
#24501=DIRECTION('ref_axis',(1.22464679914735E-16,0.,-1.));
#24502=DIRECTION('',(1.22464679914735E-16,0.,-1.));
#24503=DIRECTION('',(1.22464679914735E-16,0.,-1.));
#24504=DIRECTION('',(0.,1.,0.));
#24505=DIRECTION('center_axis',(-1.22464679914735E-16,0.,1.));
#24506=DIRECTION('ref_axis',(1.,0.,1.22464679914735E-16));
#24507=DIRECTION('',(1.,0.,1.22464679914735E-16));
#24508=DIRECTION('',(1.,0.,1.22464679914735E-16));
#24509=DIRECTION('',(0.,1.,0.));
#24510=DIRECTION('center_axis',(0.710721462348357,0.,0.703473526834815));
#24511=DIRECTION('ref_axis',(0.703473526834815,0.,-0.710721462348357));
#24512=DIRECTION('',(0.703473526834815,0.,-0.710721462348357));
#24513=DIRECTION('',(0.703473526834815,0.,-0.710721462348357));
#24514=DIRECTION('',(0.,1.,0.));
#24515=DIRECTION('center_axis',(0.,-1.,0.));
#24516=DIRECTION('ref_axis',(1.22464679914735E-16,0.,-1.));
#24517=DIRECTION('center_axis',(0.,1.,0.));
#24518=DIRECTION('ref_axis',(1.22464679914735E-16,0.,-1.));
#24519=DIRECTION('',(0.,1.,0.));
#24520=DIRECTION('center_axis',(0.,1.,0.));
#24521=DIRECTION('ref_axis',(1.22464679914735E-16,0.,-1.));
#24522=DIRECTION('center_axis',(1.,0.,3.15944630467493E-16));
#24523=DIRECTION('ref_axis',(3.15944630467493E-16,0.,-1.));
#24524=DIRECTION('',(3.15944630467493E-16,0.,-1.));
#24525=DIRECTION('',(0.,1.,0.));
#24526=DIRECTION('',(3.15944630467493E-16,0.,-1.));
#24527=DIRECTION('center_axis',(0.,-1.,0.));
#24528=DIRECTION('ref_axis',(1.,0.,1.78860330739173E-14));
#24529=DIRECTION('center_axis',(0.,1.,0.));
#24530=DIRECTION('ref_axis',(1.,0.,1.78860330739173E-14));
#24531=DIRECTION('',(0.,1.,0.));
#24532=DIRECTION('center_axis',(0.,1.,0.));
#24533=DIRECTION('ref_axis',(1.,0.,1.78860330739173E-14));
#24534=DIRECTION('center_axis',(-1.22464679914735E-16,0.,1.));
#24535=DIRECTION('ref_axis',(1.,0.,1.22464679914735E-16));
#24536=DIRECTION('',(1.,0.,1.22464679914735E-16));
#24537=DIRECTION('',(1.,0.,1.22464679914735E-16));
#24538=DIRECTION('center_axis',(1.22464679914735E-16,0.,-1.));
#24539=DIRECTION('ref_axis',(-1.,0.,-1.22464679914735E-16));
#24540=DIRECTION('',(-1.,0.,-1.22464679914735E-16));
#24541=DIRECTION('',(0.,1.,0.));
#24542=DIRECTION('',(-1.,0.,-1.22464679914735E-16));
#24543=DIRECTION('center_axis',(0.710721462348357,0.,-0.703473526834815));
#24544=DIRECTION('ref_axis',(-0.703473526834815,0.,-0.710721462348357));
#24545=DIRECTION('',(-0.703473526834815,0.,-0.710721462348357));
#24546=DIRECTION('',(0.,1.,0.));
#24547=DIRECTION('',(-0.703473526834815,0.,-0.710721462348357));
#24548=DIRECTION('center_axis',(1.,0.,1.22464679914735E-16));
#24549=DIRECTION('ref_axis',(1.22464679914735E-16,0.,-1.));
#24550=DIRECTION('',(1.22464679914735E-16,0.,-1.));
#24551=DIRECTION('',(0.,1.,0.));
#24552=DIRECTION('',(1.22464679914735E-16,0.,-1.));
#24553=DIRECTION('center_axis',(-1.22464679914735E-16,0.,1.));
#24554=DIRECTION('ref_axis',(1.,0.,1.22464679914735E-16));
#24555=DIRECTION('',(1.,0.,1.22464679914735E-16));
#24556=DIRECTION('',(0.,1.,0.));
#24557=DIRECTION('',(1.,0.,1.22464679914735E-16));
#24558=DIRECTION('center_axis',(1.,0.,1.22464679914735E-16));
#24559=DIRECTION('ref_axis',(1.22464679914735E-16,0.,-1.));
#24560=DIRECTION('',(1.22464679914735E-16,0.,-1.));
#24561=DIRECTION('',(0.,1.,0.));
#24562=DIRECTION('',(1.22464679914735E-16,0.,-1.));
#24563=DIRECTION('center_axis',(1.22464679914735E-16,0.,-1.));
#24564=DIRECTION('ref_axis',(-1.,0.,-1.22464679914735E-16));
#24565=DIRECTION('',(-1.,0.,-1.22464679914735E-16));
#24566=DIRECTION('',(0.,1.,0.));
#24567=DIRECTION('',(-1.,0.,-1.22464679914735E-16));
#24568=DIRECTION('center_axis',(1.,0.,1.22464679914735E-16));
#24569=DIRECTION('ref_axis',(1.22464679914735E-16,0.,-1.));
#24570=DIRECTION('',(1.22464679914735E-16,0.,-1.));
#24571=DIRECTION('',(0.,1.,0.));
#24572=DIRECTION('',(1.22464679914735E-16,0.,-1.));
#24573=DIRECTION('center_axis',(1.22464679914735E-16,0.,-1.));
#24574=DIRECTION('ref_axis',(-1.,0.,-1.22464679914735E-16));
#24575=DIRECTION('',(-1.,0.,-1.22464679914735E-16));
#24576=DIRECTION('',(0.,1.,0.));
#24577=DIRECTION('',(-1.,0.,-1.22464679914735E-16));
#24578=DIRECTION('center_axis',(0.,-1.,0.));
#24579=DIRECTION('ref_axis',(1.,0.,1.22464679914735E-16));
#24580=DIRECTION('center_axis',(0.,-1.,0.));
#24581=DIRECTION('ref_axis',(1.,0.,1.22464679914735E-16));
#24582=DIRECTION('',(0.,1.,0.));
#24583=DIRECTION('center_axis',(0.,-1.,0.));
#24584=DIRECTION('ref_axis',(1.,0.,1.22464679914735E-16));
#24585=DIRECTION('center_axis',(-1.,0.,-1.22464679914735E-16));
#24586=DIRECTION('ref_axis',(-1.22464679914735E-16,0.,1.));
#24587=DIRECTION('',(-1.22464679914735E-16,0.,1.));
#24588=DIRECTION('',(0.,1.,0.));
#24589=DIRECTION('',(-1.22464679914735E-16,0.,1.));
#24590=DIRECTION('center_axis',(-1.22464679914735E-16,0.,1.));
#24591=DIRECTION('ref_axis',(1.,0.,1.22464679914735E-16));
#24592=DIRECTION('',(1.,0.,1.22464679914735E-16));
#24593=DIRECTION('',(0.,1.,0.));
#24594=DIRECTION('',(1.,0.,1.22464679914735E-16));
#24595=DIRECTION('center_axis',(-1.,0.,-2.70193671200296E-15));
#24596=DIRECTION('ref_axis',(-2.70193671200296E-15,0.,1.));
#24597=DIRECTION('',(-2.70193671200296E-15,0.,1.));
#24598=DIRECTION('',(0.,1.,0.));
#24599=DIRECTION('',(-2.70193671200296E-15,0.,1.));
#24600=DIRECTION('center_axis',(2.14733784037198E-15,0.,1.));
#24601=DIRECTION('ref_axis',(1.,0.,-2.14733784037198E-15));
#24602=DIRECTION('',(1.,0.,-2.14733784037198E-15));
#24603=DIRECTION('',(0.,1.,0.));
#24604=DIRECTION('',(1.,0.,-2.14733784037198E-15));
#24605=DIRECTION('center_axis',(1.,0.,1.22464679914735E-16));
#24606=DIRECTION('ref_axis',(1.22464679914735E-16,0.,-1.));
#24607=DIRECTION('',(1.22464679914735E-16,0.,-1.));
#24608=DIRECTION('',(0.,1.,0.));
#24609=DIRECTION('',(1.22464679914735E-16,0.,-1.));
#24610=DIRECTION('center_axis',(-1.22464679914735E-16,0.,1.));
#24611=DIRECTION('ref_axis',(1.,0.,1.22464679914735E-16));
#24612=DIRECTION('',(1.,0.,1.22464679914735E-16));
#24613=DIRECTION('',(0.,1.,0.));
#24614=DIRECTION('',(1.,0.,1.22464679914735E-16));
#24615=DIRECTION('center_axis',(-0.710721462348357,0.,0.703473526834815));
#24616=DIRECTION('ref_axis',(0.703473526834815,0.,0.710721462348357));
#24617=DIRECTION('',(0.703473526834815,0.,0.710721462348357));
#24618=DIRECTION('',(0.,1.,0.));
#24619=DIRECTION('',(0.703473526834815,0.,0.710721462348357));
#24620=DIRECTION('center_axis',(1.22464679914735E-16,0.,-1.));
#24621=DIRECTION('ref_axis',(-1.,0.,-1.22464679914735E-16));
#24622=DIRECTION('',(-1.,0.,-1.22464679914735E-16));
#24623=DIRECTION('',(0.,1.,0.));
#24624=DIRECTION('',(-1.,0.,-1.22464679914735E-16));
#24625=DIRECTION('',(0.,1.,0.));
#24626=DIRECTION('center_axis',(0.,1.,0.));
#24627=DIRECTION('ref_axis',(-1.,0.,-1.22464679914735E-16));
#24628=DIRECTION('center_axis',(0.,-1.,0.));
#24629=DIRECTION('ref_axis',(-1.,0.,-1.22464679914735E-16));
#24630=DIRECTION('',(0.,1.,0.));
#24631=DIRECTION('center_axis',(0.,-1.,0.));
#24632=DIRECTION('ref_axis',(-1.,0.,-1.22464679914735E-16));
#24633=DIRECTION('center_axis',(1.,0.,5.0942458102025E-16));
#24634=DIRECTION('ref_axis',(5.0942458102025E-16,0.,-1.));
#24635=DIRECTION('',(5.0942458102025E-16,0.,-1.));
#24636=DIRECTION('',(0.,1.,0.));
#24637=DIRECTION('',(5.0942458102025E-16,0.,-1.));
#24638=DIRECTION('center_axis',(0.,1.,0.));
#24639=DIRECTION('ref_axis',(1.22464679914735E-16,0.,-1.));
#24640=DIRECTION('center_axis',(0.,-1.,0.));
#24641=DIRECTION('ref_axis',(1.22464679914735E-16,0.,-1.));
#24642=DIRECTION('',(0.,1.,0.));
#24643=DIRECTION('center_axis',(0.,-1.,0.));
#24644=DIRECTION('ref_axis',(1.22464679914735E-16,0.,-1.));
#24645=DIRECTION('center_axis',(0.710721462348357,0.,-0.703473526834815));
#24646=DIRECTION('ref_axis',(-0.703473526834815,0.,-0.710721462348357));
#24647=DIRECTION('',(-0.703473526834815,0.,-0.710721462348357));
#24648=DIRECTION('',(0.,1.,0.));
#24649=DIRECTION('',(-0.703473526834815,0.,-0.710721462348357));
#24650=DIRECTION('',(0.,1.,0.));
#24651=DIRECTION('center_axis',(1.,0.,1.22464679914735E-16));
#24652=DIRECTION('ref_axis',(1.22464679914735E-16,0.,-1.));
#24653=DIRECTION('',(1.22464679914735E-16,0.,-1.));
#24654=DIRECTION('',(0.,1.,0.));
#24655=DIRECTION('',(1.22464679914735E-16,0.,-1.));
#24656=DIRECTION('center_axis',(-1.22464679914735E-16,0.,1.));
#24657=DIRECTION('ref_axis',(1.,0.,1.22464679914735E-16));
#24658=DIRECTION('',(1.,0.,1.22464679914735E-16));
#24659=DIRECTION('',(0.,1.,0.));
#24660=DIRECTION('',(1.,0.,1.22464679914735E-16));
#24661=DIRECTION('center_axis',(1.,0.,1.22464679914735E-16));
#24662=DIRECTION('ref_axis',(1.22464679914735E-16,0.,-1.));
#24663=DIRECTION('',(1.22464679914735E-16,0.,-1.));
#24664=DIRECTION('',(0.,1.,0.));
#24665=DIRECTION('',(1.22464679914735E-16,0.,-1.));
#24666=DIRECTION('center_axis',(1.22464679914735E-16,0.,-1.));
#24667=DIRECTION('ref_axis',(-1.,0.,-1.22464679914735E-16));
#24668=DIRECTION('',(-1.,0.,-1.22464679914735E-16));
#24669=DIRECTION('',(0.,1.,0.));
#24670=DIRECTION('',(-1.,0.,-1.22464679914735E-16));
#24671=DIRECTION('center_axis',(1.,0.,1.22464679914735E-16));
#24672=DIRECTION('ref_axis',(1.22464679914735E-16,0.,-1.));
#24673=DIRECTION('',(1.22464679914735E-16,0.,-1.));
#24674=DIRECTION('',(0.,1.,0.));
#24675=DIRECTION('',(1.22464679914735E-16,0.,-1.));
#24676=DIRECTION('center_axis',(1.22464679914735E-16,0.,-1.));
#24677=DIRECTION('ref_axis',(-1.,0.,-1.22464679914735E-16));
#24678=DIRECTION('',(1.,0.,0.));
#24679=DIRECTION('',(-1.,0.,-1.22464679914735E-16));
#24680=DIRECTION('center_axis',(-1.22464679914735E-16,0.,1.));
#24681=DIRECTION('ref_axis',(1.,0.,1.22464679914735E-16));
#24682=DIRECTION('',(1.,0.,1.22464679914735E-16));
#24683=DIRECTION('',(0.,1.,0.));
#24684=DIRECTION('',(-1.,0.,0.));
#24685=DIRECTION('center_axis',(-1.,0.,-1.22464679914735E-16));
#24686=DIRECTION('ref_axis',(-1.22464679914735E-16,0.,1.));
#24687=DIRECTION('',(-1.22464679914735E-16,0.,1.));
#24688=DIRECTION('',(0.,1.,0.));
#24689=DIRECTION('',(-1.22464679914735E-16,0.,1.));
#24690=DIRECTION('center_axis',(-1.22464679914735E-16,0.,1.));
#24691=DIRECTION('ref_axis',(1.,0.,1.22464679914735E-16));
#24692=DIRECTION('',(1.,0.,1.22464679914735E-16));
#24693=DIRECTION('',(0.,1.,0.));
#24694=DIRECTION('',(1.,0.,1.22464679914735E-16));
#24695=DIRECTION('center_axis',(-0.710721462348357,0.,0.703473526834815));
#24696=DIRECTION('ref_axis',(0.703473526834815,0.,0.710721462348357));
#24697=DIRECTION('',(0.703473526834815,0.,0.710721462348357));
#24698=DIRECTION('',(0.,1.,0.));
#24699=DIRECTION('',(0.703473526834815,0.,0.710721462348357));
#24700=DIRECTION('center_axis',(-1.,0.,-1.22464679914735E-16));
#24701=DIRECTION('ref_axis',(-1.22464679914735E-16,0.,1.));
#24702=DIRECTION('',(1.22464679914735E-16,0.,-1.));
#24703=DIRECTION('',(-1.22464679914735E-16,0.,1.));
#24704=DIRECTION('center_axis',(0.,1.,0.));
#24705=DIRECTION('ref_axis',(-1.,0.,-1.22464679914735E-16));
#24706=DIRECTION('center_axis',(0.,-1.,0.));
#24707=DIRECTION('ref_axis',(-1.,0.,-1.22464679914735E-16));
#24708=DIRECTION('',(0.,-1.,0.));
#24709=DIRECTION('center_axis',(0.,1.,0.));
#24710=DIRECTION('ref_axis',(-1.,0.,-1.22464679914735E-16));
#24711=DIRECTION('center_axis',(1.,0.,1.22464679914735E-16));
#24712=DIRECTION('ref_axis',(1.22464679914735E-16,0.,-1.));
#24713=DIRECTION('',(1.22464679914735E-16,0.,-1.));
#24714=DIRECTION('',(0.,1.,0.));
#24715=DIRECTION('',(-1.22464679914735E-16,0.,1.));
#24716=DIRECTION('center_axis',(0.,1.,0.));
#24717=DIRECTION('ref_axis',(-1.22464679914735E-16,0.,1.));
#24718=DIRECTION('center_axis',(0.,-1.,0.));
#24719=DIRECTION('ref_axis',(-1.22464679914735E-16,0.,1.));
#24720=DIRECTION('center_axis',(0.,-1.,0.));
#24721=DIRECTION('ref_axis',(-1.22464679914735E-16,0.,1.));
#24722=DIRECTION('',(0.,1.,0.));
#24723=DIRECTION('center_axis',(-1.,0.,7.10152706380222E-17));
#24724=DIRECTION('ref_axis',(7.10152706380222E-17,0.,1.));
#24725=DIRECTION('',(7.10152706380222E-17,0.,1.));
#24726=DIRECTION('',(7.10152706380222E-17,0.,1.));
#24727=DIRECTION('',(0.,1.,0.));
#24728=DIRECTION('center_axis',(0.,1.,0.));
#24729=DIRECTION('ref_axis',(1.,0.,-1.76411037140878E-14));
#24730=DIRECTION('center_axis',(0.,-1.,0.));
#24731=DIRECTION('ref_axis',(1.,0.,-1.76411037140878E-14));
#24732=DIRECTION('center_axis',(0.,-1.,0.));
#24733=DIRECTION('ref_axis',(1.,0.,-1.76411037140878E-14));
#24734=DIRECTION('',(0.,1.,0.));
#24735=DIRECTION('center_axis',(-1.22464679914735E-16,0.,1.));
#24736=DIRECTION('ref_axis',(1.,0.,1.22464679914735E-16));
#24737=DIRECTION('',(1.,0.,1.22464679914735E-16));
#24738=DIRECTION('',(1.,0.,1.22464679914735E-16));
#24739=DIRECTION('center_axis',(1.22464679914735E-16,0.,-1.));
#24740=DIRECTION('ref_axis',(-1.,0.,-1.22464679914735E-16));
#24741=DIRECTION('',(-1.,0.,-1.22464679914735E-16));
#24742=DIRECTION('',(-1.,0.,-1.22464679914735E-16));
#24743=DIRECTION('',(0.,1.,0.));
#24744=DIRECTION('center_axis',(-0.710721462348357,0.,-0.703473526834815));
#24745=DIRECTION('ref_axis',(-0.703473526834815,0.,0.710721462348357));
#24746=DIRECTION('',(-0.703473526834815,0.,0.710721462348357));
#24747=DIRECTION('',(-0.703473526834815,0.,0.710721462348357));
#24748=DIRECTION('',(0.,1.,0.));
#24749=DIRECTION('center_axis',(-1.,0.,-1.22464679914735E-16));
#24750=DIRECTION('ref_axis',(-1.22464679914735E-16,0.,1.));
#24751=DIRECTION('',(-1.22464679914735E-16,0.,1.));
#24752=DIRECTION('',(-1.22464679914735E-16,0.,1.));
#24753=DIRECTION('',(0.,1.,0.));
#24754=DIRECTION('center_axis',(-1.22464679914735E-16,0.,1.));
#24755=DIRECTION('ref_axis',(1.,0.,1.22464679914735E-16));
#24756=DIRECTION('',(1.,0.,1.22464679914735E-16));
#24757=DIRECTION('',(1.,0.,1.22464679914735E-16));
#24758=DIRECTION('',(0.,1.,0.));
#24759=DIRECTION('center_axis',(-1.,0.,-1.22464679914735E-16));
#24760=DIRECTION('ref_axis',(-1.22464679914735E-16,0.,1.));
#24761=DIRECTION('',(-1.22464679914735E-16,0.,1.));
#24762=DIRECTION('',(-1.22464679914735E-16,0.,1.));
#24763=DIRECTION('',(0.,1.,0.));
#24764=DIRECTION('center_axis',(1.22464679914735E-16,0.,-1.));
#24765=DIRECTION('ref_axis',(-1.,0.,-1.22464679914735E-16));
#24766=DIRECTION('',(-1.,0.,-1.22464679914735E-16));
#24767=DIRECTION('',(-1.,0.,-1.22464679914735E-16));
#24768=DIRECTION('',(0.,1.,0.));
#24769=DIRECTION('center_axis',(-1.,0.,-1.22464679914735E-16));
#24770=DIRECTION('ref_axis',(-1.22464679914735E-16,0.,1.));
#24771=DIRECTION('',(-1.22464679914735E-16,0.,1.));
#24772=DIRECTION('',(-1.22464679914735E-16,0.,1.));
#24773=DIRECTION('',(0.,1.,0.));
#24774=DIRECTION('center_axis',(1.22464679914735E-16,0.,-1.));
#24775=DIRECTION('ref_axis',(-1.,0.,-1.22464679914735E-16));
#24776=DIRECTION('',(-1.,0.,-1.22464679914735E-16));
#24777=DIRECTION('',(-1.,0.,-1.22464679914735E-16));
#24778=DIRECTION('',(0.,1.,0.));
#24779=DIRECTION('center_axis',(0.,1.,0.));
#24780=DIRECTION('ref_axis',(1.,0.,1.22464679914735E-16));
#24781=DIRECTION('center_axis',(0.,1.,0.));
#24782=DIRECTION('ref_axis',(1.,0.,1.22464679914735E-16));
#24783=DIRECTION('center_axis',(0.,1.,0.));
#24784=DIRECTION('ref_axis',(1.,0.,1.22464679914735E-16));
#24785=DIRECTION('',(0.,1.,0.));
#24786=DIRECTION('center_axis',(1.,0.,1.22464679914735E-16));
#24787=DIRECTION('ref_axis',(1.22464679914735E-16,0.,-1.));
#24788=DIRECTION('',(1.22464679914735E-16,0.,-1.));
#24789=DIRECTION('',(1.22464679914735E-16,0.,-1.));
#24790=DIRECTION('',(0.,1.,0.));
#24791=DIRECTION('center_axis',(-1.22464679914735E-16,0.,1.));
#24792=DIRECTION('ref_axis',(1.,0.,1.22464679914735E-16));
#24793=DIRECTION('',(1.,0.,1.22464679914735E-16));
#24794=DIRECTION('',(1.,0.,1.22464679914735E-16));
#24795=DIRECTION('',(0.,1.,0.));
#24796=DIRECTION('center_axis',(1.,0.,-2.45700735217349E-15));
#24797=DIRECTION('ref_axis',(-2.45700735217349E-15,0.,-1.));
#24798=DIRECTION('',(-2.45700735217349E-15,0.,-1.));
#24799=DIRECTION('',(-2.45700735217349E-15,0.,-1.));
#24800=DIRECTION('',(0.,1.,0.));
#24801=DIRECTION('center_axis',(-2.39226720020145E-15,0.,1.));
#24802=DIRECTION('ref_axis',(1.,0.,2.39226720020145E-15));
#24803=DIRECTION('',(1.,0.,2.39226720020145E-15));
#24804=DIRECTION('',(1.,0.,2.39226720020145E-15));
#24805=DIRECTION('',(0.,1.,0.));
#24806=DIRECTION('center_axis',(-1.,0.,-1.22464679914735E-16));
#24807=DIRECTION('ref_axis',(-1.22464679914735E-16,0.,1.));
#24808=DIRECTION('',(-1.22464679914735E-16,0.,1.));
#24809=DIRECTION('',(-1.22464679914735E-16,0.,1.));
#24810=DIRECTION('',(0.,1.,0.));
#24811=DIRECTION('center_axis',(-1.22464679914735E-16,0.,1.));
#24812=DIRECTION('ref_axis',(1.,0.,1.22464679914735E-16));
#24813=DIRECTION('',(1.,0.,1.22464679914735E-16));
#24814=DIRECTION('',(1.,0.,1.22464679914735E-16));
#24815=DIRECTION('',(0.,1.,0.));
#24816=DIRECTION('center_axis',(0.710721462348356,0.,0.703473526834815));
#24817=DIRECTION('ref_axis',(0.703473526834815,0.,-0.710721462348356));
#24818=DIRECTION('',(0.703473526834815,0.,-0.710721462348356));
#24819=DIRECTION('',(0.703473526834815,0.,-0.710721462348356));
#24820=DIRECTION('center_axis',(-1.,0.,0.));
#24821=DIRECTION('ref_axis',(0.,0.,1.));
#24822=DIRECTION('',(0.,0.,1.));
#24823=DIRECTION('',(0.,1.,0.));
#24824=DIRECTION('',(0.,0.,1.));
#24825=DIRECTION('',(0.,1.,0.));
#24826=DIRECTION('center_axis',(0.,0.,1.));
#24827=DIRECTION('ref_axis',(1.,0.,0.));
#24828=DIRECTION('',(1.,0.,0.));
#24829=DIRECTION('',(0.,1.,0.));
#24830=DIRECTION('',(1.,0.,0.));
#24831=DIRECTION('center_axis',(-0.710721462348357,0.,0.703473526834815));
#24832=DIRECTION('ref_axis',(0.703473526834815,0.,0.710721462348357));
#24833=DIRECTION('',(0.703473526834815,0.,0.710721462348357));
#24834=DIRECTION('',(0.,1.,0.));
#24835=DIRECTION('',(0.703473526834815,0.,0.710721462348357));
#24836=DIRECTION('center_axis',(1.,0.,0.));
#24837=DIRECTION('ref_axis',(0.,0.,-1.));
#24838=DIRECTION('',(0.,0.,-1.));
#24839=DIRECTION('',(0.,1.,0.));
#24840=DIRECTION('',(0.,0.,-1.));
#24841=DIRECTION('',(0.,1.,0.));
#24842=DIRECTION('center_axis',(0.,0.,-1.));
#24843=DIRECTION('ref_axis',(-1.,0.,0.));
#24844=DIRECTION('',(-1.,0.,0.));
#24845=DIRECTION('',(-1.,0.,0.));
#24846=DIRECTION('',(0.,1.,0.));
#24847=DIRECTION('center_axis',(1.,0.,0.));
#24848=DIRECTION('ref_axis',(0.,0.,-1.));
#24849=DIRECTION('',(0.,0.,-1.));
#24850=DIRECTION('',(0.,0.,-1.));
#24851=DIRECTION('',(0.,1.,0.));
#24852=DIRECTION('center_axis',(0.,0.,1.));
#24853=DIRECTION('ref_axis',(1.,0.,0.));
#24854=DIRECTION('',(1.,0.,0.));
#24855=DIRECTION('',(1.,0.,0.));
#24856=DIRECTION('',(0.,1.,0.));
#24857=DIRECTION('center_axis',(1.,0.,0.));
#24858=DIRECTION('ref_axis',(0.,0.,-1.));
#24859=DIRECTION('',(0.,0.,-1.));
#24860=DIRECTION('',(0.,0.,-1.));
#24861=DIRECTION('',(0.,1.,0.));
#24862=DIRECTION('center_axis',(0.710721462348357,0.,-0.703473526834815));
#24863=DIRECTION('ref_axis',(-0.703473526834815,0.,-0.710721462348357));
#24864=DIRECTION('',(-0.703473526834815,0.,-0.710721462348357));
#24865=DIRECTION('',(-0.703473526834815,0.,-0.710721462348357));
#24866=DIRECTION('',(0.,1.,0.));
#24867=DIRECTION('center_axis',(0.,0.,-1.));
#24868=DIRECTION('ref_axis',(-1.,0.,0.));
#24869=DIRECTION('',(-1.,0.,0.));
#24870=DIRECTION('',(-1.,0.,0.));
#24871=DIRECTION('',(0.,1.,0.));
#24872=DIRECTION('center_axis',(-1.,0.,0.));
#24873=DIRECTION('ref_axis',(0.,0.,1.));
#24874=DIRECTION('',(0.,0.,1.));
#24875=DIRECTION('',(0.,0.,1.));
#24876=DIRECTION('',(0.,1.,0.));
#24877=DIRECTION('center_axis',(0.,0.,-1.));
#24878=DIRECTION('ref_axis',(-1.,0.,0.));
#24879=DIRECTION('',(-1.,0.,0.));
#24880=DIRECTION('',(-1.,0.,0.));
#24881=DIRECTION('',(0.,1.,0.));
#24882=DIRECTION('center_axis',(-0.710721462348357,0.,-0.703473526834815));
#24883=DIRECTION('ref_axis',(-0.703473526834815,0.,0.710721462348357));
#24884=DIRECTION('',(-0.703473526834815,0.,0.710721462348357));
#24885=DIRECTION('',(-0.703473526834815,0.,0.710721462348357));
#24886=DIRECTION('',(0.,1.,0.));
#24887=DIRECTION('center_axis',(0.,0.,1.));
#24888=DIRECTION('ref_axis',(1.,0.,0.));
#24889=DIRECTION('',(1.,0.,0.));
#24890=DIRECTION('',(-1.,0.,0.));
#24891=DIRECTION('',(0.,1.,0.));
#24892=DIRECTION('center_axis',(0.,0.,1.));
#24893=DIRECTION('ref_axis',(1.,0.,0.));
#24894=DIRECTION('',(-1.,0.,0.));
#24895=DIRECTION('',(0.,1.,0.));
#24896=DIRECTION('',(1.,0.,0.));
#24897=DIRECTION('center_axis',(1.,0.,0.));
#24898=DIRECTION('ref_axis',(0.,0.,-1.));
#24899=DIRECTION('',(0.,0.,-1.));
#24900=DIRECTION('',(0.,1.,0.));
#24901=DIRECTION('',(0.,0.,-1.));
#24902=DIRECTION('center_axis',(0.,0.,1.));
#24903=DIRECTION('ref_axis',(1.,0.,0.));
#24904=DIRECTION('',(1.,0.,0.));
#24905=DIRECTION('',(0.,1.,0.));
#24906=DIRECTION('',(1.,0.,0.));
#24907=DIRECTION('center_axis',(1.,0.,0.));
#24908=DIRECTION('ref_axis',(0.,0.,-1.));
#24909=DIRECTION('',(0.,0.,-1.));
#24910=DIRECTION('',(0.,1.,0.));
#24911=DIRECTION('',(0.,0.,-1.));
#24912=DIRECTION('center_axis',(0.,0.,-1.));
#24913=DIRECTION('ref_axis',(-1.,0.,0.));
#24914=DIRECTION('',(-1.,0.,0.));
#24915=DIRECTION('',(0.,1.,0.));
#24916=DIRECTION('',(-1.,0.,0.));
#24917=DIRECTION('center_axis',(1.,0.,0.));
#24918=DIRECTION('ref_axis',(0.,0.,-1.));
#24919=DIRECTION('',(0.,0.,-1.));
#24920=DIRECTION('',(0.,1.,0.));
#24921=DIRECTION('',(0.,0.,-1.));
#24922=DIRECTION('center_axis',(0.710721462348357,0.,0.703473526834815));
#24923=DIRECTION('ref_axis',(0.703473526834815,0.,-0.710721462348357));
#24924=DIRECTION('',(0.703473526834815,0.,-0.710721462348357));
#24925=DIRECTION('',(0.703473526834815,0.,-0.710721462348357));
#24926=DIRECTION('center_axis',(1.,0.,0.));
#24927=DIRECTION('ref_axis',(0.,0.,-1.));
#24928=DIRECTION('',(0.,0.,-1.));
#24929=DIRECTION('',(0.,1.,0.));
#24930=DIRECTION('',(0.,0.,-1.));
#24931=DIRECTION('',(0.,1.,0.));
#24932=DIRECTION('center_axis',(0.,0.,1.));
#24933=DIRECTION('ref_axis',(1.,0.,0.));
#24934=DIRECTION('',(1.,0.,0.));
#24935=DIRECTION('',(1.,0.,0.));
#24936=DIRECTION('',(0.,1.,0.));
#24937=DIRECTION('center_axis',(0.710721462348357,0.,0.703473526834815));
#24938=DIRECTION('ref_axis',(0.703473526834815,0.,-0.710721462348357));
#24939=DIRECTION('',(0.703473526834815,0.,-0.710721462348357));
#24940=DIRECTION('',(0.703473526834815,0.,-0.710721462348357));
#24941=DIRECTION('',(0.,1.,0.));
#24942=DIRECTION('center_axis',(1.,0.,0.));
#24943=DIRECTION('ref_axis',(0.,0.,-1.));
#24944=DIRECTION('',(0.,0.,1.));
#24945=DIRECTION('',(0.,0.,-1.));
#24946=DIRECTION('center_axis',(-1.,0.,0.));
#24947=DIRECTION('ref_axis',(0.,0.,1.));
#24948=DIRECTION('',(0.,0.,1.));
#24949=DIRECTION('',(0.,1.,0.));
#24950=DIRECTION('',(0.,0.,1.));
#24951=DIRECTION('',(0.,1.,0.));
#24952=DIRECTION('center_axis',(0.,0.,-1.));
#24953=DIRECTION('ref_axis',(-1.,0.,0.));
#24954=DIRECTION('',(-1.,0.,0.));
#24955=DIRECTION('',(0.,1.,0.));
#24956=DIRECTION('',(-1.,0.,0.));
#24957=DIRECTION('center_axis',(-1.,0.,0.));
#24958=DIRECTION('ref_axis',(0.,0.,1.));
#24959=DIRECTION('',(0.,0.,1.));
#24960=DIRECTION('',(0.,1.,0.));
#24961=DIRECTION('',(0.,0.,1.));
#24962=DIRECTION('center_axis',(0.,0.,1.));
#24963=DIRECTION('ref_axis',(1.,0.,0.));
#24964=DIRECTION('',(1.,0.,0.));
#24965=DIRECTION('',(0.,1.,0.));
#24966=DIRECTION('',(1.,0.,0.));
#24967=DIRECTION('center_axis',(-1.,0.,0.));
#24968=DIRECTION('ref_axis',(0.,0.,1.));
#24969=DIRECTION('',(0.,0.,1.));
#24970=DIRECTION('',(0.,1.,0.));
#24971=DIRECTION('',(0.,0.,1.));
#24972=DIRECTION('center_axis',(-0.710721462348357,0.,-0.703473526834815));
#24973=DIRECTION('ref_axis',(-0.703473526834815,0.,0.710721462348357));
#24974=DIRECTION('',(-0.703473526834815,0.,0.710721462348357));
#24975=DIRECTION('',(0.,1.,0.));
#24976=DIRECTION('',(-0.703473526834815,0.,0.710721462348357));
#24977=DIRECTION('center_axis',(0.,0.,-1.));
#24978=DIRECTION('ref_axis',(-1.,0.,0.));
#24979=DIRECTION('',(-1.,0.,0.));
#24980=DIRECTION('',(0.,1.,0.));
#24981=DIRECTION('',(1.,0.,0.));
#24982=DIRECTION('center_axis',(1.,0.,0.));
#24983=DIRECTION('ref_axis',(0.,0.,-1.));
#24984=DIRECTION('',(0.,0.,-1.));
#24985=DIRECTION('',(0.,1.,0.));
#24986=DIRECTION('',(0.,0.,-1.));
#24987=DIRECTION('center_axis',(0.,0.,-1.));
#24988=DIRECTION('ref_axis',(-1.,0.,0.));
#24989=DIRECTION('',(-1.,0.,0.));
#24990=DIRECTION('',(0.,1.,0.));
#24991=DIRECTION('',(-1.,0.,0.));
#24992=DIRECTION('center_axis',(0.710721462348357,0.,-0.703473526834815));
#24993=DIRECTION('ref_axis',(-0.703473526834815,0.,-0.710721462348357));
#24994=DIRECTION('',(-0.703473526834815,0.,-0.710721462348357));
#24995=DIRECTION('',(0.,1.,0.));
#24996=DIRECTION('',(-0.703473526834815,0.,-0.710721462348357));
#24997=DIRECTION('center_axis',(1.,0.,0.));
#24998=DIRECTION('ref_axis',(0.,0.,-1.));
#24999=DIRECTION('',(0.,0.,1.));
#25000=DIRECTION('',(0.,0.,-1.));
#25001=DIRECTION('center_axis',(0.,1.,0.));
#25002=DIRECTION('ref_axis',(1.,0.,0.));
#25003=DIRECTION('center_axis',(0.,1.,0.));
#25004=DIRECTION('ref_axis',(1.,0.,0.));
#25005=DIRECTION('',(0.,-1.,0.));
#25006=DIRECTION('center_axis',(0.,1.,0.));
#25007=DIRECTION('ref_axis',(-1.,0.,0.));
#25008=DIRECTION('center_axis',(0.,0.,1.));
#25009=DIRECTION('ref_axis',(1.,0.,0.));
#25010=DIRECTION('',(1.,0.,0.));
#25011=DIRECTION('',(0.,1.,0.));
#25012=DIRECTION('',(-1.,0.,0.));
#25013=DIRECTION('center_axis',(0.,0.,1.));
#25014=DIRECTION('ref_axis',(1.,0.,0.));
#25015=DIRECTION('',(-1.,0.,0.));
#25016=DIRECTION('',(1.,0.,0.));
#25017=DIRECTION('',(0.,1.,0.));
#25018=DIRECTION('center_axis',(-1.,0.,0.));
#25019=DIRECTION('ref_axis',(0.,0.,1.));
#25020=DIRECTION('',(0.,0.,1.));
#25021=DIRECTION('',(0.,0.,1.));
#25022=DIRECTION('',(0.,1.,0.));
#25023=DIRECTION('center_axis',(0.,0.,1.));
#25024=DIRECTION('ref_axis',(1.,0.,0.));
#25025=DIRECTION('',(1.,0.,0.));
#25026=DIRECTION('',(1.,0.,0.));
#25027=DIRECTION('',(0.,1.,0.));
#25028=DIRECTION('center_axis',(-1.,0.,0.));
#25029=DIRECTION('ref_axis',(0.,0.,1.));
#25030=DIRECTION('',(0.,0.,1.));
#25031=DIRECTION('',(0.,0.,1.));
#25032=DIRECTION('',(0.,1.,0.));
#25033=DIRECTION('center_axis',(0.,0.,-1.));
#25034=DIRECTION('ref_axis',(-1.,0.,0.));
#25035=DIRECTION('',(-1.,0.,0.));
#25036=DIRECTION('',(-1.,0.,0.));
#25037=DIRECTION('',(0.,1.,0.));
#25038=DIRECTION('center_axis',(-1.,0.,0.));
#25039=DIRECTION('ref_axis',(0.,0.,1.));
#25040=DIRECTION('',(0.,0.,1.));
#25041=DIRECTION('',(0.,0.,1.));
#25042=DIRECTION('',(0.,1.,0.));
#25043=DIRECTION('center_axis',(-0.710721462348357,0.,0.703473526834815));
#25044=DIRECTION('ref_axis',(0.703473526834815,0.,0.710721462348357));
#25045=DIRECTION('',(0.703473526834815,0.,0.710721462348357));
#25046=DIRECTION('',(0.703473526834815,0.,0.710721462348357));
#25047=DIRECTION('center_axis',(-1.,0.,0.));
#25048=DIRECTION('ref_axis',(0.,0.,1.));
#25049=DIRECTION('',(0.,0.,1.));
#25050=DIRECTION('',(0.,1.,0.));
#25051=DIRECTION('',(0.,0.,1.));
#25052=DIRECTION('',(0.,1.,0.));
#25053=DIRECTION('center_axis',(0.,0.,1.));
#25054=DIRECTION('ref_axis',(1.,0.,0.));
#25055=DIRECTION('',(1.,0.,0.));
#25056=DIRECTION('',(0.,1.,0.));
#25057=DIRECTION('',(1.,0.,0.));
#25058=DIRECTION('center_axis',(-0.710721462348357,0.,0.703473526834815));
#25059=DIRECTION('ref_axis',(0.703473526834815,0.,0.710721462348357));
#25060=DIRECTION('',(0.703473526834815,0.,0.710721462348357));
#25061=DIRECTION('',(0.,1.,0.));
#25062=DIRECTION('',(0.703473526834815,0.,0.710721462348357));
#25063=DIRECTION('center_axis',(1.,0.,0.));
#25064=DIRECTION('ref_axis',(0.,0.,-1.));
#25065=DIRECTION('',(0.,0.,-1.));
#25066=DIRECTION('',(0.,1.,0.));
#25067=DIRECTION('',(0.,0.,-1.));
#25068=DIRECTION('',(0.,1.,0.));
#25069=DIRECTION('center_axis',(0.,0.,-1.));
#25070=DIRECTION('ref_axis',(-1.,0.,0.));
#25071=DIRECTION('',(-1.,0.,0.));
#25072=DIRECTION('',(-1.,0.,0.));
#25073=DIRECTION('',(0.,1.,0.));
#25074=DIRECTION('center_axis',(1.,0.,0.));
#25075=DIRECTION('ref_axis',(0.,0.,-1.));
#25076=DIRECTION('',(0.,0.,-1.));
#25077=DIRECTION('',(0.,0.,-1.));
#25078=DIRECTION('',(0.,1.,0.));
#25079=DIRECTION('center_axis',(0.,0.,1.));
#25080=DIRECTION('ref_axis',(1.,0.,0.));
#25081=DIRECTION('',(1.,0.,0.));
#25082=DIRECTION('',(1.,0.,0.));
#25083=DIRECTION('',(0.,1.,0.));
#25084=DIRECTION('center_axis',(1.,0.,0.));
#25085=DIRECTION('ref_axis',(0.,0.,-1.));
#25086=DIRECTION('',(0.,0.,-1.));
#25087=DIRECTION('',(0.,0.,-1.));
#25088=DIRECTION('',(0.,1.,0.));
#25089=DIRECTION('center_axis',(0.710721462348357,0.,-0.703473526834815));
#25090=DIRECTION('ref_axis',(-0.703473526834815,0.,-0.710721462348357));
#25091=DIRECTION('',(-0.703473526834815,0.,-0.710721462348357));
#25092=DIRECTION('',(-0.703473526834815,0.,-0.710721462348357));
#25093=DIRECTION('',(0.,1.,0.));
#25094=DIRECTION('center_axis',(0.,0.,-1.));
#25095=DIRECTION('ref_axis',(-1.,0.,0.));
#25096=DIRECTION('',(-1.,0.,0.));
#25097=DIRECTION('',(-1.,0.,0.));
#25098=DIRECTION('',(0.,1.,0.));
#25099=DIRECTION('center_axis',(-1.,0.,0.));
#25100=DIRECTION('ref_axis',(0.,0.,1.));
#25101=DIRECTION('',(0.,0.,1.));
#25102=DIRECTION('',(0.,0.,1.));
#25103=DIRECTION('',(0.,1.,0.));
#25104=DIRECTION('center_axis',(0.,0.,-1.));
#25105=DIRECTION('ref_axis',(-1.,0.,0.));
#25106=DIRECTION('',(-1.,0.,0.));
#25107=DIRECTION('',(-1.,0.,0.));
#25108=DIRECTION('',(0.,1.,0.));
#25109=DIRECTION('center_axis',(-0.710721462348357,0.,-0.703473526834815));
#25110=DIRECTION('ref_axis',(-0.703473526834815,0.,0.710721462348357));
#25111=DIRECTION('',(-0.703473526834815,0.,0.710721462348357));
#25112=DIRECTION('',(-0.703473526834815,0.,0.710721462348357));
#25113=DIRECTION('',(0.,1.,0.));
#25114=DIRECTION('center_axis',(0.,0.,1.));
#25115=DIRECTION('ref_axis',(1.,0.,0.));
#25116=DIRECTION('',(1.,0.,0.));
#25117=DIRECTION('',(-1.,0.,0.));
#25118=DIRECTION('',(0.,1.,0.));
#25119=DIRECTION('center_axis',(0.,0.,1.));
#25120=DIRECTION('ref_axis',(1.,0.,0.));
#25121=DIRECTION('',(-1.,0.,0.));
#25122=DIRECTION('',(0.,1.,0.));
#25123=DIRECTION('',(1.,0.,0.));
#25124=DIRECTION('center_axis',(1.,0.,0.));
#25125=DIRECTION('ref_axis',(0.,0.,-1.));
#25126=DIRECTION('',(0.,0.,-1.));
#25127=DIRECTION('',(0.,1.,0.));
#25128=DIRECTION('',(0.,0.,-1.));
#25129=DIRECTION('center_axis',(0.,0.,1.));
#25130=DIRECTION('ref_axis',(1.,0.,0.));
#25131=DIRECTION('',(1.,0.,0.));
#25132=DIRECTION('',(0.,1.,0.));
#25133=DIRECTION('',(1.,0.,0.));
#25134=DIRECTION('center_axis',(1.,0.,0.));
#25135=DIRECTION('ref_axis',(0.,0.,-1.));
#25136=DIRECTION('',(0.,0.,-1.));
#25137=DIRECTION('',(0.,1.,0.));
#25138=DIRECTION('',(0.,0.,-1.));
#25139=DIRECTION('center_axis',(0.,0.,-1.));
#25140=DIRECTION('ref_axis',(-1.,0.,0.));
#25141=DIRECTION('',(-1.,0.,0.));
#25142=DIRECTION('',(0.,1.,0.));
#25143=DIRECTION('',(-1.,0.,0.));
#25144=DIRECTION('center_axis',(1.,0.,0.));
#25145=DIRECTION('ref_axis',(0.,0.,-1.));
#25146=DIRECTION('',(0.,0.,-1.));
#25147=DIRECTION('',(0.,1.,0.));
#25148=DIRECTION('',(0.,0.,-1.));
#25149=DIRECTION('center_axis',(0.710721462348357,0.,0.703473526834815));
#25150=DIRECTION('ref_axis',(0.703473526834815,0.,-0.710721462348357));
#25151=DIRECTION('',(0.703473526834815,0.,-0.710721462348357));
#25152=DIRECTION('',(0.703473526834815,0.,-0.710721462348357));
#25153=DIRECTION('center_axis',(1.,0.,0.));
#25154=DIRECTION('ref_axis',(0.,0.,-1.));
#25155=DIRECTION('',(0.,0.,-1.));
#25156=DIRECTION('',(0.,1.,0.));
#25157=DIRECTION('',(0.,0.,-1.));
#25158=DIRECTION('',(0.,1.,0.));
#25159=DIRECTION('center_axis',(0.,0.,1.));
#25160=DIRECTION('ref_axis',(1.,0.,0.));
#25161=DIRECTION('',(1.,0.,0.));
#25162=DIRECTION('',(1.,0.,0.));
#25163=DIRECTION('',(0.,1.,0.));
#25164=DIRECTION('center_axis',(0.710721462348357,0.,0.703473526834815));
#25165=DIRECTION('ref_axis',(0.703473526834815,0.,-0.710721462348357));
#25166=DIRECTION('',(0.703473526834815,0.,-0.710721462348357));
#25167=DIRECTION('',(0.703473526834815,0.,-0.710721462348357));
#25168=DIRECTION('',(0.,1.,0.));
#25169=DIRECTION('center_axis',(1.,0.,0.));
#25170=DIRECTION('ref_axis',(0.,0.,-1.));
#25171=DIRECTION('',(0.,0.,1.));
#25172=DIRECTION('',(0.,0.,-1.));
#25173=DIRECTION('center_axis',(-1.,0.,0.));
#25174=DIRECTION('ref_axis',(0.,0.,1.));
#25175=DIRECTION('',(0.,0.,1.));
#25176=DIRECTION('',(0.,1.,0.));
#25177=DIRECTION('',(0.,0.,1.));
#25178=DIRECTION('',(0.,1.,0.));
#25179=DIRECTION('center_axis',(0.,0.,-1.));
#25180=DIRECTION('ref_axis',(-1.,0.,0.));
#25181=DIRECTION('',(-1.,0.,0.));
#25182=DIRECTION('',(0.,1.,0.));
#25183=DIRECTION('',(-1.,0.,0.));
#25184=DIRECTION('center_axis',(-1.,0.,0.));
#25185=DIRECTION('ref_axis',(0.,0.,1.));
#25186=DIRECTION('',(0.,0.,1.));
#25187=DIRECTION('',(0.,1.,0.));
#25188=DIRECTION('',(0.,0.,1.));
#25189=DIRECTION('center_axis',(0.,0.,1.));
#25190=DIRECTION('ref_axis',(1.,0.,0.));
#25191=DIRECTION('',(1.,0.,0.));
#25192=DIRECTION('',(0.,1.,0.));
#25193=DIRECTION('',(1.,0.,0.));
#25194=DIRECTION('center_axis',(-1.,0.,0.));
#25195=DIRECTION('ref_axis',(0.,0.,1.));
#25196=DIRECTION('',(0.,0.,1.));
#25197=DIRECTION('',(0.,1.,0.));
#25198=DIRECTION('',(0.,0.,1.));
#25199=DIRECTION('center_axis',(-0.710721462348357,0.,-0.703473526834815));
#25200=DIRECTION('ref_axis',(-0.703473526834815,0.,0.710721462348357));
#25201=DIRECTION('',(-0.703473526834815,0.,0.710721462348357));
#25202=DIRECTION('',(0.,1.,0.));
#25203=DIRECTION('',(-0.703473526834815,0.,0.710721462348357));
#25204=DIRECTION('center_axis',(0.,0.,-1.));
#25205=DIRECTION('ref_axis',(-1.,0.,0.));
#25206=DIRECTION('',(-1.,0.,0.));
#25207=DIRECTION('',(0.,1.,0.));
#25208=DIRECTION('',(1.,0.,0.));
#25209=DIRECTION('center_axis',(1.,0.,0.));
#25210=DIRECTION('ref_axis',(0.,0.,-1.));
#25211=DIRECTION('',(0.,0.,-1.));
#25212=DIRECTION('',(0.,1.,0.));
#25213=DIRECTION('',(0.,0.,-1.));
#25214=DIRECTION('center_axis',(0.,0.,-1.));
#25215=DIRECTION('ref_axis',(-1.,0.,0.));
#25216=DIRECTION('',(-1.,0.,0.));
#25217=DIRECTION('',(0.,1.,0.));
#25218=DIRECTION('',(-1.,0.,0.));
#25219=DIRECTION('center_axis',(0.710721462348357,0.,-0.703473526834815));
#25220=DIRECTION('ref_axis',(-0.703473526834815,0.,-0.710721462348357));
#25221=DIRECTION('',(-0.703473526834815,0.,-0.710721462348357));
#25222=DIRECTION('',(0.,1.,0.));
#25223=DIRECTION('',(-0.703473526834815,0.,-0.710721462348357));
#25224=DIRECTION('center_axis',(1.,0.,0.));
#25225=DIRECTION('ref_axis',(0.,0.,-1.));
#25226=DIRECTION('',(0.,0.,1.));
#25227=DIRECTION('',(0.,0.,-1.));
#25228=DIRECTION('center_axis',(0.,1.,0.));
#25229=DIRECTION('ref_axis',(1.,0.,0.));
#25230=DIRECTION('center_axis',(0.,1.,0.));
#25231=DIRECTION('ref_axis',(1.,0.,0.));
#25232=DIRECTION('',(0.,-1.,0.));
#25233=DIRECTION('center_axis',(0.,1.,0.));
#25234=DIRECTION('ref_axis',(-1.,0.,0.));
#25235=DIRECTION('center_axis',(0.,0.,1.));
#25236=DIRECTION('ref_axis',(1.,0.,0.));
#25237=DIRECTION('',(1.,0.,0.));
#25238=DIRECTION('',(0.,1.,0.));
#25239=DIRECTION('',(-1.,0.,0.));
#25240=DIRECTION('center_axis',(0.,0.,1.));
#25241=DIRECTION('ref_axis',(1.,0.,0.));
#25242=DIRECTION('',(-1.,0.,0.));
#25243=DIRECTION('',(1.,0.,0.));
#25244=DIRECTION('',(0.,1.,0.));
#25245=DIRECTION('center_axis',(-1.,0.,0.));
#25246=DIRECTION('ref_axis',(0.,0.,1.));
#25247=DIRECTION('',(0.,0.,1.));
#25248=DIRECTION('',(0.,0.,1.));
#25249=DIRECTION('',(0.,1.,0.));
#25250=DIRECTION('center_axis',(0.,0.,1.));
#25251=DIRECTION('ref_axis',(1.,0.,0.));
#25252=DIRECTION('',(1.,0.,0.));
#25253=DIRECTION('',(1.,0.,0.));
#25254=DIRECTION('',(0.,1.,0.));
#25255=DIRECTION('center_axis',(-1.,0.,0.));
#25256=DIRECTION('ref_axis',(0.,0.,1.));
#25257=DIRECTION('',(0.,0.,1.));
#25258=DIRECTION('',(0.,0.,1.));
#25259=DIRECTION('',(0.,1.,0.));
#25260=DIRECTION('center_axis',(0.,0.,-1.));
#25261=DIRECTION('ref_axis',(-1.,0.,0.));
#25262=DIRECTION('',(-1.,0.,0.));
#25263=DIRECTION('',(-1.,0.,0.));
#25264=DIRECTION('',(0.,1.,0.));
#25265=DIRECTION('center_axis',(-1.,0.,0.));
#25266=DIRECTION('ref_axis',(0.,0.,1.));
#25267=DIRECTION('',(0.,0.,1.));
#25268=DIRECTION('',(0.,0.,1.));
#25269=DIRECTION('',(0.,1.,0.));
#25270=DIRECTION('center_axis',(-0.710721462348357,0.,0.703473526834815));
#25271=DIRECTION('ref_axis',(0.703473526834815,0.,0.710721462348357));
#25272=DIRECTION('',(0.703473526834815,0.,0.710721462348357));
#25273=DIRECTION('',(0.703473526834815,0.,0.710721462348357));
#25274=DIRECTION('center_axis',(0.,0.,1.));
#25275=DIRECTION('ref_axis',(1.,0.,0.));
#25276=DIRECTION('',(1.,0.,0.));
#25277=DIRECTION('',(0.,1.,0.));
#25278=DIRECTION('',(1.,0.,0.));
#25279=DIRECTION('',(0.,1.,0.));
#25280=DIRECTION('center_axis',(0.,-1.,0.));
#25281=DIRECTION('ref_axis',(1.,0.,0.));
#25282=DIRECTION('center_axis',(0.,1.,0.));
#25283=DIRECTION('ref_axis',(1.,0.,0.));
#25284=DIRECTION('center_axis',(0.,1.,0.));
#25285=DIRECTION('ref_axis',(1.,0.,0.));
#25286=DIRECTION('',(0.,1.,0.));
#25287=DIRECTION('center_axis',(1.,0.,-3.86959901105515E-16));
#25288=DIRECTION('ref_axis',(-3.86959901105515E-16,0.,-1.));
#25289=DIRECTION('',(-3.86959901105515E-16,0.,-1.));
#25290=DIRECTION('',(-3.86959901105515E-16,0.,-1.));
#25291=DIRECTION('',(0.,1.,0.));
#25292=DIRECTION('center_axis',(0.,-1.,0.));
#25293=DIRECTION('ref_axis',(0.,0.,-1.));
#25294=DIRECTION('center_axis',(0.,1.,0.));
#25295=DIRECTION('ref_axis',(0.,0.,-1.));
#25296=DIRECTION('center_axis',(0.,1.,0.));
#25297=DIRECTION('ref_axis',(0.,0.,-1.));
#25298=DIRECTION('',(0.,1.,0.));
#25299=DIRECTION('center_axis',(0.710721462348357,0.,0.703473526834815));
#25300=DIRECTION('ref_axis',(0.703473526834815,0.,-0.710721462348357));
#25301=DIRECTION('',(0.703473526834815,0.,-0.710721462348357));
#25302=DIRECTION('',(0.,1.,0.));
#25303=DIRECTION('',(0.703473526834815,0.,-0.710721462348357));
#25304=DIRECTION('',(0.,1.,0.));
#25305=DIRECTION('center_axis',(1.,0.,0.));
#25306=DIRECTION('ref_axis',(0.,0.,-1.));
#25307=DIRECTION('',(0.,0.,-1.));
#25308=DIRECTION('',(0.,0.,-1.));
#25309=DIRECTION('',(0.,1.,0.));
#25310=DIRECTION('center_axis',(0.,0.,-1.));
#25311=DIRECTION('ref_axis',(-1.,0.,0.));
#25312=DIRECTION('',(-1.,0.,0.));
#25313=DIRECTION('',(-1.,0.,0.));
#25314=DIRECTION('',(0.,1.,0.));
#25315=DIRECTION('center_axis',(1.,0.,0.));
#25316=DIRECTION('ref_axis',(0.,0.,-1.));
#25317=DIRECTION('',(0.,0.,-1.));
#25318=DIRECTION('',(0.,0.,-1.));
#25319=DIRECTION('',(0.,1.,0.));
#25320=DIRECTION('center_axis',(0.,0.,1.));
#25321=DIRECTION('ref_axis',(1.,0.,0.));
#25322=DIRECTION('',(1.,0.,0.));
#25323=DIRECTION('',(1.,0.,0.));
#25324=DIRECTION('',(0.,1.,0.));
#25325=DIRECTION('center_axis',(1.,0.,0.));
#25326=DIRECTION('ref_axis',(0.,0.,-1.));
#25327=DIRECTION('',(0.,0.,-1.));
#25328=DIRECTION('',(0.,0.,-1.));
#25329=DIRECTION('',(0.,1.,0.));
#25330=DIRECTION('center_axis',(0.,0.,1.));
#25331=DIRECTION('ref_axis',(1.,0.,0.));
#25332=DIRECTION('',(-1.,0.,0.));
#25333=DIRECTION('',(1.,0.,0.));
#25334=DIRECTION('center_axis',(0.,0.,-1.));
#25335=DIRECTION('ref_axis',(-1.,0.,0.));
#25336=DIRECTION('',(-1.,0.,0.));
#25337=DIRECTION('',(1.,0.,0.));
#25338=DIRECTION('',(0.,1.,0.));
#25339=DIRECTION('center_axis',(-1.,0.,0.));
#25340=DIRECTION('ref_axis',(0.,0.,1.));
#25341=DIRECTION('',(0.,0.,1.));
#25342=DIRECTION('',(0.,0.,1.));
#25343=DIRECTION('',(0.,1.,0.));
#25344=DIRECTION('center_axis',(0.,0.,-1.));
#25345=DIRECTION('ref_axis',(-1.,0.,0.));
#25346=DIRECTION('',(-1.,0.,0.));
#25347=DIRECTION('',(-1.,0.,0.));
#25348=DIRECTION('',(0.,1.,0.));
#25349=DIRECTION('center_axis',(-0.710721462348357,0.,-0.703473526834815));
#25350=DIRECTION('ref_axis',(-0.703473526834815,0.,0.710721462348357));
#25351=DIRECTION('',(-0.703473526834815,0.,0.710721462348357));
#25352=DIRECTION('',(-0.703473526834815,0.,0.710721462348357));
#25353=DIRECTION('',(0.,1.,0.));
#25354=DIRECTION('center_axis',(0.,-1.,0.));
#25355=DIRECTION('ref_axis',(0.,0.,1.));
#25356=DIRECTION('center_axis',(0.,1.,0.));
#25357=DIRECTION('ref_axis',(0.,0.,1.));
#25358=DIRECTION('',(0.,1.,0.));
#25359=DIRECTION('center_axis',(0.,1.,0.));
#25360=DIRECTION('ref_axis',(0.,0.,1.));
#25361=DIRECTION('center_axis',(-1.,0.,-1.93479950552757E-16));
#25362=DIRECTION('ref_axis',(-1.93479950552757E-16,0.,1.));
#25363=DIRECTION('',(-1.93479950552757E-16,0.,1.));
#25364=DIRECTION('',(0.,1.,0.));
#25365=DIRECTION('',(-1.93479950552757E-16,0.,1.));
#25366=DIRECTION('center_axis',(0.,-1.,0.));
#25367=DIRECTION('ref_axis',(-1.,0.,-1.77635683940026E-14));
#25368=DIRECTION('center_axis',(0.,1.,0.));
#25369=DIRECTION('ref_axis',(-1.,0.,-1.77635683940026E-14));
#25370=DIRECTION('',(0.,1.,0.));
#25371=DIRECTION('center_axis',(0.,1.,0.));
#25372=DIRECTION('ref_axis',(-1.,0.,-1.77635683940026E-14));
#25373=DIRECTION('center_axis',(0.,0.,-1.));
#25374=DIRECTION('ref_axis',(-1.,0.,0.));
#25375=DIRECTION('',(-1.,0.,0.));
#25376=DIRECTION('',(-1.,0.,0.));
#25377=DIRECTION('center_axis',(0.,0.,1.));
#25378=DIRECTION('ref_axis',(1.,0.,0.));
#25379=DIRECTION('',(1.,0.,0.));
#25380=DIRECTION('',(0.,1.,0.));
#25381=DIRECTION('',(1.,0.,0.));
#25382=DIRECTION('center_axis',(-0.710721462348357,0.,0.703473526834815));
#25383=DIRECTION('ref_axis',(0.703473526834815,0.,0.710721462348357));
#25384=DIRECTION('',(0.703473526834815,0.,0.710721462348357));
#25385=DIRECTION('',(0.,1.,0.));
#25386=DIRECTION('',(0.703473526834815,0.,0.710721462348357));
#25387=DIRECTION('center_axis',(-1.,0.,0.));
#25388=DIRECTION('ref_axis',(0.,0.,1.));
#25389=DIRECTION('',(0.,0.,1.));
#25390=DIRECTION('',(0.,1.,0.));
#25391=DIRECTION('',(0.,0.,1.));
#25392=DIRECTION('center_axis',(0.,0.,-1.));
#25393=DIRECTION('ref_axis',(-1.,0.,0.));
#25394=DIRECTION('',(-1.,0.,0.));
#25395=DIRECTION('',(0.,1.,0.));
#25396=DIRECTION('',(-1.,0.,0.));
#25397=DIRECTION('center_axis',(-1.,0.,0.));
#25398=DIRECTION('ref_axis',(0.,0.,1.));
#25399=DIRECTION('',(0.,0.,1.));
#25400=DIRECTION('',(0.,1.,0.));
#25401=DIRECTION('',(0.,0.,1.));
#25402=DIRECTION('center_axis',(0.,0.,1.));
#25403=DIRECTION('ref_axis',(1.,0.,0.));
#25404=DIRECTION('',(1.,0.,0.));
#25405=DIRECTION('',(0.,1.,0.));
#25406=DIRECTION('',(1.,0.,0.));
#25407=DIRECTION('center_axis',(-1.,0.,0.));
#25408=DIRECTION('ref_axis',(0.,0.,1.));
#25409=DIRECTION('',(0.,0.,1.));
#25410=DIRECTION('',(0.,1.,0.));
#25411=DIRECTION('',(0.,0.,1.));
#25412=DIRECTION('center_axis',(0.,0.,1.));
#25413=DIRECTION('ref_axis',(1.,0.,0.));
#25414=DIRECTION('',(1.,0.,0.));
#25415=DIRECTION('',(0.,1.,0.));
#25416=DIRECTION('',(1.,0.,0.));
#25417=DIRECTION('center_axis',(0.,-1.,0.));
#25418=DIRECTION('ref_axis',(-1.,0.,0.));
#25419=DIRECTION('center_axis',(0.,-1.,0.));
#25420=DIRECTION('ref_axis',(-1.,0.,0.));
#25421=DIRECTION('',(0.,1.,0.));
#25422=DIRECTION('center_axis',(0.,-1.,0.));
#25423=DIRECTION('ref_axis',(-1.,0.,0.));
#25424=DIRECTION('center_axis',(1.,0.,0.));
#25425=DIRECTION('ref_axis',(0.,0.,-1.));
#25426=DIRECTION('',(0.,0.,-1.));
#25427=DIRECTION('',(0.,1.,0.));
#25428=DIRECTION('',(0.,0.,-1.));
#25429=DIRECTION('center_axis',(0.,0.,-1.));
#25430=DIRECTION('ref_axis',(-1.,0.,0.));
#25431=DIRECTION('',(-1.,0.,0.));
#25432=DIRECTION('',(0.,1.,0.));
#25433=DIRECTION('',(-1.,0.,0.));
#25434=DIRECTION('center_axis',(1.,0.,2.57947203208822E-15));
#25435=DIRECTION('ref_axis',(2.57947203208822E-15,0.,-1.));
#25436=DIRECTION('',(2.57947203208822E-15,0.,-1.));
#25437=DIRECTION('',(0.,1.,0.));
#25438=DIRECTION('',(2.57947203208822E-15,0.,-1.));
#25439=DIRECTION('center_axis',(-2.26980252028671E-15,0.,-1.));
#25440=DIRECTION('ref_axis',(-1.,0.,2.26980252028671E-15));
#25441=DIRECTION('',(-1.,0.,2.26980252028671E-15));
#25442=DIRECTION('',(0.,1.,0.));
#25443=DIRECTION('',(-1.,0.,2.26980252028671E-15));
#25444=DIRECTION('center_axis',(-1.,0.,0.));
#25445=DIRECTION('ref_axis',(0.,0.,1.));
#25446=DIRECTION('',(0.,0.,1.));
#25447=DIRECTION('',(0.,1.,0.));
#25448=DIRECTION('',(0.,0.,1.));
#25449=DIRECTION('center_axis',(0.,0.,-1.));
#25450=DIRECTION('ref_axis',(-1.,0.,0.));
#25451=DIRECTION('',(-1.,0.,0.));
#25452=DIRECTION('',(0.,1.,0.));
#25453=DIRECTION('',(-1.,0.,0.));
#25454=DIRECTION('center_axis',(0.710721462348357,0.,-0.703473526834815));
#25455=DIRECTION('ref_axis',(-0.703473526834815,0.,-0.710721462348357));
#25456=DIRECTION('',(-0.703473526834815,0.,-0.710721462348357));
#25457=DIRECTION('',(0.,1.,0.));
#25458=DIRECTION('',(-0.703473526834815,0.,-0.710721462348357));
#25459=DIRECTION('center_axis',(0.,1.,0.));
#25460=DIRECTION('ref_axis',(1.,0.,0.));
#25461=DIRECTION('',(-1.,0.,0.));
#25462=DIRECTION('',(0.,0.,1.));
#25463=DIRECTION('',(1.,0.,0.));
#25464=DIRECTION('',(0.,0.,1.));
#25465=DIRECTION('',(-1.,0.,0.));
#25466=DIRECTION('',(0.,0.,1.));
#25467=DIRECTION('',(0.703473526834815,0.,0.710721462348357));
#25468=DIRECTION('',(1.,0.,0.));
#25469=DIRECTION('',(0.703473526834815,0.,-0.710721462348357));
#25470=DIRECTION('',(0.,0.,-1.));
#25471=DIRECTION('',(-1.,0.,0.));
#25472=DIRECTION('',(0.,0.,-1.));
#25473=DIRECTION('',(1.,0.,0.));
#25474=DIRECTION('',(0.,0.,-1.));
#25475=DIRECTION('',(1.,0.,0.));
#25476=DIRECTION('center_axis',(0.,1.,0.));
#25477=DIRECTION('ref_axis',(-1.,0.,0.));
#25478=DIRECTION('',(0.,0.,1.));
#25479=DIRECTION('',(-1.,0.,0.));
#25480=DIRECTION('',(2.57947203208822E-15,0.,1.));
#25481=DIRECTION('',(-1.,0.,-2.26980252028671E-15));
#25482=DIRECTION('',(0.,0.,-1.));
#25483=DIRECTION('',(-1.,0.,0.));
#25484=DIRECTION('',(-0.703473526834815,0.,0.710721462348357));
#25485=DIRECTION('',(0.,0.,1.));
#25486=DIRECTION('',(0.,0.,1.));
#25487=DIRECTION('',(-0.703473526834815,0.,-0.710721462348357));
#25488=DIRECTION('',(-1.,0.,0.));
#25489=DIRECTION('',(0.,0.,-1.));
#25490=DIRECTION('',(-1.,0.,0.));
#25491=DIRECTION('center_axis',(0.,-1.,0.));
#25492=DIRECTION('ref_axis',(0.,0.,1.));
#25493=DIRECTION('',(-3.86959901105515E-16,0.,1.));
#25494=DIRECTION('center_axis',(0.,-1.,0.));
#25495=DIRECTION('ref_axis',(1.,0.,0.));
#25496=DIRECTION('',(1.,0.,0.));
#25497=DIRECTION('center_axis',(0.,-1.,0.));
#25498=DIRECTION('ref_axis',(0.,0.,-1.));
#25499=DIRECTION('',(-1.93479950552757E-16,0.,-1.));
#25500=DIRECTION('center_axis',(0.,-1.,0.));
#25501=DIRECTION('ref_axis',(-1.,0.,1.77635683940026E-14));
#25502=DIRECTION('',(-1.,0.,0.));
#25503=DIRECTION('center_axis',(0.,1.,0.));
#25504=DIRECTION('ref_axis',(1.,0.,0.));
#25505=DIRECTION('center_axis',(0.,0.,1.));
#25506=DIRECTION('ref_axis',(1.,0.,0.));
#25507=DIRECTION('',(0.,1.,0.));
#25508=DIRECTION('',(1.,0.,0.));
#25509=DIRECTION('',(0.,1.,0.));
#25510=DIRECTION('center_axis',(0.,1.,0.));
#25511=DIRECTION('ref_axis',(1.,0.,0.));
#25512=DIRECTION('',(0.,1.,0.));
#25513=DIRECTION('center_axis',(0.,-1.,0.));
#25514=DIRECTION('ref_axis',(1.,0.,0.));
#25515=DIRECTION('center_axis',(-1.,0.,-3.86959901105515E-16));
#25516=DIRECTION('ref_axis',(-3.86959901105515E-16,0.,1.));
#25517=DIRECTION('',(0.,1.,0.));
#25518=DIRECTION('',(-3.86959901105515E-16,0.,1.));
#25519=DIRECTION('center_axis',(0.,1.,0.));
#25520=DIRECTION('ref_axis',(0.,0.,1.));
#25521=DIRECTION('',(0.,1.,0.));
#25522=DIRECTION('center_axis',(0.,-1.,0.));
#25523=DIRECTION('ref_axis',(0.,0.,1.));
#25524=DIRECTION('center_axis',(-0.710721462348357,0.,0.703473526834815));
#25525=DIRECTION('ref_axis',(0.703473526834815,0.,0.710721462348357));
#25526=DIRECTION('',(0.,1.,0.));
#25527=DIRECTION('',(0.703473526834815,0.,0.710721462348357));
#25528=DIRECTION('',(0.,1.,0.));
#25529=DIRECTION('center_axis',(-1.,0.,0.));
#25530=DIRECTION('ref_axis',(0.,0.,1.));
#25531=DIRECTION('',(0.,1.,0.));
#25532=DIRECTION('',(0.,0.,1.));
#25533=DIRECTION('center_axis',(0.,0.,-1.));
#25534=DIRECTION('ref_axis',(-1.,0.,0.));
#25535=DIRECTION('',(0.,1.,0.));
#25536=DIRECTION('',(-1.,0.,0.));
#25537=DIRECTION('center_axis',(-1.,0.,0.));
#25538=DIRECTION('ref_axis',(0.,0.,1.));
#25539=DIRECTION('',(0.,1.,0.));
#25540=DIRECTION('',(0.,0.,1.));
#25541=DIRECTION('center_axis',(0.,0.,1.));
#25542=DIRECTION('ref_axis',(1.,0.,0.));
#25543=DIRECTION('',(0.,1.,0.));
#25544=DIRECTION('',(1.,0.,0.));
#25545=DIRECTION('center_axis',(-1.,0.,0.));
#25546=DIRECTION('ref_axis',(0.,0.,1.));
#25547=DIRECTION('',(0.,1.,0.));
#25548=DIRECTION('',(0.,0.,1.));
#25549=DIRECTION('center_axis',(0.,0.,1.));
#25550=DIRECTION('ref_axis',(1.,0.,0.));
#25551=DIRECTION('',(1.,0.,0.));
#25552=DIRECTION('center_axis',(0.,0.,-1.));
#25553=DIRECTION('ref_axis',(-1.,0.,0.));
#25554=DIRECTION('',(0.,1.,0.));
#25555=DIRECTION('',(1.,0.,0.));
#25556=DIRECTION('center_axis',(1.,0.,0.));
#25557=DIRECTION('ref_axis',(0.,0.,-1.));
#25558=DIRECTION('',(0.,1.,0.));
#25559=DIRECTION('',(0.,0.,-1.));
#25560=DIRECTION('center_axis',(0.,0.,-1.));
#25561=DIRECTION('ref_axis',(-1.,0.,0.));
#25562=DIRECTION('',(0.,1.,0.));
#25563=DIRECTION('',(-1.,0.,0.));
#25564=DIRECTION('center_axis',(0.710721462348357,0.,-0.703473526834815));
#25565=DIRECTION('ref_axis',(-0.703473526834815,0.,-0.710721462348357));
#25566=DIRECTION('',(0.,1.,0.));
#25567=DIRECTION('',(-0.703473526834815,0.,-0.710721462348357));
#25568=DIRECTION('center_axis',(1.,0.,0.));
#25569=DIRECTION('ref_axis',(0.,0.,-1.));
#25570=DIRECTION('',(0.,0.,-1.));
#25571=DIRECTION('center_axis',(0.,1.,0.));
#25572=DIRECTION('ref_axis',(1.,0.,0.));
#25573=DIRECTION('center_axis',(0.,-1.,0.));
#25574=DIRECTION('ref_axis',(1.,0.,0.));
#25575=DIRECTION('',(0.,-1.,0.));
#25576=DIRECTION('center_axis',(-1.,0.,0.));
#25577=DIRECTION('ref_axis',(0.,0.,1.));
#25578=DIRECTION('',(0.,1.,0.));
#25579=DIRECTION('',(0.,0.,-1.));
#25580=DIRECTION('center_axis',(0.,1.,0.));
#25581=DIRECTION('ref_axis',(0.,0.,-1.));
#25582=DIRECTION('center_axis',(0.,-1.,0.));
#25583=DIRECTION('ref_axis',(0.,0.,-1.));
#25584=DIRECTION('',(0.,1.,0.));
#25585=DIRECTION('center_axis',(1.,0.,-1.93479950552757E-16));
#25586=DIRECTION('ref_axis',(-1.93479950552757E-16,0.,-1.));
#25587=DIRECTION('',(-1.93479950552757E-16,0.,-1.));
#25588=DIRECTION('',(0.,1.,0.));
#25589=DIRECTION('center_axis',(0.,1.,0.));
#25590=DIRECTION('ref_axis',(-1.,0.,1.77635683940026E-14));
#25591=DIRECTION('center_axis',(0.,-1.,0.));
#25592=DIRECTION('ref_axis',(-1.,0.,1.77635683940026E-14));
#25593=DIRECTION('',(0.,1.,0.));
#25594=DIRECTION('center_axis',(0.,0.,-1.));
#25595=DIRECTION('ref_axis',(-1.,0.,0.));
#25596=DIRECTION('',(-1.,0.,0.));
#25597=DIRECTION('center_axis',(0.,0.,1.));
#25598=DIRECTION('ref_axis',(1.,0.,0.));
#25599=DIRECTION('',(1.,0.,0.));
#25600=DIRECTION('',(0.,1.,0.));
#25601=DIRECTION('center_axis',(0.710721462348357,0.,0.703473526834815));
#25602=DIRECTION('ref_axis',(0.703473526834815,0.,-0.710721462348357));
#25603=DIRECTION('',(0.703473526834815,0.,-0.710721462348357));
#25604=DIRECTION('',(0.,1.,0.));
#25605=DIRECTION('center_axis',(1.,0.,0.));
#25606=DIRECTION('ref_axis',(0.,0.,-1.));
#25607=DIRECTION('',(0.,0.,-1.));
#25608=DIRECTION('',(0.,1.,0.));
#25609=DIRECTION('center_axis',(0.,0.,-1.));
#25610=DIRECTION('ref_axis',(-1.,0.,0.));
#25611=DIRECTION('',(-1.,0.,0.));
#25612=DIRECTION('',(0.,1.,0.));
#25613=DIRECTION('center_axis',(1.,0.,0.));
#25614=DIRECTION('ref_axis',(0.,0.,-1.));
#25615=DIRECTION('',(0.,0.,-1.));
#25616=DIRECTION('',(0.,1.,0.));
#25617=DIRECTION('center_axis',(0.,0.,1.));
#25618=DIRECTION('ref_axis',(1.,0.,0.));
#25619=DIRECTION('',(1.,0.,0.));
#25620=DIRECTION('',(0.,1.,0.));
#25621=DIRECTION('center_axis',(1.,0.,0.));
#25622=DIRECTION('ref_axis',(0.,0.,-1.));
#25623=DIRECTION('',(0.,0.,-1.));
#25624=DIRECTION('',(0.,1.,0.));
#25625=DIRECTION('center_axis',(0.,0.,1.));
#25626=DIRECTION('ref_axis',(1.,0.,0.));
#25627=DIRECTION('',(1.,0.,0.));
#25628=DIRECTION('',(0.,1.,0.));
#25629=DIRECTION('center_axis',(0.,1.,0.));
#25630=DIRECTION('ref_axis',(-1.,0.,0.));
#25631=DIRECTION('center_axis',(0.,1.,0.));
#25632=DIRECTION('ref_axis',(-1.,0.,0.));
#25633=DIRECTION('',(0.,1.,0.));
#25634=DIRECTION('center_axis',(-1.,0.,0.));
#25635=DIRECTION('ref_axis',(0.,0.,1.));
#25636=DIRECTION('',(0.,0.,1.));
#25637=DIRECTION('',(0.,1.,0.));
#25638=DIRECTION('center_axis',(0.,0.,-1.));
#25639=DIRECTION('ref_axis',(-1.,0.,0.));
#25640=DIRECTION('',(-1.,0.,0.));
#25641=DIRECTION('',(0.,1.,0.));
#25642=DIRECTION('center_axis',(-1.,0.,2.57947203208822E-15));
#25643=DIRECTION('ref_axis',(2.57947203208822E-15,0.,1.));
#25644=DIRECTION('',(2.57947203208822E-15,0.,1.));
#25645=DIRECTION('',(0.,1.,0.));
#25646=DIRECTION('center_axis',(2.26980252028671E-15,0.,-1.));
#25647=DIRECTION('ref_axis',(-1.,0.,-2.26980252028671E-15));
#25648=DIRECTION('',(-1.,0.,-2.26980252028671E-15));
#25649=DIRECTION('',(0.,1.,0.));
#25650=DIRECTION('center_axis',(1.,0.,0.));
#25651=DIRECTION('ref_axis',(0.,0.,-1.));
#25652=DIRECTION('',(0.,0.,-1.));
#25653=DIRECTION('',(0.,1.,0.));
#25654=DIRECTION('center_axis',(0.,0.,-1.));
#25655=DIRECTION('ref_axis',(-1.,0.,0.));
#25656=DIRECTION('',(-1.,0.,0.));
#25657=DIRECTION('',(0.,1.,0.));
#25658=DIRECTION('center_axis',(-0.710721462348357,0.,-0.703473526834815));
#25659=DIRECTION('ref_axis',(-0.703473526834815,0.,0.710721462348357));
#25660=DIRECTION('',(-0.703473526834815,0.,0.710721462348357));
#25661=DIRECTION('center_axis',(0.,1.,0.));
#25662=DIRECTION('ref_axis',(1.,0.,0.));
#25663=DIRECTION('axis',(0.,0.,1.));
#25664=DIRECTION('refdir',(1.,0.,0.));
#25665=DIRECTION('center_axis',(0.,-1.,0.));
#25666=DIRECTION('ref_axis',(-1.,0.,0.));
#25667=DIRECTION('',(0.,1.,0.));
#25668=DIRECTION('center_axis',(0.,1.,0.));
#25669=DIRECTION('ref_axis',(-1.,0.,0.));
#25670=DIRECTION('center_axis',(0.,-1.,0.));
#25671=DIRECTION('ref_axis',(-1.,0.,0.));
#25672=DIRECTION('',(0.,1.,0.));
#25673=DIRECTION('center_axis',(0.,-1.,0.));
#25674=DIRECTION('ref_axis',(-1.,0.,0.));
#25675=DIRECTION('',(0.,1.,0.));
#25676=DIRECTION('center_axis',(0.,-1.,0.));
#25677=DIRECTION('ref_axis',(-1.,0.,0.));
#25678=DIRECTION('',(0.,1.,0.));
#25679=DIRECTION('center_axis',(0.,-1.,0.));
#25680=DIRECTION('ref_axis',(-1.,0.,0.));
#25681=DIRECTION('',(0.,1.,0.));
#25682=DIRECTION('center_axis',(0.,-1.,0.));
#25683=DIRECTION('ref_axis',(-1.,0.,0.));
#25684=DIRECTION('',(0.,1.,0.));
#25685=DIRECTION('center_axis',(0.,-1.,0.));
#25686=DIRECTION('ref_axis',(-1.,0.,0.));
#25687=DIRECTION('',(0.,1.,0.));
#25688=DIRECTION('center_axis',(0.,-1.,0.));
#25689=DIRECTION('ref_axis',(-1.,0.,0.));
#25690=DIRECTION('',(0.,1.,0.));
#25691=DIRECTION('center_axis',(0.,-1.,0.));
#25692=DIRECTION('ref_axis',(-1.,0.,0.));
#25693=DIRECTION('',(0.,1.,0.));
#25694=DIRECTION('center_axis',(0.,-1.,0.));
#25695=DIRECTION('ref_axis',(-1.,0.,0.));
#25696=DIRECTION('',(0.,1.,0.));
#25697=DIRECTION('center_axis',(0.,-1.,0.));
#25698=DIRECTION('ref_axis',(-1.,0.,0.));
#25699=DIRECTION('',(0.,1.,0.));
#25700=DIRECTION('center_axis',(0.,-1.,0.));
#25701=DIRECTION('ref_axis',(-1.,0.,0.));
#25702=DIRECTION('',(0.,1.,0.));
#25703=DIRECTION('center_axis',(0.,-1.,0.));
#25704=DIRECTION('ref_axis',(-1.,0.,0.));
#25705=DIRECTION('',(0.,1.,0.));
#25706=DIRECTION('center_axis',(0.,-1.,0.));
#25707=DIRECTION('ref_axis',(-1.,0.,0.));
#25708=DIRECTION('',(0.,1.,0.));
#25709=DIRECTION('center_axis',(0.,-1.,0.));
#25710=DIRECTION('ref_axis',(-1.,0.,0.));
#25711=DIRECTION('',(0.,1.,0.));
#25712=DIRECTION('center_axis',(0.,-1.,0.));
#25713=DIRECTION('ref_axis',(-1.,0.,0.));
#25714=DIRECTION('',(0.,1.,0.));
#25715=DIRECTION('center_axis',(0.,-1.,0.));
#25716=DIRECTION('ref_axis',(-1.,0.,0.));
#25717=DIRECTION('',(0.,1.,0.));
#25718=DIRECTION('center_axis',(0.,-1.,0.));
#25719=DIRECTION('ref_axis',(-1.,0.,0.));
#25720=DIRECTION('',(0.,1.,0.));
#25721=DIRECTION('center_axis',(0.,-1.,0.));
#25722=DIRECTION('ref_axis',(-1.,0.,0.));
#25723=DIRECTION('',(0.,1.,0.));
#25724=DIRECTION('center_axis',(0.,-1.,0.));
#25725=DIRECTION('ref_axis',(-1.,0.,0.));
#25726=DIRECTION('',(0.,1.,0.));
#25727=DIRECTION('center_axis',(0.,-1.,0.));
#25728=DIRECTION('ref_axis',(-1.,0.,0.));
#25729=DIRECTION('',(0.,1.,0.));
#25730=DIRECTION('center_axis',(0.,-1.,0.));
#25731=DIRECTION('ref_axis',(-1.,0.,0.));
#25732=DIRECTION('',(0.,1.,0.));
#25733=DIRECTION('center_axis',(0.,-1.,0.));
#25734=DIRECTION('ref_axis',(-1.,0.,0.));
#25735=DIRECTION('',(0.,1.,0.));
#25736=DIRECTION('center_axis',(0.,-1.,0.));
#25737=DIRECTION('ref_axis',(-1.,0.,0.));
#25738=DIRECTION('',(0.,1.,0.));
#25739=DIRECTION('center_axis',(0.,-1.,0.));
#25740=DIRECTION('ref_axis',(-1.,0.,0.));
#25741=DIRECTION('',(0.,1.,0.));
#25742=DIRECTION('center_axis',(0.,-1.,0.));
#25743=DIRECTION('ref_axis',(-1.,0.,0.));
#25744=DIRECTION('',(0.,1.,0.));
#25745=DIRECTION('center_axis',(0.,-1.,0.));
#25746=DIRECTION('ref_axis',(-1.,0.,0.));
#25747=DIRECTION('',(0.,1.,0.));
#25748=DIRECTION('center_axis',(0.,-1.,0.));
#25749=DIRECTION('ref_axis',(-1.,0.,0.));
#25750=DIRECTION('',(0.,1.,0.));
#25751=DIRECTION('center_axis',(0.,-1.,0.));
#25752=DIRECTION('ref_axis',(-1.,0.,0.));
#25753=DIRECTION('',(0.,1.,0.));
#25754=DIRECTION('center_axis',(0.,-1.,0.));
#25755=DIRECTION('ref_axis',(-1.,0.,0.));
#25756=DIRECTION('',(0.,1.,0.));
#25757=DIRECTION('center_axis',(0.,-1.,0.));
#25758=DIRECTION('ref_axis',(-1.,0.,0.));
#25759=DIRECTION('',(0.,1.,0.));
#25760=DIRECTION('center_axis',(0.,-1.,0.));
#25761=DIRECTION('ref_axis',(-1.,0.,0.));
#25762=DIRECTION('',(0.,1.,0.));
#25763=DIRECTION('center_axis',(0.,-1.,0.));
#25764=DIRECTION('ref_axis',(-1.,0.,0.));
#25765=DIRECTION('',(0.,1.,0.));
#25766=DIRECTION('center_axis',(0.,-1.,0.));
#25767=DIRECTION('ref_axis',(-1.,0.,0.));
#25768=DIRECTION('',(0.,1.,0.));
#25769=DIRECTION('center_axis',(0.,-1.,0.));
#25770=DIRECTION('ref_axis',(-1.,0.,0.));
#25771=DIRECTION('',(0.,1.,0.));
#25772=DIRECTION('center_axis',(0.,-1.,0.));
#25773=DIRECTION('ref_axis',(-1.,0.,0.));
#25774=DIRECTION('',(0.,1.,0.));
#25775=DIRECTION('center_axis',(0.,-1.,0.));
#25776=DIRECTION('ref_axis',(-1.,0.,0.));
#25777=DIRECTION('',(0.,1.,0.));
#25778=DIRECTION('center_axis',(0.,-1.,0.));
#25779=DIRECTION('ref_axis',(-1.,0.,0.));
#25780=DIRECTION('',(0.,1.,0.));
#25781=DIRECTION('center_axis',(0.,-1.,0.));
#25782=DIRECTION('ref_axis',(-1.,0.,0.));
#25783=DIRECTION('',(0.,1.,0.));
#25784=DIRECTION('center_axis',(0.,-1.,0.));
#25785=DIRECTION('ref_axis',(-1.,0.,0.));
#25786=DIRECTION('',(0.,1.,0.));
#25787=DIRECTION('center_axis',(0.,-1.,0.));
#25788=DIRECTION('ref_axis',(-1.,0.,0.));
#25789=DIRECTION('',(0.,1.,0.));
#25790=DIRECTION('center_axis',(0.,-1.,0.));
#25791=DIRECTION('ref_axis',(-1.,0.,0.));
#25792=DIRECTION('',(0.,1.,0.));
#25793=DIRECTION('center_axis',(0.,-1.,0.));
#25794=DIRECTION('ref_axis',(-1.,0.,0.));
#25795=DIRECTION('',(0.,1.,0.));
#25796=DIRECTION('center_axis',(0.,-1.,0.));
#25797=DIRECTION('ref_axis',(-1.,0.,0.));
#25798=DIRECTION('',(0.,1.,0.));
#25799=DIRECTION('center_axis',(0.,-1.,0.));
#25800=DIRECTION('ref_axis',(-1.,0.,0.));
#25801=DIRECTION('',(0.,1.,0.));
#25802=DIRECTION('center_axis',(0.,-1.,0.));
#25803=DIRECTION('ref_axis',(-1.,0.,0.));
#25804=DIRECTION('',(0.,1.,0.));
#25805=DIRECTION('center_axis',(0.,-1.,0.));
#25806=DIRECTION('ref_axis',(-1.,0.,0.));
#25807=DIRECTION('',(0.,1.,0.));
#25808=DIRECTION('center_axis',(0.,-1.,0.));
#25809=DIRECTION('ref_axis',(-1.,0.,0.));
#25810=DIRECTION('',(0.,1.,0.));
#25811=DIRECTION('center_axis',(0.,-1.,0.));
#25812=DIRECTION('ref_axis',(-1.,0.,0.));
#25813=DIRECTION('',(0.,1.,0.));
#25814=DIRECTION('center_axis',(0.,-1.,0.));
#25815=DIRECTION('ref_axis',(-1.,0.,0.));
#25816=DIRECTION('',(0.,1.,0.));
#25817=DIRECTION('center_axis',(0.,-1.,0.));
#25818=DIRECTION('ref_axis',(-1.,0.,0.));
#25819=DIRECTION('',(0.,1.,0.));
#25820=DIRECTION('center_axis',(0.,-1.,0.));
#25821=DIRECTION('ref_axis',(-1.,0.,0.));
#25822=DIRECTION('',(0.,1.,0.));
#25823=DIRECTION('center_axis',(0.,-1.,0.));
#25824=DIRECTION('ref_axis',(-1.,0.,0.));
#25825=DIRECTION('',(0.,1.,0.));
#25826=DIRECTION('center_axis',(0.,-1.,0.));
#25827=DIRECTION('ref_axis',(-1.,0.,0.));
#25828=DIRECTION('',(0.,1.,0.));
#25829=DIRECTION('center_axis',(0.,-1.,0.));
#25830=DIRECTION('ref_axis',(-1.,0.,0.));
#25831=DIRECTION('',(0.,1.,0.));
#25832=DIRECTION('center_axis',(0.,-1.,0.));
#25833=DIRECTION('ref_axis',(-1.,0.,0.));
#25834=DIRECTION('',(0.,1.,0.));
#25835=DIRECTION('center_axis',(0.,-1.,0.));
#25836=DIRECTION('ref_axis',(-1.,0.,0.));
#25837=DIRECTION('',(0.,1.,0.));
#25838=DIRECTION('center_axis',(0.,-1.,0.));
#25839=DIRECTION('ref_axis',(-1.,0.,0.));
#25840=DIRECTION('',(0.,1.,0.));
#25841=DIRECTION('center_axis',(0.,-1.,0.));
#25842=DIRECTION('ref_axis',(-1.,0.,0.));
#25843=DIRECTION('',(0.,1.,0.));
#25844=DIRECTION('center_axis',(0.,-1.,0.));
#25845=DIRECTION('ref_axis',(-1.,0.,0.));
#25846=DIRECTION('',(0.,1.,0.));
#25847=DIRECTION('center_axis',(0.,-1.,0.));
#25848=DIRECTION('ref_axis',(-1.,0.,0.));
#25849=DIRECTION('',(0.,1.,0.));
#25850=DIRECTION('center_axis',(0.,-1.,0.));
#25851=DIRECTION('ref_axis',(-1.,0.,0.));
#25852=DIRECTION('',(0.,1.,0.));
#25853=DIRECTION('center_axis',(0.,-1.,0.));
#25854=DIRECTION('ref_axis',(-1.,0.,0.));
#25855=DIRECTION('',(0.,1.,0.));
#25856=DIRECTION('center_axis',(0.,-1.,0.));
#25857=DIRECTION('ref_axis',(-1.,0.,0.));
#25858=DIRECTION('',(0.,1.,0.));
#25859=DIRECTION('center_axis',(0.,-1.,0.));
#25860=DIRECTION('ref_axis',(-1.,0.,0.));
#25861=DIRECTION('',(0.,1.,0.));
#25862=DIRECTION('center_axis',(0.,-1.,0.));
#25863=DIRECTION('ref_axis',(-1.,0.,0.));
#25864=DIRECTION('',(0.,1.,0.));
#25865=DIRECTION('center_axis',(0.,-1.,0.));
#25866=DIRECTION('ref_axis',(-1.,0.,0.));
#25867=DIRECTION('',(0.,1.,0.));
#25868=DIRECTION('center_axis',(0.,-1.,0.));
#25869=DIRECTION('ref_axis',(-1.,0.,0.));
#25870=DIRECTION('',(0.,1.,0.));
#25871=DIRECTION('center_axis',(0.,-1.,0.));
#25872=DIRECTION('ref_axis',(-1.,0.,0.));
#25873=DIRECTION('',(0.,1.,0.));
#25874=DIRECTION('center_axis',(0.,-1.,0.));
#25875=DIRECTION('ref_axis',(-1.,0.,0.));
#25876=DIRECTION('',(0.,1.,0.));
#25877=DIRECTION('center_axis',(0.,-1.,0.));
#25878=DIRECTION('ref_axis',(-1.,0.,0.));
#25879=DIRECTION('',(0.,1.,0.));
#25880=DIRECTION('center_axis',(0.,-1.,0.));
#25881=DIRECTION('ref_axis',(-1.,0.,0.));
#25882=DIRECTION('',(0.,1.,0.));
#25883=DIRECTION('center_axis',(0.,-1.,0.));
#25884=DIRECTION('ref_axis',(-1.,0.,0.));
#25885=DIRECTION('',(0.,1.,0.));
#25886=DIRECTION('center_axis',(0.,-1.,0.));
#25887=DIRECTION('ref_axis',(-1.,0.,0.));
#25888=DIRECTION('',(0.,1.,0.));
#25889=DIRECTION('center_axis',(0.,-1.,0.));
#25890=DIRECTION('ref_axis',(-1.,0.,0.));
#25891=DIRECTION('',(0.,1.,0.));
#25892=DIRECTION('center_axis',(0.,-1.,0.));
#25893=DIRECTION('ref_axis',(-1.,0.,0.));
#25894=DIRECTION('',(0.,1.,0.));
#25895=DIRECTION('center_axis',(0.,-1.,0.));
#25896=DIRECTION('ref_axis',(-1.,0.,0.));
#25897=DIRECTION('',(0.,1.,0.));
#25898=DIRECTION('center_axis',(0.,-1.,0.));
#25899=DIRECTION('ref_axis',(-1.,0.,0.));
#25900=DIRECTION('',(0.,1.,0.));
#25901=DIRECTION('center_axis',(0.,-1.,0.));
#25902=DIRECTION('ref_axis',(-1.,0.,0.));
#25903=DIRECTION('',(0.,1.,0.));
#25904=DIRECTION('center_axis',(0.,-1.,0.));
#25905=DIRECTION('ref_axis',(-1.,0.,0.));
#25906=DIRECTION('',(0.,1.,0.));
#25907=DIRECTION('center_axis',(0.,-1.,0.));
#25908=DIRECTION('ref_axis',(-1.,0.,0.));
#25909=DIRECTION('',(0.,1.,0.));
#25910=DIRECTION('center_axis',(0.,-1.,0.));
#25911=DIRECTION('ref_axis',(-1.,0.,0.));
#25912=DIRECTION('',(0.,1.,0.));
#25913=DIRECTION('center_axis',(0.,-1.,0.));
#25914=DIRECTION('ref_axis',(-1.,0.,0.));
#25915=DIRECTION('',(0.,1.,0.));
#25916=DIRECTION('center_axis',(0.,-1.,0.));
#25917=DIRECTION('ref_axis',(-1.,0.,0.));
#25918=DIRECTION('',(0.,1.,0.));
#25919=DIRECTION('center_axis',(0.,-1.,0.));
#25920=DIRECTION('ref_axis',(-1.,0.,0.));
#25921=DIRECTION('',(0.,1.,0.));
#25922=DIRECTION('center_axis',(0.,-1.,0.));
#25923=DIRECTION('ref_axis',(-1.,0.,0.));
#25924=DIRECTION('',(0.,1.,0.));
#25925=DIRECTION('center_axis',(0.,-1.,0.));
#25926=DIRECTION('ref_axis',(-1.,0.,0.));
#25927=DIRECTION('',(0.,1.,0.));
#25928=DIRECTION('center_axis',(0.,-1.,0.));
#25929=DIRECTION('ref_axis',(-1.,0.,0.));
#25930=DIRECTION('',(0.,1.,0.));
#25931=DIRECTION('center_axis',(0.,-1.,0.));
#25932=DIRECTION('ref_axis',(-1.,0.,0.));
#25933=DIRECTION('',(0.,1.,0.));
#25934=DIRECTION('center_axis',(0.,-1.,0.));
#25935=DIRECTION('ref_axis',(-1.,0.,0.));
#25936=DIRECTION('',(0.,1.,0.));
#25937=DIRECTION('center_axis',(0.,-1.,0.));
#25938=DIRECTION('ref_axis',(-1.,0.,0.));
#25939=DIRECTION('',(0.,1.,0.));
#25940=DIRECTION('center_axis',(0.,-1.,0.));
#25941=DIRECTION('ref_axis',(-1.,0.,0.));
#25942=DIRECTION('',(0.,1.,0.));
#25943=DIRECTION('center_axis',(0.,-1.,0.));
#25944=DIRECTION('ref_axis',(-1.,0.,0.));
#25945=DIRECTION('',(0.,1.,0.));
#25946=DIRECTION('center_axis',(0.,-1.,0.));
#25947=DIRECTION('ref_axis',(-1.,0.,0.));
#25948=DIRECTION('',(0.,1.,0.));
#25949=DIRECTION('center_axis',(0.,-1.,0.));
#25950=DIRECTION('ref_axis',(-1.,0.,0.));
#25951=DIRECTION('',(0.,1.,0.));
#25952=DIRECTION('center_axis',(0.,-1.,0.));
#25953=DIRECTION('ref_axis',(-1.,0.,0.));
#25954=DIRECTION('',(0.,1.,0.));
#25955=DIRECTION('center_axis',(0.,-1.,0.));
#25956=DIRECTION('ref_axis',(-1.,0.,0.));
#25957=DIRECTION('',(0.,1.,0.));
#25958=DIRECTION('center_axis',(0.,-1.,0.));
#25959=DIRECTION('ref_axis',(-1.,0.,0.));
#25960=DIRECTION('',(0.,1.,0.));
#25961=DIRECTION('center_axis',(0.,-1.,0.));
#25962=DIRECTION('ref_axis',(-1.,0.,0.));
#25963=DIRECTION('',(0.,1.,0.));
#25964=DIRECTION('center_axis',(0.,-1.,0.));
#25965=DIRECTION('ref_axis',(-1.,0.,0.));
#25966=DIRECTION('',(0.,1.,0.));
#25967=DIRECTION('center_axis',(0.,-1.,0.));
#25968=DIRECTION('ref_axis',(-1.,0.,0.));
#25969=DIRECTION('',(0.,1.,0.));
#25970=DIRECTION('center_axis',(0.,1.,0.));
#25971=DIRECTION('ref_axis',(-1.,0.,0.));
#25972=DIRECTION('center_axis',(0.,1.,0.));
#25973=DIRECTION('ref_axis',(1.,0.,0.));
#25974=DIRECTION('',(0.,-1.,0.));
#25975=DIRECTION('',(0.,-1.,0.));
#25976=DIRECTION('center_axis',(0.,1.,0.));
#25977=DIRECTION('ref_axis',(1.,0.,0.));
#25978=DIRECTION('center_axis',(0.,-1.,0.));
#25979=DIRECTION('ref_axis',(1.,0.,0.));
#25980=DIRECTION('center_axis',(0.,1.,0.));
#25981=DIRECTION('ref_axis',(1.,0.,0.));
#25982=DIRECTION('',(0.,-1.,0.));
#25983=DIRECTION('center_axis',(0.,1.,0.));
#25984=DIRECTION('ref_axis',(1.,0.,0.));
#25985=DIRECTION('',(0.,-1.,0.));
#25986=DIRECTION('center_axis',(0.,1.,0.));
#25987=DIRECTION('ref_axis',(1.,0.,0.));
#25988=DIRECTION('',(0.,-1.,0.));
#25989=DIRECTION('center_axis',(0.,1.,0.));
#25990=DIRECTION('ref_axis',(1.,0.,0.));
#25991=DIRECTION('',(0.,-1.,0.));
#25992=DIRECTION('center_axis',(0.,1.,0.));
#25993=DIRECTION('ref_axis',(1.,0.,0.));
#25994=DIRECTION('',(0.,-1.,0.));
#25995=DIRECTION('center_axis',(0.,1.,0.));
#25996=DIRECTION('ref_axis',(1.,0.,0.));
#25997=DIRECTION('',(0.,-1.,0.));
#25998=DIRECTION('center_axis',(0.,1.,0.));
#25999=DIRECTION('ref_axis',(1.,0.,0.));
#26000=DIRECTION('',(0.,-1.,0.));
#26001=DIRECTION('center_axis',(0.,1.,0.));
#26002=DIRECTION('ref_axis',(1.,0.,0.));
#26003=DIRECTION('',(0.,-1.,0.));
#26004=DIRECTION('center_axis',(0.,1.,0.));
#26005=DIRECTION('ref_axis',(1.,0.,0.));
#26006=DIRECTION('',(0.,-1.,0.));
#26007=DIRECTION('center_axis',(0.,-1.,0.));
#26008=DIRECTION('ref_axis',(1.,0.,0.));
#26009=DIRECTION('center_axis',(0.,1.,0.));
#26010=DIRECTION('ref_axis',(0.409697292977236,0.,0.912221534566645));
#26011=DIRECTION('',(0.,1.,0.));
#26012=DIRECTION('center_axis',(0.,1.,0.));
#26013=DIRECTION('ref_axis',(1.,0.,-6.50117889680365E-14));
#26014=DIRECTION('center_axis',(0.,1.,0.));
#26015=DIRECTION('ref_axis',(1.,0.,-6.50117889680365E-14));
#26016=DIRECTION('',(0.,1.,0.));
#26017=DIRECTION('center_axis',(0.,1.,0.));
#26018=DIRECTION('ref_axis',(1.,0.,-6.50117889680365E-14));
#26019=DIRECTION('',(0.,1.,0.));
#26020=DIRECTION('center_axis',(0.,1.,0.));
#26021=DIRECTION('ref_axis',(1.,0.,-6.50117889680365E-14));
#26022=DIRECTION('',(0.,1.,0.));
#26023=DIRECTION('center_axis',(0.,1.,0.));
#26024=DIRECTION('ref_axis',(1.,0.,-6.50117889680365E-14));
#26025=DIRECTION('',(0.,1.,0.));
#26026=DIRECTION('center_axis',(0.,1.,0.));
#26027=DIRECTION('ref_axis',(1.,0.,-6.50117889680365E-14));
#26028=DIRECTION('',(0.,1.,0.));
#26029=DIRECTION('center_axis',(0.,1.,0.));
#26030=DIRECTION('ref_axis',(1.,0.,-6.50117889680365E-14));
#26031=DIRECTION('',(0.,1.,0.));
#26032=DIRECTION('center_axis',(0.,1.,0.));
#26033=DIRECTION('ref_axis',(1.,0.,-6.50117889680365E-14));
#26034=DIRECTION('',(0.,1.,0.));
#26035=DIRECTION('center_axis',(0.,1.,0.));
#26036=DIRECTION('ref_axis',(1.,0.,-6.50117889680365E-14));
#26037=DIRECTION('',(0.,1.,0.));
#26038=DIRECTION('center_axis',(0.,1.,0.));
#26039=DIRECTION('ref_axis',(1.,0.,-6.50117889680365E-14));
#26040=DIRECTION('',(0.,1.,0.));
#26041=DIRECTION('center_axis',(0.,-1.,0.));
#26042=DIRECTION('ref_axis',(-1.,0.,2.36700689860723E-12));
#26043=DIRECTION('',(0.,-1.,0.));
#26044=DIRECTION('center_axis',(0.,1.,0.));
#26045=DIRECTION('ref_axis',(-1.,0.,2.36700689860723E-12));
#26046=DIRECTION('center_axis',(0.,-1.,0.));
#26047=DIRECTION('ref_axis',(-1.,0.,2.36700689860723E-12));
#26048=DIRECTION('',(0.,-1.,0.));
#26049=DIRECTION('center_axis',(0.,-1.,0.));
#26050=DIRECTION('ref_axis',(-1.,0.,2.36700689860723E-12));
#26051=DIRECTION('',(0.,-1.,0.));
#26052=DIRECTION('center_axis',(0.,-1.,0.));
#26053=DIRECTION('ref_axis',(-1.,0.,2.36700689860723E-12));
#26054=DIRECTION('',(0.,-1.,0.));
#26055=DIRECTION('center_axis',(0.,-1.,0.));
#26056=DIRECTION('ref_axis',(-1.,0.,2.36700689860723E-12));
#26057=DIRECTION('',(0.,-1.,0.));
#26058=DIRECTION('center_axis',(0.,-1.,0.));
#26059=DIRECTION('ref_axis',(-1.,0.,2.36700689860723E-12));
#26060=DIRECTION('',(0.,-1.,0.));
#26061=DIRECTION('center_axis',(0.,-1.,0.));
#26062=DIRECTION('ref_axis',(-1.,0.,2.36700689860723E-12));
#26063=DIRECTION('',(0.,-1.,0.));
#26064=DIRECTION('center_axis',(0.,-1.,0.));
#26065=DIRECTION('ref_axis',(-1.,0.,2.36700689860723E-12));
#26066=DIRECTION('',(0.,-1.,0.));
#26067=DIRECTION('center_axis',(0.,-1.,0.));
#26068=DIRECTION('ref_axis',(-1.,0.,2.36700689860723E-12));
#26069=DIRECTION('',(0.,-1.,0.));
#26070=DIRECTION('center_axis',(0.,-1.,0.));
#26071=DIRECTION('ref_axis',(-1.,0.,2.36700689860723E-12));
#26072=DIRECTION('',(0.,-1.,0.));
#26073=DIRECTION('center_axis',(0.,-1.,0.));
#26074=DIRECTION('ref_axis',(-1.,0.,2.36700689860723E-12));
#26075=DIRECTION('',(0.,-1.,0.));
#26076=DIRECTION('center_axis',(0.,-1.,0.));
#26077=DIRECTION('ref_axis',(-1.,0.,2.36700689860723E-12));
#26078=DIRECTION('',(0.,-1.,0.));
#26079=DIRECTION('center_axis',(0.,-1.,0.));
#26080=DIRECTION('ref_axis',(-1.,0.,2.36700689860723E-12));
#26081=DIRECTION('',(0.,-1.,0.));
#26082=DIRECTION('center_axis',(0.,-1.,0.));
#26083=DIRECTION('ref_axis',(-1.,0.,2.36700689860723E-12));
#26084=DIRECTION('',(0.,-1.,0.));
#26085=DIRECTION('center_axis',(0.,-1.,0.));
#26086=DIRECTION('ref_axis',(-1.,0.,2.36700689860723E-12));
#26087=DIRECTION('',(0.,-1.,0.));
#26088=DIRECTION('center_axis',(0.,-1.,0.));
#26089=DIRECTION('ref_axis',(-1.,0.,2.36700689860723E-12));
#26090=DIRECTION('',(0.,-1.,0.));
#26091=DIRECTION('center_axis',(0.,-1.,0.));
#26092=DIRECTION('ref_axis',(-1.,0.,2.36700689860723E-12));
#26093=DIRECTION('',(0.,-1.,0.));
#26094=DIRECTION('center_axis',(0.,-1.,0.));
#26095=DIRECTION('ref_axis',(-1.,0.,2.36700689860723E-12));
#26096=DIRECTION('',(0.,-1.,0.));
#26097=DIRECTION('center_axis',(0.,-1.,0.));
#26098=DIRECTION('ref_axis',(-1.,0.,2.36700689860723E-12));
#26099=DIRECTION('',(0.,-1.,0.));
#26100=DIRECTION('center_axis',(0.,-1.,0.));
#26101=DIRECTION('ref_axis',(-1.,0.,2.36700689860723E-12));
#26102=DIRECTION('',(0.,-1.,0.));
#26103=DIRECTION('center_axis',(0.,-1.,0.));
#26104=DIRECTION('ref_axis',(-1.,0.,2.36700689860723E-12));
#26105=DIRECTION('',(0.,-1.,0.));
#26106=DIRECTION('center_axis',(0.,-1.,0.));
#26107=DIRECTION('ref_axis',(-1.,0.,2.36700689860723E-12));
#26108=DIRECTION('',(0.,-1.,0.));
#26109=DIRECTION('center_axis',(0.,-1.,0.));
#26110=DIRECTION('ref_axis',(-1.,0.,2.36700689860723E-12));
#26111=DIRECTION('',(0.,-1.,0.));
#26112=DIRECTION('center_axis',(0.,-1.,0.));
#26113=DIRECTION('ref_axis',(-1.,0.,2.36700689860723E-12));
#26114=DIRECTION('',(0.,-1.,0.));
#26115=DIRECTION('center_axis',(0.,-1.,0.));
#26116=DIRECTION('ref_axis',(-1.,0.,2.36700689860723E-12));
#26117=DIRECTION('',(0.,-1.,0.));
#26118=DIRECTION('center_axis',(0.,-1.,0.));
#26119=DIRECTION('ref_axis',(-1.,0.,2.36700689860723E-12));
#26120=DIRECTION('',(0.,-1.,0.));
#26121=DIRECTION('center_axis',(0.,-1.,0.));
#26122=DIRECTION('ref_axis',(-1.,0.,2.36700689860723E-12));
#26123=DIRECTION('',(0.,-1.,0.));
#26124=DIRECTION('center_axis',(0.,-1.,0.));
#26125=DIRECTION('ref_axis',(-1.,0.,2.36700689860723E-12));
#26126=DIRECTION('',(0.,-1.,0.));
#26127=DIRECTION('center_axis',(0.,-1.,0.));
#26128=DIRECTION('ref_axis',(-1.,0.,2.36700689860723E-12));
#26129=DIRECTION('',(0.,-1.,0.));
#26130=DIRECTION('center_axis',(0.,-1.,0.));
#26131=DIRECTION('ref_axis',(-1.,0.,2.36700689860723E-12));
#26132=DIRECTION('',(0.,-1.,0.));
#26133=DIRECTION('center_axis',(0.,-1.,0.));
#26134=DIRECTION('ref_axis',(-1.,0.,2.36700689860723E-12));
#26135=DIRECTION('',(0.,-1.,0.));
#26136=DIRECTION('center_axis',(0.,-1.,0.));
#26137=DIRECTION('ref_axis',(-1.,0.,2.36700689860723E-12));
#26138=DIRECTION('',(0.,-1.,0.));
#26139=DIRECTION('center_axis',(0.,-1.,0.));
#26140=DIRECTION('ref_axis',(-1.,0.,2.36700689860723E-12));
#26141=DIRECTION('',(0.,-1.,0.));
#26142=DIRECTION('center_axis',(0.,-1.,0.));
#26143=DIRECTION('ref_axis',(-1.,0.,2.36700689860723E-12));
#26144=DIRECTION('',(0.,-1.,0.));
#26145=DIRECTION('center_axis',(0.,-1.,0.));
#26146=DIRECTION('ref_axis',(-1.,0.,2.36700689860723E-12));
#26147=DIRECTION('',(0.,-1.,0.));
#26148=DIRECTION('center_axis',(0.,-1.,0.));
#26149=DIRECTION('ref_axis',(-1.,0.,2.36700689860723E-12));
#26150=DIRECTION('',(0.,-1.,0.));
#26151=DIRECTION('center_axis',(0.,-1.,0.));
#26152=DIRECTION('ref_axis',(-1.,0.,2.36700689860723E-12));
#26153=DIRECTION('',(0.,-1.,0.));
#26154=DIRECTION('center_axis',(0.,-1.,0.));
#26155=DIRECTION('ref_axis',(-1.,0.,2.36700689860723E-12));
#26156=DIRECTION('',(0.,-1.,0.));
#26157=DIRECTION('center_axis',(0.,-1.,0.));
#26158=DIRECTION('ref_axis',(-1.,0.,2.36700689860723E-12));
#26159=DIRECTION('',(0.,-1.,0.));
#26160=DIRECTION('center_axis',(0.,-1.,0.));
#26161=DIRECTION('ref_axis',(-1.,0.,2.36700689860723E-12));
#26162=DIRECTION('',(0.,-1.,0.));
#26163=DIRECTION('center_axis',(0.,-1.,0.));
#26164=DIRECTION('ref_axis',(-1.,0.,2.36700689860723E-12));
#26165=DIRECTION('',(0.,-1.,0.));
#26166=DIRECTION('center_axis',(0.,-1.,0.));
#26167=DIRECTION('ref_axis',(-1.,0.,2.36700689860723E-12));
#26168=DIRECTION('',(0.,-1.,0.));
#26169=DIRECTION('center_axis',(0.,-1.,0.));
#26170=DIRECTION('ref_axis',(-1.,0.,2.36700689860723E-12));
#26171=DIRECTION('',(0.,-1.,0.));
#26172=DIRECTION('center_axis',(0.,-1.,0.));
#26173=DIRECTION('ref_axis',(-1.,0.,2.36700689860723E-12));
#26174=DIRECTION('',(0.,-1.,0.));
#26175=DIRECTION('center_axis',(0.,-1.,0.));
#26176=DIRECTION('ref_axis',(-1.,0.,2.36700689860723E-12));
#26177=DIRECTION('',(0.,-1.,0.));
#26178=DIRECTION('center_axis',(0.,-1.,0.));
#26179=DIRECTION('ref_axis',(-1.,0.,2.36700689860723E-12));
#26180=DIRECTION('',(0.,-1.,0.));
#26181=DIRECTION('center_axis',(0.,-1.,0.));
#26182=DIRECTION('ref_axis',(-1.,0.,2.36700689860723E-12));
#26183=DIRECTION('',(0.,-1.,0.));
#26184=DIRECTION('center_axis',(0.,-1.,0.));
#26185=DIRECTION('ref_axis',(-1.,0.,2.36700689860723E-12));
#26186=DIRECTION('',(0.,-1.,0.));
#26187=DIRECTION('center_axis',(0.,-1.,0.));
#26188=DIRECTION('ref_axis',(-1.,0.,2.36700689860723E-12));
#26189=DIRECTION('',(0.,-1.,0.));
#26190=DIRECTION('center_axis',(0.,-1.,0.));
#26191=DIRECTION('ref_axis',(-1.,0.,2.36700689860723E-12));
#26192=DIRECTION('',(0.,-1.,0.));
#26193=DIRECTION('center_axis',(0.,-1.,0.));
#26194=DIRECTION('ref_axis',(-1.,0.,2.36700689860723E-12));
#26195=DIRECTION('',(0.,-1.,0.));
#26196=DIRECTION('center_axis',(0.,-1.,0.));
#26197=DIRECTION('ref_axis',(-1.,0.,2.36700689860723E-12));
#26198=DIRECTION('',(0.,-1.,0.));
#26199=DIRECTION('center_axis',(0.,-1.,0.));
#26200=DIRECTION('ref_axis',(-1.,0.,2.36700689860723E-12));
#26201=DIRECTION('',(0.,-1.,0.));
#26202=DIRECTION('center_axis',(0.,-1.,0.));
#26203=DIRECTION('ref_axis',(-1.,0.,2.36700689860723E-12));
#26204=DIRECTION('',(0.,-1.,0.));
#26205=DIRECTION('center_axis',(0.,-1.,0.));
#26206=DIRECTION('ref_axis',(-1.,0.,2.36700689860723E-12));
#26207=DIRECTION('',(0.,-1.,0.));
#26208=DIRECTION('center_axis',(0.,-1.,0.));
#26209=DIRECTION('ref_axis',(-1.,0.,2.36700689860723E-12));
#26210=DIRECTION('',(0.,-1.,0.));
#26211=DIRECTION('center_axis',(0.,-1.,0.));
#26212=DIRECTION('ref_axis',(-1.,0.,2.36700689860723E-12));
#26213=DIRECTION('',(0.,-1.,0.));
#26214=DIRECTION('center_axis',(0.,-1.,0.));
#26215=DIRECTION('ref_axis',(-1.,0.,2.36700689860723E-12));
#26216=DIRECTION('',(0.,-1.,0.));
#26217=DIRECTION('center_axis',(0.,-1.,0.));
#26218=DIRECTION('ref_axis',(-1.,0.,2.36700689860723E-12));
#26219=DIRECTION('',(0.,-1.,0.));
#26220=DIRECTION('center_axis',(0.,-1.,0.));
#26221=DIRECTION('ref_axis',(-1.,0.,2.36700689860723E-12));
#26222=DIRECTION('',(0.,-1.,0.));
#26223=DIRECTION('center_axis',(0.,-1.,0.));
#26224=DIRECTION('ref_axis',(-1.,0.,2.36700689860723E-12));
#26225=DIRECTION('',(0.,-1.,0.));
#26226=DIRECTION('center_axis',(0.,-1.,0.));
#26227=DIRECTION('ref_axis',(-1.,0.,2.36700689860723E-12));
#26228=DIRECTION('',(0.,-1.,0.));
#26229=DIRECTION('center_axis',(0.,-1.,0.));
#26230=DIRECTION('ref_axis',(-1.,0.,2.36700689860723E-12));
#26231=DIRECTION('',(0.,-1.,0.));
#26232=DIRECTION('center_axis',(0.,-1.,0.));
#26233=DIRECTION('ref_axis',(-1.,0.,2.36700689860723E-12));
#26234=DIRECTION('',(0.,-1.,0.));
#26235=DIRECTION('center_axis',(0.,-1.,0.));
#26236=DIRECTION('ref_axis',(-1.,0.,2.36700689860723E-12));
#26237=DIRECTION('',(0.,-1.,0.));
#26238=DIRECTION('center_axis',(0.,-1.,0.));
#26239=DIRECTION('ref_axis',(-1.,0.,2.36700689860723E-12));
#26240=DIRECTION('',(0.,-1.,0.));
#26241=DIRECTION('center_axis',(0.,-1.,0.));
#26242=DIRECTION('ref_axis',(-1.,0.,2.36700689860723E-12));
#26243=DIRECTION('',(0.,-1.,0.));
#26244=DIRECTION('center_axis',(0.,-1.,0.));
#26245=DIRECTION('ref_axis',(-1.,0.,2.36700689860723E-12));
#26246=DIRECTION('',(0.,-1.,0.));
#26247=DIRECTION('center_axis',(0.,-1.,0.));
#26248=DIRECTION('ref_axis',(-1.,0.,2.36700689860723E-12));
#26249=DIRECTION('',(0.,-1.,0.));
#26250=DIRECTION('center_axis',(0.,-1.,0.));
#26251=DIRECTION('ref_axis',(-1.,0.,2.36700689860723E-12));
#26252=DIRECTION('',(0.,-1.,0.));
#26253=DIRECTION('center_axis',(0.,-1.,0.));
#26254=DIRECTION('ref_axis',(-1.,0.,2.36700689860723E-12));
#26255=DIRECTION('',(0.,-1.,0.));
#26256=DIRECTION('center_axis',(0.,-1.,0.));
#26257=DIRECTION('ref_axis',(-1.,0.,2.36700689860723E-12));
#26258=DIRECTION('',(0.,-1.,0.));
#26259=DIRECTION('center_axis',(0.,-1.,0.));
#26260=DIRECTION('ref_axis',(-1.,0.,2.36700689860723E-12));
#26261=DIRECTION('',(0.,-1.,0.));
#26262=DIRECTION('center_axis',(0.,-1.,0.));
#26263=DIRECTION('ref_axis',(-1.,0.,2.36700689860723E-12));
#26264=DIRECTION('',(0.,-1.,0.));
#26265=DIRECTION('center_axis',(0.,-1.,0.));
#26266=DIRECTION('ref_axis',(-1.,0.,2.36700689860723E-12));
#26267=DIRECTION('',(0.,-1.,0.));
#26268=DIRECTION('center_axis',(0.,-1.,0.));
#26269=DIRECTION('ref_axis',(-1.,0.,2.36700689860723E-12));
#26270=DIRECTION('',(0.,-1.,0.));
#26271=DIRECTION('center_axis',(0.,-1.,0.));
#26272=DIRECTION('ref_axis',(-1.,0.,2.36700689860723E-12));
#26273=DIRECTION('',(0.,-1.,0.));
#26274=DIRECTION('center_axis',(0.,-1.,0.));
#26275=DIRECTION('ref_axis',(-1.,0.,2.36700689860723E-12));
#26276=DIRECTION('',(0.,-1.,0.));
#26277=DIRECTION('center_axis',(0.,-1.,0.));
#26278=DIRECTION('ref_axis',(-1.,0.,2.36700689860723E-12));
#26279=DIRECTION('',(0.,-1.,0.));
#26280=DIRECTION('center_axis',(0.,-1.,0.));
#26281=DIRECTION('ref_axis',(-1.,0.,2.36700689860723E-12));
#26282=DIRECTION('',(0.,-1.,0.));
#26283=DIRECTION('center_axis',(0.,-1.,0.));
#26284=DIRECTION('ref_axis',(-1.,0.,2.36700689860723E-12));
#26285=DIRECTION('',(0.,-1.,0.));
#26286=DIRECTION('center_axis',(0.,-1.,0.));
#26287=DIRECTION('ref_axis',(-1.,0.,2.36700689860723E-12));
#26288=DIRECTION('',(0.,-1.,0.));
#26289=DIRECTION('center_axis',(0.,-1.,0.));
#26290=DIRECTION('ref_axis',(-1.,0.,2.36700689860723E-12));
#26291=DIRECTION('',(0.,-1.,0.));
#26292=DIRECTION('center_axis',(0.,-1.,0.));
#26293=DIRECTION('ref_axis',(-1.,0.,2.36700689860723E-12));
#26294=DIRECTION('',(0.,-1.,0.));
#26295=DIRECTION('center_axis',(0.,-1.,0.));
#26296=DIRECTION('ref_axis',(-1.,0.,2.36700689860723E-12));
#26297=DIRECTION('',(0.,-1.,0.));
#26298=DIRECTION('center_axis',(0.,-1.,0.));
#26299=DIRECTION('ref_axis',(-1.,0.,2.36700689860723E-12));
#26300=DIRECTION('',(0.,-1.,0.));
#26301=DIRECTION('center_axis',(0.,-1.,0.));
#26302=DIRECTION('ref_axis',(-1.,0.,2.36700689860723E-12));
#26303=DIRECTION('',(0.,-1.,0.));
#26304=DIRECTION('center_axis',(0.,-1.,0.));
#26305=DIRECTION('ref_axis',(-1.,0.,2.36700689860723E-12));
#26306=DIRECTION('',(0.,-1.,0.));
#26307=DIRECTION('center_axis',(0.,-1.,0.));
#26308=DIRECTION('ref_axis',(-1.,0.,2.36700689860723E-12));
#26309=DIRECTION('',(0.,-1.,0.));
#26310=DIRECTION('center_axis',(0.,-1.,0.));
#26311=DIRECTION('ref_axis',(-1.,0.,2.36700689860723E-12));
#26312=DIRECTION('',(0.,-1.,0.));
#26313=DIRECTION('center_axis',(0.,-1.,0.));
#26314=DIRECTION('ref_axis',(-1.,0.,2.36700689860723E-12));
#26315=DIRECTION('',(0.,-1.,0.));
#26316=DIRECTION('center_axis',(0.,-1.,0.));
#26317=DIRECTION('ref_axis',(-1.,0.,2.36700689860723E-12));
#26318=DIRECTION('',(0.,-1.,0.));
#26319=DIRECTION('center_axis',(0.,-1.,0.));
#26320=DIRECTION('ref_axis',(-1.,0.,2.36700689860723E-12));
#26321=DIRECTION('',(0.,-1.,0.));
#26322=DIRECTION('center_axis',(0.,-1.,0.));
#26323=DIRECTION('ref_axis',(-1.,0.,2.36700689860723E-12));
#26324=DIRECTION('',(0.,-1.,0.));
#26325=DIRECTION('center_axis',(0.,-1.,0.));
#26326=DIRECTION('ref_axis',(-1.,0.,2.36700689860723E-12));
#26327=DIRECTION('',(0.,-1.,0.));
#26328=DIRECTION('center_axis',(0.,-1.,0.));
#26329=DIRECTION('ref_axis',(-1.,0.,2.36700689860723E-12));
#26330=DIRECTION('',(0.,-1.,0.));
#26331=DIRECTION('center_axis',(0.,-1.,0.));
#26332=DIRECTION('ref_axis',(-1.,0.,2.36700689860723E-12));
#26333=DIRECTION('',(0.,-1.,0.));
#26334=DIRECTION('center_axis',(0.,-1.,0.));
#26335=DIRECTION('ref_axis',(-1.,0.,2.36700689860723E-12));
#26336=DIRECTION('',(0.,-1.,0.));
#26337=DIRECTION('center_axis',(0.,-1.,0.));
#26338=DIRECTION('ref_axis',(-1.,0.,2.36700689860723E-12));
#26339=DIRECTION('',(0.,-1.,0.));
#26340=DIRECTION('center_axis',(0.,-1.,0.));
#26341=DIRECTION('ref_axis',(-1.,0.,2.36700689860723E-12));
#26342=DIRECTION('',(0.,-1.,0.));
#26343=DIRECTION('center_axis',(0.,-1.,0.));
#26344=DIRECTION('ref_axis',(1.,0.,0.));
#26345=DIRECTION('center_axis',(0.,1.,0.));
#26346=DIRECTION('ref_axis',(1.,0.,0.));
#26347=DIRECTION('',(0.707106781186541,0.707106781186554,8.65956056235486E-17));
#26348=DIRECTION('center_axis',(0.,-1.,0.));
#26349=DIRECTION('ref_axis',(1.,0.,0.));
#26350=DIRECTION('center_axis',(0.,1.,0.));
#26351=DIRECTION('ref_axis',(1.,0.,0.));
#26352=DIRECTION('',(0.,-1.,0.));
#26353=DIRECTION('center_axis',(0.,1.,0.));
#26354=DIRECTION('ref_axis',(1.,0.,0.));
#26355=DIRECTION('center_axis',(0.,1.,0.));
#26356=DIRECTION('ref_axis',(1.,0.,0.));
#26357=DIRECTION('center_axis',(0.,1.,0.));
#26358=DIRECTION('ref_axis',(-1.,0.,0.));
#26359=DIRECTION('center_axis',(0.,1.,0.));
#26360=DIRECTION('ref_axis',(-1.,0.,0.));
#26361=DIRECTION('',(0.707106781186546,0.707106781186549,8.65956056235492E-17));
#26362=DIRECTION('center_axis',(0.,-1.,0.));
#26363=DIRECTION('ref_axis',(-1.,0.,0.));
#26364=DIRECTION('center_axis',(0.,1.,0.));
#26365=DIRECTION('ref_axis',(-1.,0.,0.));
#26366=DIRECTION('',(0.,1.,0.));
#26367=DIRECTION('center_axis',(0.,-1.,0.));
#26368=DIRECTION('ref_axis',(-1.,0.,0.));
#26369=DIRECTION('center_axis',(0.,-1.,0.));
#26370=DIRECTION('ref_axis',(-1.,0.,0.));
#26371=DIRECTION('center_axis',(0.,-1.,0.));
#26372=DIRECTION('ref_axis',(-1.,0.,0.));
#26373=DIRECTION('center_axis',(0.,1.,0.));
#26374=DIRECTION('ref_axis',(-1.,0.,0.));
#26375=DIRECTION('center_axis',(0.,-1.,0.));
#26376=DIRECTION('ref_axis',(-0.9659062825861,0.,-0.258891972182802));
#26377=DIRECTION('center_axis',(0.,1.,0.));
#26378=DIRECTION('ref_axis',(-1.,0.,2.36700689860723E-12));
#26379=DIRECTION('center_axis',(0.,1.,0.));
#26380=DIRECTION('ref_axis',(0.,0.,1.));
#26381=DIRECTION('center_axis',(0.,-1.,0.));
#26382=DIRECTION('ref_axis',(1.,0.,0.));
#26383=DIRECTION('center_axis',(0.,1.,0.));
#26384=DIRECTION('ref_axis',(0.,0.,1.));
#26385=DIRECTION('center_axis',(0.,-1.,0.));
#26386=DIRECTION('ref_axis',(1.,0.,-6.50117889680365E-14));
#26387=DIRECTION('center_axis',(0.,1.,0.));
#26388=DIRECTION('ref_axis',(-0.644123759008342,0.,-0.764921292082371));
#26389=DIRECTION('center_axis',(0.,1.,0.));
#26390=DIRECTION('ref_axis',(-0.0923927080499103,0.,0.995722645870427));
#26391=DIRECTION('center_axis',(0.,1.,0.));
#26392=DIRECTION('ref_axis',(1.,0.,0.));
#26393=DIRECTION('center_axis',(0.,-1.,0.));
#26394=DIRECTION('ref_axis',(-1.,0.,0.));
#26395=DIRECTION('axis',(0.,0.,1.));
#26396=DIRECTION('refdir',(1.,0.,0.));
#26397=DIRECTION('center_axis',(0.,1.,0.));
#26398=DIRECTION('ref_axis',(1.,0.,0.));
#26399=DIRECTION('center_axis',(0.,-1.,0.));
#26400=DIRECTION('ref_axis',(0.707106781186547,0.,-0.707106781186547));
#26401=DIRECTION('',(1.,0.,0.));
#26402=DIRECTION('center_axis',(0.,-1.,0.));
#26403=DIRECTION('ref_axis',(-0.707106781186547,0.,-0.707106781186547));
#26404=DIRECTION('',(0.,0.,-1.));
#26405=DIRECTION('',(-1.,0.,0.));
#26406=DIRECTION('',(0.,0.,-1.));
#26407=DIRECTION('center_axis',(0.,-1.,0.));
#26408=DIRECTION('ref_axis',(1.,0.,0.));
#26409=DIRECTION('center_axis',(0.,0.,-1.));
#26410=DIRECTION('ref_axis',(-1.,0.,0.));
#26411=DIRECTION('center_axis',(0.,0.,-1.));
#26412=DIRECTION('ref_axis',(-1.,0.,0.));
#26413=DIRECTION('',(0.,0.,-1.));
#26414=DIRECTION('center_axis',(0.,0.,1.));
#26415=DIRECTION('ref_axis',(-1.,0.,0.));
#26416=DIRECTION('center_axis',(0.,0.,-1.));
#26417=DIRECTION('ref_axis',(-1.,0.,0.));
#26418=DIRECTION('center_axis',(0.,0.,-1.));
#26419=DIRECTION('ref_axis',(-1.,0.,0.));
#26420=DIRECTION('',(0.,0.,-1.));
#26421=DIRECTION('center_axis',(0.,0.,1.));
#26422=DIRECTION('ref_axis',(-1.,0.,0.));
#26423=DIRECTION('center_axis',(0.,0.,-1.));
#26424=DIRECTION('ref_axis',(-1.,0.,0.));
#26425=DIRECTION('center_axis',(0.,0.,-1.));
#26426=DIRECTION('ref_axis',(-1.,0.,0.));
#26427=DIRECTION('',(0.,0.,-1.));
#26428=DIRECTION('center_axis',(0.,0.,1.));
#26429=DIRECTION('ref_axis',(-1.,0.,0.));
#26430=DIRECTION('center_axis',(0.,0.,-1.));
#26431=DIRECTION('ref_axis',(-1.,0.,0.));
#26432=DIRECTION('center_axis',(0.,0.,-1.));
#26433=DIRECTION('ref_axis',(-1.,0.,0.));
#26434=DIRECTION('',(0.,0.,-1.));
#26435=DIRECTION('center_axis',(0.,0.,1.));
#26436=DIRECTION('ref_axis',(-1.,0.,0.));
#26437=DIRECTION('center_axis',(0.,0.,-1.));
#26438=DIRECTION('ref_axis',(-1.,0.,0.));
#26439=DIRECTION('center_axis',(0.,0.,-1.));
#26440=DIRECTION('ref_axis',(-1.,0.,0.));
#26441=DIRECTION('',(0.,0.,-1.));
#26442=DIRECTION('center_axis',(0.,0.,1.));
#26443=DIRECTION('ref_axis',(-1.,0.,0.));
#26444=DIRECTION('center_axis',(0.,0.,-1.));
#26445=DIRECTION('ref_axis',(-1.,0.,0.));
#26446=DIRECTION('center_axis',(0.,0.,-1.));
#26447=DIRECTION('ref_axis',(-1.,0.,0.));
#26448=DIRECTION('',(0.,0.,-1.));
#26449=DIRECTION('center_axis',(0.,0.,1.));
#26450=DIRECTION('ref_axis',(-1.,0.,0.));
#26451=DIRECTION('center_axis',(0.,0.,-1.));
#26452=DIRECTION('ref_axis',(-1.,0.,0.));
#26453=DIRECTION('center_axis',(0.,0.,-1.));
#26454=DIRECTION('ref_axis',(-1.,0.,0.));
#26455=DIRECTION('',(0.,0.,-1.));
#26456=DIRECTION('center_axis',(0.,0.,1.));
#26457=DIRECTION('ref_axis',(-1.,0.,0.));
#26458=DIRECTION('center_axis',(0.,0.,-1.));
#26459=DIRECTION('ref_axis',(-1.,0.,0.));
#26460=DIRECTION('center_axis',(0.,0.,-1.));
#26461=DIRECTION('ref_axis',(-1.,0.,0.));
#26462=DIRECTION('',(0.,0.,-1.));
#26463=DIRECTION('center_axis',(0.,0.,1.));
#26464=DIRECTION('ref_axis',(-1.,0.,0.));
#26465=DIRECTION('center_axis',(0.,0.,-1.));
#26466=DIRECTION('ref_axis',(-1.,0.,0.));
#26467=DIRECTION('center_axis',(0.,0.,-1.));
#26468=DIRECTION('ref_axis',(-1.,0.,0.));
#26469=DIRECTION('',(0.,0.,-1.));
#26470=DIRECTION('center_axis',(0.,0.,1.));
#26471=DIRECTION('ref_axis',(-1.,0.,0.));
#26472=DIRECTION('center_axis',(0.,0.,-1.));
#26473=DIRECTION('ref_axis',(-1.,0.,0.));
#26474=DIRECTION('center_axis',(0.,0.,-1.));
#26475=DIRECTION('ref_axis',(-1.,0.,0.));
#26476=DIRECTION('',(0.,0.,-1.));
#26477=DIRECTION('center_axis',(0.,0.,1.));
#26478=DIRECTION('ref_axis',(-1.,0.,0.));
#26479=DIRECTION('center_axis',(0.,0.,-1.));
#26480=DIRECTION('ref_axis',(-1.,0.,0.));
#26481=DIRECTION('center_axis',(0.,0.,-1.));
#26482=DIRECTION('ref_axis',(-1.,0.,0.));
#26483=DIRECTION('',(0.,0.,-1.));
#26484=DIRECTION('center_axis',(0.,0.,1.));
#26485=DIRECTION('ref_axis',(-1.,0.,0.));
#26486=DIRECTION('center_axis',(0.,0.,-1.));
#26487=DIRECTION('ref_axis',(-1.,0.,0.));
#26488=DIRECTION('center_axis',(0.,0.,-1.));
#26489=DIRECTION('ref_axis',(-1.,0.,0.));
#26490=DIRECTION('',(0.,0.,-1.));
#26491=DIRECTION('center_axis',(0.,0.,1.));
#26492=DIRECTION('ref_axis',(-1.,0.,0.));
#26493=DIRECTION('center_axis',(0.,0.,-1.));
#26494=DIRECTION('ref_axis',(-1.,0.,0.));
#26495=DIRECTION('center_axis',(0.,0.,-1.));
#26496=DIRECTION('ref_axis',(-1.,0.,0.));
#26497=DIRECTION('',(0.,0.,-1.));
#26498=DIRECTION('center_axis',(0.,0.,1.));
#26499=DIRECTION('ref_axis',(-1.,0.,0.));
#26500=DIRECTION('center_axis',(0.,0.,-1.));
#26501=DIRECTION('ref_axis',(-1.,0.,0.));
#26502=DIRECTION('center_axis',(0.,0.,-1.));
#26503=DIRECTION('ref_axis',(-1.,0.,0.));
#26504=DIRECTION('',(0.,0.,-1.));
#26505=DIRECTION('center_axis',(0.,0.,1.));
#26506=DIRECTION('ref_axis',(-1.,0.,0.));
#26507=DIRECTION('center_axis',(0.,0.,-1.));
#26508=DIRECTION('ref_axis',(-1.,0.,0.));
#26509=DIRECTION('center_axis',(0.,0.,-1.));
#26510=DIRECTION('ref_axis',(-1.,0.,0.));
#26511=DIRECTION('',(0.,0.,-1.));
#26512=DIRECTION('center_axis',(0.,0.,1.));
#26513=DIRECTION('ref_axis',(-1.,0.,0.));
#26514=DIRECTION('center_axis',(0.,0.,-1.));
#26515=DIRECTION('ref_axis',(-1.,0.,0.));
#26516=DIRECTION('center_axis',(0.,0.,-1.));
#26517=DIRECTION('ref_axis',(-1.,0.,0.));
#26518=DIRECTION('',(0.,0.,-1.));
#26519=DIRECTION('center_axis',(0.,0.,1.));
#26520=DIRECTION('ref_axis',(-1.,0.,0.));
#26521=DIRECTION('center_axis',(0.,1.,0.));
#26522=DIRECTION('ref_axis',(1.,0.,0.));
#26523=DIRECTION('center_axis',(0.,1.,0.));
#26524=DIRECTION('ref_axis',(1.,0.,0.));
#26525=DIRECTION('',(1.22464679914735E-16,1.,-1.49975978266186E-32));
#26526=DIRECTION('center_axis',(0.,-1.,0.));
#26527=DIRECTION('ref_axis',(0.707106781186547,0.,-0.707106781186547));
#26528=DIRECTION('center_axis',(0.,1.,0.));
#26529=DIRECTION('ref_axis',(0.707106781186547,0.,-0.707106781186547));
#26530=DIRECTION('',(0.,1.,0.));
#26531=DIRECTION('',(0.,-1.,0.));
#26532=DIRECTION('center_axis',(0.,0.,-1.));
#26533=DIRECTION('ref_axis',(-1.,0.,0.));
#26534=DIRECTION('',(-1.,0.,0.));
#26535=DIRECTION('',(0.,-1.,0.));
#26536=DIRECTION('center_axis',(0.,1.,0.));
#26537=DIRECTION('ref_axis',(-0.707106781186547,0.,-0.707106781186547));
#26538=DIRECTION('center_axis',(0.,1.,0.));
#26539=DIRECTION('ref_axis',(-0.707106781186547,0.,-0.707106781186547));
#26540=DIRECTION('',(0.,1.,0.));
#26541=DIRECTION('center_axis',(-1.,0.,0.));
#26542=DIRECTION('ref_axis',(0.,1.,0.));
#26543=DIRECTION('',(0.,0.,-1.));
#26544=DIRECTION('',(0.,-1.,0.));
#26545=DIRECTION('center_axis',(0.,-1.,0.));
#26546=DIRECTION('ref_axis',(-1.,0.,0.));
#26547=DIRECTION('',(0.,0.,-1.));
#26548=DIRECTION('',(1.,0.,0.));
#26549=DIRECTION('center_axis',(1.,0.,0.));
#26550=DIRECTION('ref_axis',(0.,-1.,0.));
#26551=DIRECTION('',(0.,1.,0.));
#26552=DIRECTION('center_axis',(1.,0.,0.));
#26553=DIRECTION('ref_axis',(0.,0.,-1.));
#26554=DIRECTION('',(0.,0.,-1.));
#26555=DIRECTION('',(0.,1.,0.));
#26556=DIRECTION('',(0.,0.,1.));
#26557=DIRECTION('',(0.,1.,0.));
#26558=DIRECTION('center_axis',(0.,0.,1.));
#26559=DIRECTION('ref_axis',(1.,0.,0.));
#26560=DIRECTION('',(1.,0.,0.));
#26561=DIRECTION('',(0.,1.,0.));
#26562=DIRECTION('',(-1.,0.,0.));
#26563=DIRECTION('center_axis',(-1.,0.,0.));
#26564=DIRECTION('ref_axis',(0.,0.,1.));
#26565=DIRECTION('',(0.,0.,1.));
#26566=DIRECTION('',(0.,-1.,0.));
#26567=DIRECTION('',(0.,0.,-1.));
#26568=DIRECTION('center_axis',(0.,0.,1.));
#26569=DIRECTION('ref_axis',(1.,0.,0.));
#26570=DIRECTION('',(-1.,0.,0.));
#26571=DIRECTION('',(0.,1.,0.));
#26572=DIRECTION('',(1.,0.,0.));
#26573=DIRECTION('center_axis',(0.,0.,1.));
#26574=DIRECTION('ref_axis',(1.,0.,0.));
#26575=DIRECTION('',(1.,0.,0.));
#26576=DIRECTION('',(0.,-1.,0.));
#26577=DIRECTION('',(-1.,0.,0.));
#26578=DIRECTION('center_axis',(0.,-1.,0.));
#26579=DIRECTION('ref_axis',(1.,0.,0.));
#26580=DIRECTION('',(0.,0.,1.));
#26581=DIRECTION('',(1.,0.,0.));
#26582=DIRECTION('',(0.,0.,1.));
#26583=DIRECTION('center_axis',(0.,1.,0.));
#26584=DIRECTION('ref_axis',(-1.,0.,0.));
#26585=DIRECTION('',(0.,0.,1.));
#26586=DIRECTION('',(-1.,0.,0.));
#26587=DIRECTION('',(0.,0.,1.));
#26588=DIRECTION('center_axis',(1.,0.,0.));
#26589=DIRECTION('ref_axis',(0.,1.,0.));
#26590=DIRECTION('',(0.,1.,0.));
#26591=DIRECTION('center_axis',(-1.,0.,0.));
#26592=DIRECTION('ref_axis',(0.,-1.,0.));
#26593=DIRECTION('',(0.,-1.,0.));
#26594=DIRECTION('center_axis',(0.,0.,1.));
#26595=DIRECTION('ref_axis',(1.,0.,0.));
#26596=DIRECTION('axis',(0.,0.,1.));
#26597=DIRECTION('refdir',(1.,0.,0.));
#26598=DIRECTION('center_axis',(0.710729249896214,0.,0.703465658964221));
#26599=DIRECTION('ref_axis',(-0.703465658964221,0.,0.710729249896214));
#26600=DIRECTION('',(0.,1.,0.));
#26601=DIRECTION('',(-0.703465658964221,0.,0.710729249896214));
#26602=DIRECTION('',(0.,-1.,0.));
#26603=DIRECTION('',(0.703465658964221,0.,-0.710729249896214));
#26604=DIRECTION('center_axis',(0.,-1.,0.));
#26605=DIRECTION('ref_axis',(0.963381374692954,0.,0.268134904282738));
#26606=DIRECTION('center_axis',(0.,-1.,0.));
#26607=DIRECTION('ref_axis',(0.963381374692954,0.,0.268134904282738));
#26608=DIRECTION('',(0.,-1.,0.));
#26609=DIRECTION('center_axis',(0.,1.,0.));
#26610=DIRECTION('ref_axis',(0.963381374692954,0.,0.268134904282738));
#26611=DIRECTION('center_axis',(0.,-1.,0.));
#26612=DIRECTION('ref_axis',(-0.963381374692978,0.,-0.268134904282653));
#26613=DIRECTION('center_axis',(0.,1.,0.));
#26614=DIRECTION('ref_axis',(-0.963381374692978,0.,-0.268134904282653));
#26615=DIRECTION('',(0.,-1.,0.));
#26616=DIRECTION('center_axis',(0.,-1.,0.));
#26617=DIRECTION('ref_axis',(-0.963381374692978,0.,-0.268134904282653));
#26618=DIRECTION('center_axis',(0.,-1.,0.));
#26619=DIRECTION('ref_axis',(1.,0.,-2.53764096072769E-16));
#26620=DIRECTION('center_axis',(0.,-1.,0.));
#26621=DIRECTION('ref_axis',(1.,0.,-2.53764096072769E-16));
#26622=DIRECTION('',(0.,-1.,0.));
#26623=DIRECTION('center_axis',(0.,1.,0.));
#26624=DIRECTION('ref_axis',(1.,0.,-2.53764096072769E-16));
#26625=DIRECTION('center_axis',(1.,0.,-2.53764096072769E-16));
#26626=DIRECTION('ref_axis',(2.53764096072769E-16,0.,1.));
#26627=DIRECTION('',(2.53764096072769E-16,0.,1.));
#26628=DIRECTION('',(0.,-1.,0.));
#26629=DIRECTION('',(-2.53764096072769E-16,0.,-1.));
#26630=DIRECTION('center_axis',(0.,-1.,0.));
#26631=DIRECTION('ref_axis',(0.245760053518537,0.,-0.969330694909929));
#26632=DIRECTION('center_axis',(0.,-1.,0.));
#26633=DIRECTION('ref_axis',(0.245760053518537,0.,-0.969330694909929));
#26634=DIRECTION('',(0.,-1.,0.));
#26635=DIRECTION('center_axis',(0.,1.,0.));
#26636=DIRECTION('ref_axis',(0.245760053518537,0.,-0.969330694909929));
#26637=DIRECTION('center_axis',(0.,-1.,0.));
#26638=DIRECTION('ref_axis',(-0.245760053518569,0.,0.969330694909921));
#26639=DIRECTION('center_axis',(0.,1.,0.));
#26640=DIRECTION('ref_axis',(-0.245760053518569,0.,0.969330694909921));
#26641=DIRECTION('',(0.,-1.,0.));
#26642=DIRECTION('center_axis',(0.,-1.,0.));
#26643=DIRECTION('ref_axis',(-0.245760053518569,0.,0.969330694909921));
#26644=DIRECTION('center_axis',(0.,-1.,0.));
#26645=DIRECTION('ref_axis',(0.711979844231348,0.,-0.702199901316075));
#26646=DIRECTION('center_axis',(0.,-1.,0.));
#26647=DIRECTION('ref_axis',(0.711979844231348,0.,-0.702199901316075));
#26648=DIRECTION('',(0.,-1.,0.));
#26649=DIRECTION('center_axis',(0.,1.,0.));
#26650=DIRECTION('ref_axis',(0.711979844231348,0.,-0.702199901316075));
#26651=DIRECTION('center_axis',(0.71197984423134,0.,-0.702199901316083));
#26652=DIRECTION('ref_axis',(0.702199901316083,0.,0.71197984423134));
#26653=DIRECTION('',(0.702199901316083,0.,0.71197984423134));
#26654=DIRECTION('',(0.,-1.,0.));
#26655=DIRECTION('',(-0.702199901316083,0.,-0.71197984423134));
#26656=DIRECTION('center_axis',(0.,-1.,0.));
#26657=DIRECTION('ref_axis',(-0.711979844231334,0.,0.702199901316089));
#26658=DIRECTION('center_axis',(0.,1.,0.));
#26659=DIRECTION('ref_axis',(-0.711979844231334,0.,0.702199901316089));
#26660=DIRECTION('',(0.,-1.,0.));
#26661=DIRECTION('center_axis',(0.,-1.,0.));
#26662=DIRECTION('ref_axis',(-0.711979844231334,0.,0.702199901316089));
#26663=DIRECTION('center_axis',(1.,0.,-2.53764096072769E-16));
#26664=DIRECTION('ref_axis',(2.53764096072769E-16,0.,1.));
#26665=DIRECTION('',(2.53764096072769E-16,0.,1.));
#26666=DIRECTION('',(0.,-1.,0.));
#26667=DIRECTION('',(-2.53764096072769E-16,0.,-1.));
#26668=DIRECTION('center_axis',(0.,-1.,0.));
#26669=DIRECTION('ref_axis',(-1.,0.,1.71714482808377E-14));
#26670=DIRECTION('center_axis',(0.,1.,0.));
#26671=DIRECTION('ref_axis',(-1.,0.,1.71714482808377E-14));
#26672=DIRECTION('',(0.,-1.,0.));
#26673=DIRECTION('center_axis',(0.,-1.,0.));
#26674=DIRECTION('ref_axis',(-1.,0.,1.71714482808377E-14));
#26675=DIRECTION('center_axis',(0.709478283082607,0.,0.704727298913669));
#26676=DIRECTION('ref_axis',(-0.704727298913669,0.,0.709478283082607));
#26677=DIRECTION('',(-0.704727298913669,0.,0.709478283082607));
#26678=DIRECTION('',(0.,-1.,0.));
#26679=DIRECTION('',(0.704727298913669,0.,-0.709478283082607));
#26680=DIRECTION('center_axis',(0.,-1.,0.));
#26681=DIRECTION('ref_axis',(1.,0.,-4.29093873107336E-15));
#26682=DIRECTION('center_axis',(0.,-1.,0.));
#26683=DIRECTION('ref_axis',(1.,0.,-4.29093873107336E-15));
#26684=DIRECTION('',(0.,-1.,0.));
#26685=DIRECTION('center_axis',(0.,1.,0.));
#26686=DIRECTION('ref_axis',(1.,0.,-4.29093873107336E-15));
#26687=DIRECTION('center_axis',(1.,0.,-2.53764096072769E-16));
#26688=DIRECTION('ref_axis',(2.53764096072769E-16,0.,1.));
#26689=DIRECTION('',(2.53764096072769E-16,0.,1.));
#26690=DIRECTION('',(0.,-1.,0.));
#26691=DIRECTION('',(-2.53764096072769E-16,0.,-1.));
#26692=DIRECTION('center_axis',(0.707376432457449,0.,-0.706837027046385));
#26693=DIRECTION('ref_axis',(0.706837027046385,0.,0.707376432457449));
#26694=DIRECTION('',(0.706837027046385,0.,0.707376432457449));
#26695=DIRECTION('',(0.,-1.,0.));
#26696=DIRECTION('',(-0.706837027046385,0.,-0.707376432457449));
#26697=DIRECTION('center_axis',(0.,1.,0.));
#26698=DIRECTION('ref_axis',(1.,0.,0.));
#26699=DIRECTION('',(1.,0.,-2.53764096072769E-16));
#26700=DIRECTION('',(1.,0.,0.));
#26701=DIRECTION('',(0.706837027046385,0.,-0.707376432457449));
#26702=DIRECTION('',(0.,0.,-1.));
#26703=DIRECTION('center_axis',(0.,-1.,0.));
#26704=DIRECTION('ref_axis',(-1.,0.,-4.03717463500059E-15));
#26705=DIRECTION('',(-0.704727298913669,0.,-0.709478283082607));
#26706=DIRECTION('center_axis',(0.,1.,0.));
#26707=DIRECTION('ref_axis',(1.,0.,1.69176841847649E-14));
#26708=DIRECTION('',(0.,0.,-1.));
#26709=DIRECTION('center_axis',(0.,1.,0.));
#26710=DIRECTION('ref_axis',(0.711979844231334,0.,0.702199901316089));
#26711=DIRECTION('',(0.702199901316083,0.,-0.71197984423134));
#26712=DIRECTION('center_axis',(0.,-1.,0.));
#26713=DIRECTION('ref_axis',(-0.711979844231348,0.,-0.702199901316075));
#26714=DIRECTION('center_axis',(0.,1.,0.));
#26715=DIRECTION('ref_axis',(0.245760053518569,0.,0.969330694909921));
#26716=DIRECTION('center_axis',(0.,-1.,0.));
#26717=DIRECTION('ref_axis',(-0.245760053518537,0.,-0.969330694909929));
#26718=DIRECTION('',(0.,0.,-1.));
#26719=DIRECTION('center_axis',(0.,-1.,0.));
#26720=DIRECTION('ref_axis',(-1.,0.,0.));
#26721=DIRECTION('center_axis',(0.,1.,0.));
#26722=DIRECTION('ref_axis',(0.963381374692978,0.,-0.268134904282653));
#26723=DIRECTION('center_axis',(0.,-1.,0.));
#26724=DIRECTION('ref_axis',(-0.963381374692954,0.,0.268134904282739));
#26725=DIRECTION('',(-0.703465658964221,0.,-0.710729249896213));
#26726=DIRECTION('center_axis',(0.710729249896213,0.,-0.703465658964221));
#26727=DIRECTION('ref_axis',(0.703465658964221,0.,0.710729249896213));
#26728=DIRECTION('',(0.,1.,0.));
#26729=DIRECTION('',(0.,-1.,0.));
#26730=DIRECTION('',(0.703465658964221,0.,0.710729249896213));
#26731=DIRECTION('center_axis',(0.,1.,0.));
#26732=DIRECTION('ref_axis',(-0.963381374692954,0.,0.268134904282739));
#26733=DIRECTION('',(0.,-1.,0.));
#26734=DIRECTION('center_axis',(0.,1.,0.));
#26735=DIRECTION('ref_axis',(-0.963381374692954,0.,0.268134904282739));
#26736=DIRECTION('center_axis',(0.,1.,0.));
#26737=DIRECTION('ref_axis',(0.963381374692978,0.,-0.268134904282653));
#26738=DIRECTION('',(0.,-1.,0.));
#26739=DIRECTION('center_axis',(0.,-1.,0.));
#26740=DIRECTION('ref_axis',(0.963381374692978,0.,-0.268134904282653));
#26741=DIRECTION('center_axis',(0.,1.,0.));
#26742=DIRECTION('ref_axis',(-1.,0.,0.));
#26743=DIRECTION('',(0.,-1.,0.));
#26744=DIRECTION('center_axis',(0.,1.,0.));
#26745=DIRECTION('ref_axis',(-1.,0.,0.));
#26746=DIRECTION('center_axis',(1.,0.,0.));
#26747=DIRECTION('ref_axis',(0.,0.,1.));
#26748=DIRECTION('',(0.,-1.,0.));
#26749=DIRECTION('',(0.,0.,1.));
#26750=DIRECTION('center_axis',(0.,1.,0.));
#26751=DIRECTION('ref_axis',(-0.245760053518537,0.,-0.969330694909929));
#26752=DIRECTION('',(0.,-1.,0.));
#26753=DIRECTION('center_axis',(0.,1.,0.));
#26754=DIRECTION('ref_axis',(-0.245760053518537,0.,-0.969330694909929));
#26755=DIRECTION('center_axis',(0.,1.,0.));
#26756=DIRECTION('ref_axis',(0.245760053518569,0.,0.969330694909921));
#26757=DIRECTION('',(0.,-1.,0.));
#26758=DIRECTION('center_axis',(0.,-1.,0.));
#26759=DIRECTION('ref_axis',(0.245760053518569,0.,0.969330694909921));
#26760=DIRECTION('center_axis',(0.,1.,0.));
#26761=DIRECTION('ref_axis',(-0.711979844231348,0.,-0.702199901316075));
#26762=DIRECTION('',(0.,-1.,0.));
#26763=DIRECTION('center_axis',(0.,1.,0.));
#26764=DIRECTION('ref_axis',(-0.711979844231348,0.,-0.702199901316075));
#26765=DIRECTION('center_axis',(0.71197984423134,0.,0.702199901316083));
#26766=DIRECTION('ref_axis',(-0.702199901316083,0.,0.71197984423134));
#26767=DIRECTION('',(0.,-1.,0.));
#26768=DIRECTION('',(-0.702199901316083,0.,0.71197984423134));
#26769=DIRECTION('center_axis',(0.,1.,0.));
#26770=DIRECTION('ref_axis',(0.711979844231334,0.,0.702199901316089));
#26771=DIRECTION('',(0.,-1.,0.));
#26772=DIRECTION('center_axis',(0.,-1.,0.));
#26773=DIRECTION('ref_axis',(0.711979844231334,0.,0.702199901316089));
#26774=DIRECTION('center_axis',(1.,0.,0.));
#26775=DIRECTION('ref_axis',(0.,0.,1.));
#26776=DIRECTION('',(0.,-1.,0.));
#26777=DIRECTION('',(0.,0.,1.));
#26778=DIRECTION('center_axis',(0.,1.,0.));
#26779=DIRECTION('ref_axis',(1.,0.,1.69176841847649E-14));
#26780=DIRECTION('',(0.,-1.,0.));
#26781=DIRECTION('center_axis',(0.,-1.,0.));
#26782=DIRECTION('ref_axis',(1.,0.,1.69176841847649E-14));
#26783=DIRECTION('center_axis',(0.709478283082607,0.,-0.704727298913669));
#26784=DIRECTION('ref_axis',(0.704727298913669,0.,0.709478283082607));
#26785=DIRECTION('',(0.,-1.,0.));
#26786=DIRECTION('',(0.704727298913669,0.,0.709478283082607));
#26787=DIRECTION('center_axis',(0.,1.,0.));
#26788=DIRECTION('ref_axis',(-1.,0.,-4.03717463500059E-15));
#26789=DIRECTION('',(0.,-1.,0.));
#26790=DIRECTION('center_axis',(0.,1.,0.));
#26791=DIRECTION('ref_axis',(-1.,0.,-4.03717463500059E-15));
#26792=DIRECTION('center_axis',(1.,0.,0.));
#26793=DIRECTION('ref_axis',(0.,0.,1.));
#26794=DIRECTION('',(0.,-1.,0.));
#26795=DIRECTION('',(0.,0.,1.));
#26796=DIRECTION('center_axis',(0.707376432457449,0.,0.706837027046385));
#26797=DIRECTION('ref_axis',(-0.706837027046385,0.,0.707376432457449));
#26798=DIRECTION('',(0.,-1.,0.));
#26799=DIRECTION('',(-0.706837027046385,0.,0.707376432457449));
#26800=DIRECTION('center_axis',(0.,0.,1.));
#26801=DIRECTION('ref_axis',(-1.,0.,0.));
#26802=DIRECTION('',(1.,0.,-2.53764096072769E-16));
#26803=DIRECTION('center_axis',(0.,0.,-1.));
#26804=DIRECTION('ref_axis',(1.,0.,0.));
#26805=DIRECTION('',(1.,0.,0.));
#26806=DIRECTION('center_axis',(0.,1.,0.));
#26807=DIRECTION('ref_axis',(1.,0.,0.));
#26808=DIRECTION('axis',(0.,0.,1.));
#26809=DIRECTION('refdir',(1.,0.,0.));
#26810=DIRECTION('center_axis',(0.,1.,0.));
#26811=DIRECTION('ref_axis',(1.,0.,0.));
#26812=DIRECTION('center_axis',(0.,1.,0.));
#26813=DIRECTION('ref_axis',(1.,0.,0.));
#26814=DIRECTION('',(0.,1.,0.));
#26815=DIRECTION('center_axis',(0.,-1.,0.));
#26816=DIRECTION('ref_axis',(1.,0.,0.));
#26817=DIRECTION('center_axis',(-1.,0.,0.));
#26818=DIRECTION('ref_axis',(0.,0.,1.));
#26819=DIRECTION('',(0.,0.,-1.));
#26820=DIRECTION('',(0.,1.,0.));
#26821=DIRECTION('',(0.,0.,1.));
#26822=DIRECTION('',(0.,1.,0.));
#26823=DIRECTION('center_axis',(0.,0.,-1.));
#26824=DIRECTION('ref_axis',(-1.,0.,0.));
#26825=DIRECTION('',(1.,0.,0.));
#26826=DIRECTION('',(-1.,0.,0.));
#26827=DIRECTION('',(0.,1.,0.));
#26828=DIRECTION('center_axis',(1.,0.,0.));
#26829=DIRECTION('ref_axis',(0.,0.,-1.));
#26830=DIRECTION('',(0.,0.,1.));
#26831=DIRECTION('',(0.,0.,-1.));
#26832=DIRECTION('',(0.,1.,0.));
#26833=DIRECTION('center_axis',(0.,0.,1.));
#26834=DIRECTION('ref_axis',(1.,0.,0.));
#26835=DIRECTION('',(-1.,0.,0.));
#26836=DIRECTION('',(1.,0.,0.));
#26837=DIRECTION('center_axis',(0.,1.,0.));
#26838=DIRECTION('ref_axis',(0.,0.,1.));
#26839=DIRECTION('center_axis',(0.,1.,0.));
#26840=DIRECTION('ref_axis',(1.,0.,0.));
#26841=DIRECTION('axis',(0.,0.,1.));
#26842=DIRECTION('refdir',(1.,0.,0.));
#26843=DIRECTION('center_axis',(0.,-1.,0.));
#26844=DIRECTION('ref_axis',(-1.,0.,0.));
#26845=DIRECTION('center_axis',(0.,-1.,0.));
#26846=DIRECTION('ref_axis',(-1.,0.,0.));
#26847=DIRECTION('',(0.,-1.,0.));
#26848=DIRECTION('center_axis',(0.,-1.,0.));
#26849=DIRECTION('ref_axis',(-1.,0.,0.));
#26850=DIRECTION('center_axis',(-1.,0.,0.));
#26851=DIRECTION('ref_axis',(0.,0.,1.));
#26852=DIRECTION('',(0.,0.,-1.));
#26853=DIRECTION('',(0.,-1.,0.));
#26854=DIRECTION('',(0.,0.,1.));
#26855=DIRECTION('',(0.,1.,0.));
#26856=DIRECTION('center_axis',(0.,0.,-1.));
#26857=DIRECTION('ref_axis',(-1.,0.,0.));
#26858=DIRECTION('',(1.,0.,0.));
#26859=DIRECTION('',(-1.,0.,0.));
#26860=DIRECTION('',(0.,1.,0.));
#26861=DIRECTION('center_axis',(1.,0.,0.));
#26862=DIRECTION('ref_axis',(0.,0.,-1.));
#26863=DIRECTION('',(0.,0.,1.));
#26864=DIRECTION('',(0.,0.,-1.));
#26865=DIRECTION('',(0.,1.,0.));
#26866=DIRECTION('center_axis',(0.,0.,1.));
#26867=DIRECTION('ref_axis',(1.,0.,0.));
#26868=DIRECTION('',(-1.,0.,0.));
#26869=DIRECTION('',(-1.,0.,0.));
#26870=DIRECTION('center_axis',(0.,1.,0.));
#26871=DIRECTION('ref_axis',(0.,0.,1.));
#26872=DIRECTION('center_axis',(0.,1.,0.));
#26873=DIRECTION('ref_axis',(1.,0.,0.));
#26874=DIRECTION('axis',(0.,0.,1.));
#26875=DIRECTION('refdir',(1.,0.,0.));
#26876=DIRECTION('center_axis',(0.,1.,0.));
#26877=DIRECTION('ref_axis',(-1.,0.,0.));
#26878=DIRECTION('center_axis',(0.,-1.,0.));
#26879=DIRECTION('ref_axis',(-1.,0.,0.));
#26880=DIRECTION('',(0.,-1.,0.));
#26881=DIRECTION('center_axis',(0.,1.,0.));
#26882=DIRECTION('ref_axis',(-1.,0.,0.));
#26883=DIRECTION('center_axis',(-1.,0.,0.));
#26884=DIRECTION('ref_axis',(0.,0.,1.));
#26885=DIRECTION('',(0.,0.,1.));
#26886=DIRECTION('',(0.,1.,0.));
#26887=DIRECTION('',(0.,0.,1.));
#26888=DIRECTION('',(0.,1.,0.));
#26889=DIRECTION('center_axis',(0.,0.,-1.));
#26890=DIRECTION('ref_axis',(-1.,0.,0.));
#26891=DIRECTION('',(-1.,0.,0.));
#26892=DIRECTION('',(-1.,0.,0.));
#26893=DIRECTION('',(0.,1.,0.));
#26894=DIRECTION('center_axis',(1.,0.,0.));
#26895=DIRECTION('ref_axis',(0.,0.,-1.));
#26896=DIRECTION('',(0.,0.,-1.));
#26897=DIRECTION('',(0.,0.,-1.));
#26898=DIRECTION('',(0.,1.,0.));
#26899=DIRECTION('center_axis',(0.,0.,1.));
#26900=DIRECTION('ref_axis',(1.,0.,0.));
#26901=DIRECTION('',(1.,0.,0.));
#26902=DIRECTION('',(1.,0.,0.));
#26903=DIRECTION('center_axis',(0.,-1.,0.));
#26904=DIRECTION('ref_axis',(-1.,0.,0.));
#26905=DIRECTION('center_axis',(0.,-1.,0.));
#26906=DIRECTION('ref_axis',(-1.,0.,0.));
#26907=DIRECTION('axis',(0.,0.,1.));
#26908=DIRECTION('refdir',(1.,0.,0.));
#26909=DIRECTION('center_axis',(0.710729249896214,0.,-0.703465658964221));
#26910=DIRECTION('ref_axis',(0.703465658964221,0.,0.710729249896214));
#26911=DIRECTION('',(0.,1.,0.));
#26912=DIRECTION('',(-0.703465658964221,0.,-0.710729249896214));
#26913=DIRECTION('',(0.,-1.,0.));
#26914=DIRECTION('',(0.703465658964221,0.,0.710729249896214));
#26915=DIRECTION('center_axis',(0.,1.,0.));
#26916=DIRECTION('ref_axis',(-0.963381374692954,0.,0.268134904282738));
#26917=DIRECTION('center_axis',(0.,-1.,0.));
#26918=DIRECTION('ref_axis',(-0.963381374692954,0.,0.268134904282738));
#26919=DIRECTION('',(0.,-1.,0.));
#26920=DIRECTION('center_axis',(0.,1.,0.));
#26921=DIRECTION('ref_axis',(-0.963381374692954,0.,0.268134904282738));
#26922=DIRECTION('center_axis',(0.,1.,0.));
#26923=DIRECTION('ref_axis',(0.963381374692978,0.,-0.268134904282653));
#26924=DIRECTION('center_axis',(0.,1.,0.));
#26925=DIRECTION('ref_axis',(0.963381374692978,0.,-0.268134904282653));
#26926=DIRECTION('',(0.,-1.,0.));
#26927=DIRECTION('center_axis',(0.,-1.,0.));
#26928=DIRECTION('ref_axis',(0.963381374692978,0.,-0.268134904282653));
#26929=DIRECTION('center_axis',(0.,1.,0.));
#26930=DIRECTION('ref_axis',(-1.,0.,-2.53764096072769E-16));
#26931=DIRECTION('center_axis',(0.,-1.,0.));
#26932=DIRECTION('ref_axis',(-1.,0.,-2.53764096072769E-16));
#26933=DIRECTION('',(0.,-1.,0.));
#26934=DIRECTION('center_axis',(0.,1.,0.));
#26935=DIRECTION('ref_axis',(-1.,0.,-2.53764096072769E-16));
#26936=DIRECTION('center_axis',(1.,0.,2.53764096072769E-16));
#26937=DIRECTION('ref_axis',(-2.53764096072769E-16,0.,1.));
#26938=DIRECTION('',(2.53764096072769E-16,0.,-1.));
#26939=DIRECTION('',(0.,-1.,0.));
#26940=DIRECTION('',(-2.53764096072769E-16,0.,1.));
#26941=DIRECTION('center_axis',(0.,1.,0.));
#26942=DIRECTION('ref_axis',(-0.245760053518537,0.,-0.969330694909929));
#26943=DIRECTION('center_axis',(0.,-1.,0.));
#26944=DIRECTION('ref_axis',(-0.245760053518537,0.,-0.969330694909929));
#26945=DIRECTION('',(0.,-1.,0.));
#26946=DIRECTION('center_axis',(0.,1.,0.));
#26947=DIRECTION('ref_axis',(-0.245760053518537,0.,-0.969330694909929));
#26948=DIRECTION('center_axis',(0.,1.,0.));
#26949=DIRECTION('ref_axis',(0.245760053518569,0.,0.969330694909921));
#26950=DIRECTION('center_axis',(0.,1.,0.));
#26951=DIRECTION('ref_axis',(0.245760053518569,0.,0.969330694909921));
#26952=DIRECTION('',(0.,-1.,0.));
#26953=DIRECTION('center_axis',(0.,-1.,0.));
#26954=DIRECTION('ref_axis',(0.245760053518569,0.,0.969330694909921));
#26955=DIRECTION('center_axis',(0.,1.,0.));
#26956=DIRECTION('ref_axis',(-0.711979844231348,0.,-0.702199901316075));
#26957=DIRECTION('center_axis',(0.,-1.,0.));
#26958=DIRECTION('ref_axis',(-0.711979844231348,0.,-0.702199901316075));
#26959=DIRECTION('',(0.,-1.,0.));
#26960=DIRECTION('center_axis',(0.,1.,0.));
#26961=DIRECTION('ref_axis',(-0.711979844231348,0.,-0.702199901316075));
#26962=DIRECTION('center_axis',(0.71197984423134,0.,0.702199901316083));
#26963=DIRECTION('ref_axis',(-0.702199901316083,0.,0.71197984423134));
#26964=DIRECTION('',(0.702199901316083,0.,-0.71197984423134));
#26965=DIRECTION('',(0.,-1.,0.));
#26966=DIRECTION('',(-0.702199901316083,0.,0.71197984423134));
#26967=DIRECTION('center_axis',(0.,1.,0.));
#26968=DIRECTION('ref_axis',(0.711979844231334,0.,0.702199901316089));
#26969=DIRECTION('center_axis',(0.,1.,0.));
#26970=DIRECTION('ref_axis',(0.711979844231334,0.,0.702199901316089));
#26971=DIRECTION('',(0.,-1.,0.));
#26972=DIRECTION('center_axis',(0.,-1.,0.));
#26973=DIRECTION('ref_axis',(0.711979844231334,0.,0.702199901316089));
#26974=DIRECTION('center_axis',(1.,0.,2.53764096072769E-16));
#26975=DIRECTION('ref_axis',(-2.53764096072769E-16,0.,1.));
#26976=DIRECTION('',(2.53764096072769E-16,0.,-1.));
#26977=DIRECTION('',(0.,-1.,0.));
#26978=DIRECTION('',(-2.53764096072769E-16,0.,1.));
#26979=DIRECTION('center_axis',(0.,1.,0.));
#26980=DIRECTION('ref_axis',(1.,0.,1.71714482808377E-14));
#26981=DIRECTION('center_axis',(0.,1.,0.));
#26982=DIRECTION('ref_axis',(1.,0.,1.71714482808377E-14));
#26983=DIRECTION('',(0.,-1.,0.));
#26984=DIRECTION('center_axis',(0.,-1.,0.));
#26985=DIRECTION('ref_axis',(1.,0.,1.71714482808377E-14));
#26986=DIRECTION('center_axis',(0.709478283082607,0.,-0.704727298913669));
#26987=DIRECTION('ref_axis',(0.704727298913669,0.,0.709478283082607));
#26988=DIRECTION('',(-0.704727298913669,0.,-0.709478283082607));
#26989=DIRECTION('',(0.,-1.,0.));
#26990=DIRECTION('',(0.704727298913669,0.,0.709478283082607));
#26991=DIRECTION('center_axis',(0.,1.,0.));
#26992=DIRECTION('ref_axis',(-1.,0.,-4.29093873107336E-15));
#26993=DIRECTION('center_axis',(0.,-1.,0.));
#26994=DIRECTION('ref_axis',(-1.,0.,-4.29093873107336E-15));
#26995=DIRECTION('',(0.,-1.,0.));
#26996=DIRECTION('center_axis',(0.,1.,0.));
#26997=DIRECTION('ref_axis',(-1.,0.,-4.29093873107336E-15));
#26998=DIRECTION('center_axis',(1.,0.,2.53764096072769E-16));
#26999=DIRECTION('ref_axis',(-2.53764096072769E-16,0.,1.));
#27000=DIRECTION('',(2.53764096072769E-16,0.,-1.));
#27001=DIRECTION('',(0.,-1.,0.));
#27002=DIRECTION('',(-2.53764096072769E-16,0.,1.));
#27003=DIRECTION('center_axis',(0.707376432457449,0.,0.706837027046385));
#27004=DIRECTION('ref_axis',(-0.706837027046385,0.,0.707376432457449));
#27005=DIRECTION('',(0.706837027046385,0.,-0.707376432457449));
#27006=DIRECTION('',(0.,-1.,0.));
#27007=DIRECTION('',(-0.706837027046385,0.,0.707376432457449));
#27008=DIRECTION('center_axis',(0.,-1.,0.));
#27009=DIRECTION('ref_axis',(-1.,0.,0.));
#27010=DIRECTION('',(-1.,0.,-2.53764096072769E-16));
#27011=DIRECTION('',(0.703465658964221,0.,-0.710729249896213));
#27012=DIRECTION('center_axis',(0.,1.,0.));
#27013=DIRECTION('ref_axis',(0.963381374692954,0.,0.268134904282739));
#27014=DIRECTION('center_axis',(0.,-1.,0.));
#27015=DIRECTION('ref_axis',(-0.963381374692978,0.,-0.268134904282653));
#27016=DIRECTION('center_axis',(0.,1.,0.));
#27017=DIRECTION('ref_axis',(1.,0.,0.));
#27018=DIRECTION('',(0.,0.,-1.));
#27019=DIRECTION('center_axis',(0.,1.,0.));
#27020=DIRECTION('ref_axis',(0.245760053518537,0.,-0.969330694909929));
#27021=DIRECTION('center_axis',(0.,-1.,0.));
#27022=DIRECTION('ref_axis',(-0.245760053518569,0.,0.969330694909921));
#27023=DIRECTION('center_axis',(0.,1.,0.));
#27024=DIRECTION('ref_axis',(0.711979844231348,0.,-0.702199901316075));
#27025=DIRECTION('',(-0.702199901316083,0.,-0.71197984423134));
#27026=DIRECTION('center_axis',(0.,-1.,0.));
#27027=DIRECTION('ref_axis',(-0.711979844231334,0.,0.702199901316089));
#27028=DIRECTION('',(0.,0.,-1.));
#27029=DIRECTION('center_axis',(0.,-1.,0.));
#27030=DIRECTION('ref_axis',(-1.,0.,1.69176841847649E-14));
#27031=DIRECTION('',(0.704727298913669,0.,-0.709478283082607));
#27032=DIRECTION('center_axis',(0.,1.,0.));
#27033=DIRECTION('ref_axis',(1.,0.,-4.03717463500059E-15));
#27034=DIRECTION('',(0.,0.,-1.));
#27035=DIRECTION('',(-0.706837027046385,0.,-0.707376432457449));
#27036=DIRECTION('',(-1.,0.,0.));
#27037=DIRECTION('center_axis',(0.710729249896213,0.,0.703465658964221));
#27038=DIRECTION('ref_axis',(-0.703465658964221,0.,0.710729249896213));
#27039=DIRECTION('',(0.,1.,0.));
#27040=DIRECTION('',(-0.703465658964221,0.,0.710729249896213));
#27041=DIRECTION('',(0.,-1.,0.));
#27042=DIRECTION('center_axis',(0.,-1.,0.));
#27043=DIRECTION('ref_axis',(0.963381374692954,0.,0.268134904282739));
#27044=DIRECTION('center_axis',(0.,-1.,0.));
#27045=DIRECTION('ref_axis',(0.963381374692954,0.,0.268134904282739));
#27046=DIRECTION('',(0.,-1.,0.));
#27047=DIRECTION('center_axis',(0.,-1.,0.));
#27048=DIRECTION('ref_axis',(-0.963381374692978,0.,-0.268134904282653));
#27049=DIRECTION('center_axis',(0.,1.,0.));
#27050=DIRECTION('ref_axis',(-0.963381374692978,0.,-0.268134904282653));
#27051=DIRECTION('',(0.,-1.,0.));
#27052=DIRECTION('center_axis',(0.,-1.,0.));
#27053=DIRECTION('ref_axis',(1.,0.,0.));
#27054=DIRECTION('center_axis',(0.,-1.,0.));
#27055=DIRECTION('ref_axis',(1.,0.,0.));
#27056=DIRECTION('',(0.,-1.,0.));
#27057=DIRECTION('center_axis',(1.,0.,0.));
#27058=DIRECTION('ref_axis',(0.,0.,1.));
#27059=DIRECTION('',(0.,0.,1.));
#27060=DIRECTION('',(0.,-1.,0.));
#27061=DIRECTION('center_axis',(0.,-1.,0.));
#27062=DIRECTION('ref_axis',(0.245760053518537,0.,-0.969330694909929));
#27063=DIRECTION('center_axis',(0.,-1.,0.));
#27064=DIRECTION('ref_axis',(0.245760053518537,0.,-0.969330694909929));
#27065=DIRECTION('',(0.,-1.,0.));
#27066=DIRECTION('center_axis',(0.,-1.,0.));
#27067=DIRECTION('ref_axis',(-0.245760053518569,0.,0.969330694909921));
#27068=DIRECTION('center_axis',(0.,1.,0.));
#27069=DIRECTION('ref_axis',(-0.245760053518569,0.,0.969330694909921));
#27070=DIRECTION('',(0.,-1.,0.));
#27071=DIRECTION('center_axis',(0.,-1.,0.));
#27072=DIRECTION('ref_axis',(0.711979844231348,0.,-0.702199901316075));
#27073=DIRECTION('center_axis',(0.,-1.,0.));
#27074=DIRECTION('ref_axis',(0.711979844231348,0.,-0.702199901316075));
#27075=DIRECTION('',(0.,-1.,0.));
#27076=DIRECTION('center_axis',(0.71197984423134,0.,-0.702199901316083));
#27077=DIRECTION('ref_axis',(0.702199901316083,0.,0.71197984423134));
#27078=DIRECTION('',(0.702199901316083,0.,0.71197984423134));
#27079=DIRECTION('',(0.,-1.,0.));
#27080=DIRECTION('center_axis',(0.,-1.,0.));
#27081=DIRECTION('ref_axis',(-0.711979844231334,0.,0.702199901316089));
#27082=DIRECTION('center_axis',(0.,1.,0.));
#27083=DIRECTION('ref_axis',(-0.711979844231334,0.,0.702199901316089));
#27084=DIRECTION('',(0.,-1.,0.));
#27085=DIRECTION('center_axis',(1.,0.,0.));
#27086=DIRECTION('ref_axis',(0.,0.,1.));
#27087=DIRECTION('',(0.,0.,1.));
#27088=DIRECTION('',(0.,-1.,0.));
#27089=DIRECTION('center_axis',(0.,-1.,0.));
#27090=DIRECTION('ref_axis',(-1.,0.,1.69176841847649E-14));
#27091=DIRECTION('center_axis',(0.,1.,0.));
#27092=DIRECTION('ref_axis',(-1.,0.,1.69176841847649E-14));
#27093=DIRECTION('',(0.,-1.,0.));
#27094=DIRECTION('center_axis',(0.709478283082607,0.,0.704727298913669));
#27095=DIRECTION('ref_axis',(-0.704727298913669,0.,0.709478283082607));
#27096=DIRECTION('',(-0.704727298913669,0.,0.709478283082607));
#27097=DIRECTION('',(0.,-1.,0.));
#27098=DIRECTION('center_axis',(0.,-1.,0.));
#27099=DIRECTION('ref_axis',(1.,0.,-4.03717463500059E-15));
#27100=DIRECTION('center_axis',(0.,-1.,0.));
#27101=DIRECTION('ref_axis',(1.,0.,-4.03717463500059E-15));
#27102=DIRECTION('',(0.,-1.,0.));
#27103=DIRECTION('center_axis',(1.,0.,0.));
#27104=DIRECTION('ref_axis',(0.,0.,1.));
#27105=DIRECTION('',(0.,0.,1.));
#27106=DIRECTION('',(0.,-1.,0.));
#27107=DIRECTION('center_axis',(0.707376432457449,0.,-0.706837027046385));
#27108=DIRECTION('ref_axis',(0.706837027046385,0.,0.707376432457449));
#27109=DIRECTION('',(0.706837027046385,0.,0.707376432457449));
#27110=DIRECTION('',(0.,-1.,0.));
#27111=DIRECTION('center_axis',(0.,0.,-1.));
#27112=DIRECTION('ref_axis',(1.,0.,0.));
#27113=DIRECTION('',(-1.,0.,-2.53764096072769E-16));
#27114=DIRECTION('center_axis',(0.,0.,1.));
#27115=DIRECTION('ref_axis',(-1.,0.,0.));
#27116=DIRECTION('',(-1.,0.,0.));
#27117=DIRECTION('center_axis',(0.,-1.,0.));
#27118=DIRECTION('ref_axis',(-1.,0.,0.));
#27119=DIRECTION('',(0.,0.,1.));
#27120=DIRECTION('',(1.,0.,0.));
#27121=DIRECTION('',(-1.86482773667507E-17,-1.,-2.91433543964104E-16));
#27122=DIRECTION('',(1.,2.21177243187043E-17,-5.55111512312578E-17));
#27123=DIRECTION('',(0.,0.,-1.));
#27124=DIRECTION('',(-1.,0.,0.));
#27125=DIRECTION('',(0.,0.,-1.));
#27126=DIRECTION('',(-1.,0.,0.));
#27127=DIRECTION('',(0.,0.,1.));
#27128=DIRECTION('',(1.,0.,0.));
#27129=DIRECTION('',(-1.86482773667505E-17,-1.,-2.91433543964103E-16));
#27130=DIRECTION('',(1.,2.21177243187045E-17,-5.55111512312572E-17));
#27131=DIRECTION('',(0.,0.,1.));
#27132=DIRECTION('',(1.,0.,0.));
#27133=DIRECTION('',(0.,0.,1.));
#27134=DIRECTION('',(1.,0.,0.));
#27135=DIRECTION('',(0.,0.,1.));
#27136=DIRECTION('',(1.,0.,0.));
#27137=DIRECTION('',(0.,0.,1.));
#27138=DIRECTION('',(1.,0.,0.));
#27139=DIRECTION('',(0.,0.,1.));
#27140=DIRECTION('',(1.,0.,0.));
#27141=DIRECTION('',(0.,0.,1.));
#27142=DIRECTION('',(1.,0.,0.));
#27143=DIRECTION('',(0.,0.,1.));
#27144=DIRECTION('',(1.,0.,0.));
#27145=DIRECTION('',(0.,0.,1.));
#27146=DIRECTION('',(1.,0.,0.));
#27147=CARTESIAN_POINT('',(0.,0.,0.));
#27148=CARTESIAN_POINT('',(0.,0.,0.));
#27149=CARTESIAN_POINT('Origin',(103.778785519041,230.,0.));
#27150=CARTESIAN_POINT('',(113.356459668193,230.,-58.0910625167936));
#27151=CARTESIAN_POINT('',(113.356459668193,230.,-36.0032237681315));
#27152=CARTESIAN_POINT('',(113.356459668193,230.,-29.0455312583968));
#27153=CARTESIAN_POINT('',(114.856459668193,230.,-34.5032237681315));
#27154=CARTESIAN_POINT('',(119.962847072938,230.,-29.3968363633866));
#27155=CARTESIAN_POINT('',(125.314401519217,230.,-34.5032237681315));
#27156=CARTESIAN_POINT('',(109.317622593617,230.,-34.5032237681315));
#27157=CARTESIAN_POINT('',(127.968500624638,230.,-37.1752157277839));
#27158=CARTESIAN_POINT('',(111.34106001963,230.,-20.435679696352));
#27159=CARTESIAN_POINT('',(128.273548427401,230.,-37.9151793916432));
#27160=CARTESIAN_POINT('Origin',(127.223548427401,230.,-37.9151793916432));
#27161=CARTESIAN_POINT('',(128.273548427401,230.,-39.4187321117283));
#27162=CARTESIAN_POINT('',(128.273548427401,230.,-18.9575896958216));
#27163=CARTESIAN_POINT('',(127.971127263844,230.,-40.1560420081102));
#27164=CARTESIAN_POINT('Origin',(127.223548427401,230.,-39.4187321117283));
#27165=CARTESIAN_POINT('',(127.333356762198,230.,-40.8026951072716));
#27166=CARTESIAN_POINT('',(132.044740758987,230.,-36.025692948968));
#27167=CARTESIAN_POINT('',(126.997701127708,230.,-41.3560806824536));
#27168=CARTESIAN_POINT('Origin',(128.330128544122,230.,-41.785774969114));
#27169=CARTESIAN_POINT('',(125.328762843953,230.,-42.9220241352404));
#27170=CARTESIAN_POINT('Origin',(124.747780443448,230.,-40.6305041508116));
#27171=CARTESIAN_POINT('',(124.876218876064,230.,-43.5036225521864));
#27172=CARTESIAN_POINT('Origin',(125.476218876064,230.,-43.5036225521863));
#27173=CARTESIAN_POINT('',(124.876218876064,230.,-44.4226470147914));
#27174=CARTESIAN_POINT('',(124.876218876064,230.,-21.751811276093));
#27175=CARTESIAN_POINT('',(125.387243744723,230.,-45.1153516005764));
#27176=CARTESIAN_POINT('Origin',(125.601218876064,230.,-44.4226470147914));
#27177=CARTESIAN_POINT('',(127.036092546462,230.,-46.8112703207193));
#27178=CARTESIAN_POINT('Origin',(124.659008759128,230.,-47.4728765656934));
#27179=CARTESIAN_POINT('',(127.149786002621,230.,-47.007169160326));
#27180=CARTESIAN_POINT('Origin',(127.469614165074,230.,-46.690609613792));
#27181=CARTESIAN_POINT('',(127.637659789347,230.,-47.5000804575095));
#27182=CARTESIAN_POINT('',(109.61588112148,230.,-29.2922190342974));
#27183=CARTESIAN_POINT('',(142.094409841973,230.,-47.5000804575095));
#27184=CARTESIAN_POINT('',(115.708222654194,230.,-47.5000804575095));
#27185=CARTESIAN_POINT('',(142.5822836287,230.,-47.007169160326));
#27186=CARTESIAN_POINT('',(144.48829315277,230.,-45.0814792533986));
#27187=CARTESIAN_POINT('',(142.695977084858,230.,-46.8112703207193));
#27188=CARTESIAN_POINT('Origin',(142.262455466246,230.,-46.690609613792));
#27189=CARTESIAN_POINT('',(144.344825886597,230.,-45.1153516005764));
#27190=CARTESIAN_POINT('Origin',(145.073060872192,230.,-47.4728765656934));
#27191=CARTESIAN_POINT('',(144.855850755256,230.,-44.4226470147914));
#27192=CARTESIAN_POINT('Origin',(144.130850755256,230.,-44.4226470147914));
#27193=CARTESIAN_POINT('',(144.855850755256,230.,-43.5036225521863));
#27194=CARTESIAN_POINT('',(144.855850755256,230.,-22.2113235073957));
#27195=CARTESIAN_POINT('',(144.403306787367,230.,-42.9220241352404));
#27196=CARTESIAN_POINT('Origin',(144.255850755256,230.,-43.5036225521863));
#27197=CARTESIAN_POINT('',(142.734368503612,230.,-41.3560806824536));
#27198=CARTESIAN_POINT('Origin',(144.984289187872,230.,-40.6305041508117));
#27199=CARTESIAN_POINT('',(142.398712869122,230.,-40.8026951072716));
#27200=CARTESIAN_POINT('Origin',(141.401941087198,230.,-41.7857749691141));
#27201=CARTESIAN_POINT('',(141.760942367476,230.,-40.1560420081102));
#27202=CARTESIAN_POINT('',(122.677567086127,230.,-20.8068815557118));
#27203=CARTESIAN_POINT('',(141.458521203919,230.,-39.4187321117283));
#27204=CARTESIAN_POINT('Origin',(142.508521203919,230.,-39.4187321117283));
#27205=CARTESIAN_POINT('',(141.458521203919,230.,-37.9151793916432));
#27206=CARTESIAN_POINT('',(141.45852120392,230.,-19.7093660558644));
#27207=CARTESIAN_POINT('',(141.763569006683,230.,-37.1752157277839));
#27208=CARTESIAN_POINT('Origin',(142.508521203919,230.,-37.9151793916432));
#27209=CARTESIAN_POINT('',(144.417668112103,230.,-34.5032237681314));
#27210=CARTESIAN_POINT('',(141.62477097808,230.,-37.3149494761148));
#27211=CARTESIAN_POINT('',(154.875609963127,230.,-34.5032237681314));
#27212=CARTESIAN_POINT('',(124.098226815572,230.,-34.5032237681314));
#27213=CARTESIAN_POINT('',(156.375609963127,230.,-36.0032237681314));
#27214=CARTESIAN_POINT('',(133.475597910073,230.,-13.1032117150771));
#27215=CARTESIAN_POINT('',(156.375609963127,230.,-58.0910625167936));
#27216=CARTESIAN_POINT('',(156.375609963127,230.,-18.0016118840657));
#27217=CARTESIAN_POINT('',(155.375609963127,230.,-59.0910625167936));
#27218=CARTESIAN_POINT('',(154.960007558403,230.,-59.5066649215182));
#27219=CARTESIAN_POINT('',(114.356459668193,230.,-59.0910625167936));
#27220=CARTESIAN_POINT('',(150.62266449878,230.,-59.0910625167936));
#27221=CARTESIAN_POINT('',(120.773904182304,230.,-65.5085070309049));
#27222=CARTESIAN_POINT('Origin',(142.094409841973,255.,-47.5000804575095));
#27223=CARTESIAN_POINT('',(142.094409841973,216.,-47.5000804575095));
#27224=CARTESIAN_POINT('',(142.094409841973,255.,-47.5000804575095));
#27225=CARTESIAN_POINT('',(142.5822836287,216.,-47.007169160326));
#27226=CARTESIAN_POINT('',(142.5822836287,216.,-47.007169160326));
#27227=CARTESIAN_POINT('',(142.5822836287,255.,-47.007169160326));
#27228=CARTESIAN_POINT('Origin',(142.262455466246,255.,-46.690609613792));
#27229=CARTESIAN_POINT('',(142.695977084858,216.,-46.8112703207193));
#27230=CARTESIAN_POINT('Origin',(142.262455466246,216.,-46.690609613792));
#27231=CARTESIAN_POINT('',(142.695977084858,255.,-46.8112703207193));
#27232=CARTESIAN_POINT('Origin',(145.073060872192,255.,-47.4728765656934));
#27233=CARTESIAN_POINT('',(144.344825886597,216.,-45.1153516005764));
#27234=CARTESIAN_POINT('Origin',(145.073060872192,216.,-47.4728765656934));
#27235=CARTESIAN_POINT('',(144.344825886597,255.,-45.1153516005764));
#27236=CARTESIAN_POINT('Origin',(144.130850755256,255.,-44.4226470147914));
#27237=CARTESIAN_POINT('',(144.855850755256,216.,-44.4226470147914));
#27238=CARTESIAN_POINT('Origin',(144.130850755256,216.,-44.4226470147914));
#27239=CARTESIAN_POINT('',(144.855850755256,255.,-44.4226470147914));
#27240=CARTESIAN_POINT('Origin',(144.855850755256,255.,-44.4226470147914));
#27241=CARTESIAN_POINT('',(144.855850755256,216.,-43.5036225521863));
#27242=CARTESIAN_POINT('',(144.855850755256,216.,-43.5036225521863));
#27243=CARTESIAN_POINT('',(144.855850755256,255.,-43.5036225521863));
#27244=CARTESIAN_POINT('Origin',(144.255850755256,255.,-43.5036225521863));
#27245=CARTESIAN_POINT('',(144.403306787367,216.,-42.9220241352404));
#27246=CARTESIAN_POINT('Origin',(144.255850755256,216.,-43.5036225521863));
#27247=CARTESIAN_POINT('',(144.403306787367,255.,-42.9220241352404));
#27248=CARTESIAN_POINT('Origin',(144.984289187872,255.,-40.6305041508117));
#27249=CARTESIAN_POINT('',(142.734368503612,216.,-41.3560806824536));
#27250=CARTESIAN_POINT('Origin',(144.984289187872,216.,-40.6305041508117));
#27251=CARTESIAN_POINT('',(142.734368503612,255.,-41.3560806824536));
#27252=CARTESIAN_POINT('Origin',(141.401941087198,255.,-41.7857749691141));
#27253=CARTESIAN_POINT('',(142.398712869122,216.,-40.8026951072716));
#27254=CARTESIAN_POINT('Origin',(141.401941087198,216.,-41.7857749691141));
#27255=CARTESIAN_POINT('',(142.398712869122,255.,-40.8026951072716));
#27256=CARTESIAN_POINT('Origin',(142.398712869122,255.,-40.8026951072716));
#27257=CARTESIAN_POINT('',(141.760942367476,216.,-40.1560420081102));
#27258=CARTESIAN_POINT('',(141.760942367476,216.,-40.1560420081102));
#27259=CARTESIAN_POINT('',(141.760942367476,255.,-40.1560420081102));
#27260=CARTESIAN_POINT('Origin',(142.508521203919,255.,-39.4187321117283));
#27261=CARTESIAN_POINT('',(141.458521203919,216.,-39.4187321117283));
#27262=CARTESIAN_POINT('Origin',(142.508521203919,216.,-39.4187321117283));
#27263=CARTESIAN_POINT('',(141.458521203919,255.,-39.4187321117283));
#27264=CARTESIAN_POINT('Origin',(141.458521203919,255.,-39.4187321117283));
#27265=CARTESIAN_POINT('',(141.458521203919,216.,-37.9151793916432));
#27266=CARTESIAN_POINT('',(141.458521203919,216.,-37.9151793916432));
#27267=CARTESIAN_POINT('',(141.458521203919,255.,-37.9151793916432));
#27268=CARTESIAN_POINT('Origin',(142.508521203919,255.,-37.9151793916432));
#27269=CARTESIAN_POINT('',(141.763569006683,216.,-37.1752157277839));
#27270=CARTESIAN_POINT('Origin',(142.508521203919,216.,-37.9151793916432));
#27271=CARTESIAN_POINT('',(141.763569006683,255.,-37.1752157277839));
#27272=CARTESIAN_POINT('Origin',(141.763569006683,255.,-37.1752157277839));
#27273=CARTESIAN_POINT('',(144.417668112103,216.,-34.5032237681314));
#27274=CARTESIAN_POINT('',(144.544688744748,216.,-34.375346814161));
#27275=CARTESIAN_POINT('',(144.417668112103,255.,-34.5032237681314));
#27276=CARTESIAN_POINT('Origin',(144.417668112103,255.,-34.5032237681314));
#27277=CARTESIAN_POINT('',(154.875609963127,216.,-34.5032237681314));
#27278=CARTESIAN_POINT('',(134.86603481566,216.,-34.5032237681314));
#27279=CARTESIAN_POINT('',(154.875609963127,255.,-34.5032237681314));
#27280=CARTESIAN_POINT('Origin',(154.875609963127,255.,-34.5032237681314));
#27281=CARTESIAN_POINT('',(156.375609963127,216.,-36.0032237681314));
#27282=CARTESIAN_POINT('',(154.875609963127,216.,-34.5032237681314));
#27283=CARTESIAN_POINT('',(156.375609963127,255.,-36.0032237681314));
#27284=CARTESIAN_POINT('Origin',(156.375609963127,255.,-36.0032237681314));
#27285=CARTESIAN_POINT('',(156.375609963127,216.,-58.0910625167936));
#27286=CARTESIAN_POINT('',(156.375609963127,216.,-36.0032237681314));
#27287=CARTESIAN_POINT('',(156.375609963127,255.,-58.0910625167936));
#27288=CARTESIAN_POINT('Origin',(113.356459668193,255.,-58.0910625167937));
#27289=CARTESIAN_POINT('',(113.356459668193,216.,-58.0910625167937));
#27290=CARTESIAN_POINT('',(113.356459668193,255.,-58.0910625167937));
#27291=CARTESIAN_POINT('',(113.356459668193,216.,-36.0032237681315));
#27292=CARTESIAN_POINT('',(113.356459668193,216.,-36.0032237681315));
#27293=CARTESIAN_POINT('',(113.356459668193,255.,-36.0032237681315));
#27294=CARTESIAN_POINT('Origin',(113.356459668193,255.,-36.0032237681315));
#27295=CARTESIAN_POINT('',(114.856459668193,216.,-34.5032237681315));
#27296=CARTESIAN_POINT('',(114.856459668193,216.,-34.5032237681315));
#27297=CARTESIAN_POINT('',(114.856459668193,255.,-34.5032237681315));
#27298=CARTESIAN_POINT('Origin',(114.856459668193,255.,-34.5032237681315));
#27299=CARTESIAN_POINT('',(125.314401519217,216.,-34.5032237681315));
#27300=CARTESIAN_POINT('',(134.86603481566,216.,-34.5032237681314));
#27301=CARTESIAN_POINT('',(125.314401519217,255.,-34.5032237681315));
#27302=CARTESIAN_POINT('Origin',(125.314401519217,255.,-34.5032237681315));
#27303=CARTESIAN_POINT('',(127.968500624638,216.,-37.1752157277839));
#27304=CARTESIAN_POINT('',(127.968500624638,216.,-37.1752157277839));
#27305=CARTESIAN_POINT('',(127.968500624638,255.,-37.1752157277839));
#27306=CARTESIAN_POINT('Origin',(127.223548427401,255.,-37.9151793916432));
#27307=CARTESIAN_POINT('',(128.273548427401,216.,-37.9151793916432));
#27308=CARTESIAN_POINT('Origin',(127.223548427401,216.,-37.9151793916432));
#27309=CARTESIAN_POINT('',(128.273548427401,255.,-37.9151793916432));
#27310=CARTESIAN_POINT('Origin',(156.375609963127,255.,-58.0910625167936));
#27311=CARTESIAN_POINT('',(155.375609963127,216.,-59.0910625167936));
#27312=CARTESIAN_POINT('',(156.375609963127,216.,-58.0910625167936));
#27313=CARTESIAN_POINT('',(155.375609963127,255.,-59.0910625167936));
#27314=CARTESIAN_POINT('Origin',(155.375609963127,255.,-59.0910625167936));
#27315=CARTESIAN_POINT('',(114.356459668193,216.,-59.0910625167936));
#27316=CARTESIAN_POINT('',(155.375609963127,216.,-59.0910625167936));
#27317=CARTESIAN_POINT('',(114.356459668193,255.,-59.0910625167936));
#27318=CARTESIAN_POINT('Origin',(114.356459668193,255.,-59.0910625167936));
#27319=CARTESIAN_POINT('',(113.356459668193,216.,-58.0910625167937));
#27320=CARTESIAN_POINT('Origin',(128.273548427401,255.,-37.9151793916432));
#27321=CARTESIAN_POINT('',(128.273548427401,216.,-39.4187321117283));
#27322=CARTESIAN_POINT('',(128.273548427401,216.,-39.4187321117283));
#27323=CARTESIAN_POINT('',(128.273548427401,255.,-39.4187321117283));
#27324=CARTESIAN_POINT('Origin',(127.637659789347,255.,-47.5000804575095));
#27325=CARTESIAN_POINT('',(127.637659789347,216.,-47.5000804575095));
#27326=CARTESIAN_POINT('',(127.637659789347,255.,-47.5000804575095));
#27327=CARTESIAN_POINT('',(142.094409841973,216.,-47.5000804575095));
#27328=CARTESIAN_POINT('Origin',(127.149786002621,255.,-47.007169160326));
#27329=CARTESIAN_POINT('',(127.149786002621,216.,-47.007169160326));
#27330=CARTESIAN_POINT('',(127.149786002621,255.,-47.007169160326));
#27331=CARTESIAN_POINT('',(127.637659789347,216.,-47.5000804575095));
#27332=CARTESIAN_POINT('Origin',(127.469614165074,255.,-46.690609613792));
#27333=CARTESIAN_POINT('',(127.036092546462,216.,-46.8112703207193));
#27334=CARTESIAN_POINT('',(127.036092546462,255.,-46.8112703207193));
#27335=CARTESIAN_POINT('Origin',(127.469614165074,216.,-46.690609613792));
#27336=CARTESIAN_POINT('Origin',(124.659008759128,255.,-47.4728765656934));
#27337=CARTESIAN_POINT('',(125.387243744723,216.,-45.1153516005764));
#27338=CARTESIAN_POINT('',(125.387243744723,255.,-45.1153516005764));
#27339=CARTESIAN_POINT('Origin',(124.659008759128,216.,-47.4728765656934));
#27340=CARTESIAN_POINT('Origin',(125.601218876064,255.,-44.4226470147914));
#27341=CARTESIAN_POINT('',(124.876218876064,216.,-44.4226470147914));
#27342=CARTESIAN_POINT('',(124.876218876064,255.,-44.4226470147914));
#27343=CARTESIAN_POINT('Origin',(125.601218876064,216.,-44.4226470147914));
#27344=CARTESIAN_POINT('Origin',(124.876218876064,255.,-43.5036225521864));
#27345=CARTESIAN_POINT('',(124.876218876064,216.,-43.5036225521864));
#27346=CARTESIAN_POINT('',(124.876218876064,255.,-43.5036225521864));
#27347=CARTESIAN_POINT('',(124.876218876064,216.,-44.4226470147914));
#27348=CARTESIAN_POINT('Origin',(125.476218876064,255.,-43.5036225521863));
#27349=CARTESIAN_POINT('',(125.328762843953,216.,-42.9220241352404));
#27350=CARTESIAN_POINT('',(125.328762843953,255.,-42.9220241352404));
#27351=CARTESIAN_POINT('Origin',(125.476218876064,216.,-43.5036225521863));
#27352=CARTESIAN_POINT('Origin',(124.747780443448,255.,-40.6305041508116));
#27353=CARTESIAN_POINT('',(126.997701127708,216.,-41.3560806824536));
#27354=CARTESIAN_POINT('',(126.997701127708,255.,-41.3560806824536));
#27355=CARTESIAN_POINT('Origin',(124.747780443448,216.,-40.6305041508116));
#27356=CARTESIAN_POINT('Origin',(128.330128544122,255.,-41.785774969114));
#27357=CARTESIAN_POINT('',(127.333356762198,216.,-40.8026951072716));
#27358=CARTESIAN_POINT('',(127.333356762198,255.,-40.8026951072716));
#27359=CARTESIAN_POINT('Origin',(128.330128544122,216.,-41.785774969114));
#27360=CARTESIAN_POINT('Origin',(127.971127263844,255.,-40.1560420081102));
#27361=CARTESIAN_POINT('',(127.971127263844,216.,-40.1560420081102));
#27362=CARTESIAN_POINT('',(127.971127263844,255.,-40.1560420081102));
#27363=CARTESIAN_POINT('',(127.333356762198,216.,-40.8026951072716));
#27364=CARTESIAN_POINT('Origin',(127.223548427401,255.,-39.4187321117283));
#27365=CARTESIAN_POINT('Origin',(127.223548427401,216.,-39.4187321117283));
#27366=CARTESIAN_POINT('Origin',(134.86603481566,216.,-46.7971431424625));
#27367=CARTESIAN_POINT('Origin',(142.094409841973,255.,-47.5000804575095));
#27368=CARTESIAN_POINT('',(142.094409841973,230.,-47.5000804575095));
#27369=CARTESIAN_POINT('',(142.5822836287,230.,-47.007169160326));
#27370=CARTESIAN_POINT('',(144.48829315277,230.,-45.0814792533986));
#27371=CARTESIAN_POINT('',(142.5822836287,280.,-47.007169160326));
#27372=CARTESIAN_POINT('',(142.5822836287,255.,-47.007169160326));
#27373=CARTESIAN_POINT('',(142.094409841973,280.,-47.5000804575095));
#27374=CARTESIAN_POINT('',(144.655606318974,280.,-44.9124385054979));
#27375=CARTESIAN_POINT('',(142.094409841973,255.,-47.5000804575095));
#27376=CARTESIAN_POINT('Origin',(142.262455466246,255.,-46.690609613792));
#27377=CARTESIAN_POINT('',(142.695977084858,230.,-46.8112703207193));
#27378=CARTESIAN_POINT('Origin',(142.262455466246,230.,-46.690609613792));
#27379=CARTESIAN_POINT('',(142.695977084858,280.,-46.8112703207193));
#27380=CARTESIAN_POINT('',(142.695977084858,255.,-46.8112703207193));
#27381=CARTESIAN_POINT('Origin',(142.262455466246,280.,-46.690609613792));
#27382=CARTESIAN_POINT('Origin',(145.073060872192,255.,-47.4728765656934));
#27383=CARTESIAN_POINT('',(144.344825886597,230.,-45.1153516005764));
#27384=CARTESIAN_POINT('Origin',(145.073060872192,230.,-47.4728765656934));
#27385=CARTESIAN_POINT('',(144.344825886597,280.,-45.1153516005764));
#27386=CARTESIAN_POINT('',(144.344825886597,255.,-45.1153516005764));
#27387=CARTESIAN_POINT('Origin',(145.073060872192,280.,-47.4728765656934));
#27388=CARTESIAN_POINT('Origin',(144.130850755256,255.,-44.4226470147914));
#27389=CARTESIAN_POINT('',(144.855850755256,230.,-44.4226470147914));
#27390=CARTESIAN_POINT('Origin',(144.130850755256,230.,-44.4226470147914));
#27391=CARTESIAN_POINT('',(144.855850755256,280.,-44.4226470147914));
#27392=CARTESIAN_POINT('',(144.855850755256,255.,-44.4226470147914));
#27393=CARTESIAN_POINT('Origin',(144.130850755256,280.,-44.4226470147914));
#27394=CARTESIAN_POINT('Origin',(144.855850755256,255.,-44.4226470147914));
#27395=CARTESIAN_POINT('',(144.855850755256,230.,-43.5036225521863));
#27396=CARTESIAN_POINT('',(144.855850755256,230.,-22.2113235073957));
#27397=CARTESIAN_POINT('',(144.855850755256,280.,-43.5036225521863));
#27398=CARTESIAN_POINT('',(144.855850755256,255.,-43.5036225521863));
#27399=CARTESIAN_POINT('',(144.855850755256,280.,-22.2113235073957));
#27400=CARTESIAN_POINT('Origin',(144.255850755256,255.,-43.5036225521863));
#27401=CARTESIAN_POINT('',(144.403306787367,230.,-42.9220241352404));
#27402=CARTESIAN_POINT('Origin',(144.255850755256,230.,-43.5036225521863));
#27403=CARTESIAN_POINT('',(144.403306787367,280.,-42.9220241352404));
#27404=CARTESIAN_POINT('',(144.403306787367,255.,-42.9220241352404));
#27405=CARTESIAN_POINT('Origin',(144.255850755256,280.,-43.5036225521863));
#27406=CARTESIAN_POINT('Origin',(144.984289187872,255.,-40.6305041508117));
#27407=CARTESIAN_POINT('',(142.734368503612,230.,-41.3560806824536));
#27408=CARTESIAN_POINT('Origin',(144.984289187872,230.,-40.6305041508117));
#27409=CARTESIAN_POINT('',(142.734368503612,280.,-41.3560806824536));
#27410=CARTESIAN_POINT('',(142.734368503612,255.,-41.3560806824536));
#27411=CARTESIAN_POINT('Origin',(144.984289187872,280.,-40.6305041508117));
#27412=CARTESIAN_POINT('Origin',(145.869719034433,230.,-53.247581206998));
#27413=CARTESIAN_POINT('',(156.375609963127,230.,-46.4955106076453));
#27414=CARTESIAN_POINT('',(156.873403253207,230.,-46.9933038977248));
#27415=CARTESIAN_POINT('',(156.373403253207,230.,-46.4933038977248));
#27416=CARTESIAN_POINT('',(156.375609963127,230.,-36.0032237681314));
#27417=CARTESIAN_POINT('',(156.375609963127,230.,-18.0016118840657));
#27418=CARTESIAN_POINT('',(154.875609963127,230.,-34.5032237681314));
#27419=CARTESIAN_POINT('',(133.475597910073,230.,-13.1032117150771));
#27420=CARTESIAN_POINT('',(144.417668112103,230.,-34.5032237681314));
#27421=CARTESIAN_POINT('',(124.098226815572,230.,-34.5032237681314));
#27422=CARTESIAN_POINT('',(141.763569006683,230.,-37.1752157277839));
#27423=CARTESIAN_POINT('',(141.62477097808,230.,-37.3149494761148));
#27424=CARTESIAN_POINT('',(141.458521203919,230.,-37.9151793916432));
#27425=CARTESIAN_POINT('Origin',(142.508521203919,230.,-37.9151793916432));
#27426=CARTESIAN_POINT('',(141.458521203919,230.,-39.4187321117283));
#27427=CARTESIAN_POINT('',(141.45852120392,230.,-19.7093660558644));
#27428=CARTESIAN_POINT('',(141.760942367476,230.,-40.1560420081102));
#27429=CARTESIAN_POINT('Origin',(142.508521203919,230.,-39.4187321117283));
#27430=CARTESIAN_POINT('',(142.398712869122,230.,-40.8026951072716));
#27431=CARTESIAN_POINT('',(122.677567086127,230.,-20.8068815557118));
#27432=CARTESIAN_POINT('Origin',(141.401941087198,230.,-41.7857749691141));
#27433=CARTESIAN_POINT('',(127.637659789347,230.,-47.5000804575095));
#27434=CARTESIAN_POINT('',(115.708222654194,230.,-47.5000804575095));
#27435=CARTESIAN_POINT('',(127.149786002621,230.,-47.007169160326));
#27436=CARTESIAN_POINT('',(109.61588112148,230.,-29.2922190342974));
#27437=CARTESIAN_POINT('',(127.036092546462,230.,-46.8112703207193));
#27438=CARTESIAN_POINT('Origin',(127.469614165074,230.,-46.690609613792));
#27439=CARTESIAN_POINT('',(125.387243744723,230.,-45.1153516005764));
#27440=CARTESIAN_POINT('Origin',(124.659008759128,230.,-47.4728765656934));
#27441=CARTESIAN_POINT('',(124.876218876064,230.,-44.4226470147914));
#27442=CARTESIAN_POINT('Origin',(125.601218876064,230.,-44.4226470147914));
#27443=CARTESIAN_POINT('',(124.876218876064,230.,-43.5036225521864));
#27444=CARTESIAN_POINT('',(124.876218876064,230.,-21.751811276093));
#27445=CARTESIAN_POINT('',(125.328762843953,230.,-42.9220241352404));
#27446=CARTESIAN_POINT('Origin',(125.476218876064,230.,-43.5036225521863));
#27447=CARTESIAN_POINT('',(126.997701127708,230.,-41.3560806824536));
#27448=CARTESIAN_POINT('Origin',(124.747780443448,230.,-40.6305041508116));
#27449=CARTESIAN_POINT('',(127.333356762198,230.,-40.8026951072716));
#27450=CARTESIAN_POINT('Origin',(128.330128544122,230.,-41.785774969114));
#27451=CARTESIAN_POINT('',(127.971127263844,230.,-40.1560420081102));
#27452=CARTESIAN_POINT('',(132.044740758987,230.,-36.025692948968));
#27453=CARTESIAN_POINT('',(128.273548427401,230.,-39.4187321117283));
#27454=CARTESIAN_POINT('Origin',(127.223548427401,230.,-39.4187321117283));
#27455=CARTESIAN_POINT('',(128.273548427401,230.,-37.9151793916432));
#27456=CARTESIAN_POINT('',(128.273548427401,230.,-18.9575896958216));
#27457=CARTESIAN_POINT('',(127.968500624638,230.,-37.1752157277839));
#27458=CARTESIAN_POINT('Origin',(127.223548427401,230.,-37.9151793916432));
#27459=CARTESIAN_POINT('',(125.314401519217,230.,-34.5032237681315));
#27460=CARTESIAN_POINT('',(111.34106001963,230.,-20.435679696352));
#27461=CARTESIAN_POINT('',(114.856459668193,230.,-34.5032237681315));
#27462=CARTESIAN_POINT('',(109.317622593617,230.,-34.5032237681315));
#27463=CARTESIAN_POINT('',(113.356459668193,230.,-36.0032237681315));
#27464=CARTESIAN_POINT('',(119.962847072938,230.,-29.3968363633866));
#27465=CARTESIAN_POINT('',(113.356459668193,230.,-46.4955106076453));
#27466=CARTESIAN_POINT('',(113.356459668193,230.,-29.0455312583968));
#27467=CARTESIAN_POINT('',(112.858666378114,230.,-46.9933038977248));
#27468=CARTESIAN_POINT('',(113.358666378114,230.,-46.4933038977248));
#27469=CARTESIAN_POINT('',(112.858666378113,230.,-58.9996518063507));
#27470=CARTESIAN_POINT('',(112.858666378114,230.,-46.9933038977248));
#27471=CARTESIAN_POINT('',(113.858666378113,230.,-59.9996518063507));
#27472=CARTESIAN_POINT('',(112.858666378113,230.,-58.9996518063507));
#27473=CARTESIAN_POINT('',(122.862905683347,230.,-59.9996518063507));
#27474=CARTESIAN_POINT('',(113.858666378113,230.,-59.9996518063507));
#27475=CARTESIAN_POINT('',(124.265819387872,230.,-59.4840979918677));
#27476=CARTESIAN_POINT('Origin',(124.265819387872,230.,-61.6506638626042));
#27477=CARTESIAN_POINT('',(145.466250243448,230.,-59.4840979918677));
#27478=CARTESIAN_POINT('',(145.466250243448,230.,-59.4840979918677));
#27479=CARTESIAN_POINT('',(146.869163947974,230.,-59.9996518063508));
#27480=CARTESIAN_POINT('Origin',(145.466250243448,230.,-61.6506638626042));
#27481=CARTESIAN_POINT('',(155.873403253207,230.,-59.9996518063507));
#27482=CARTESIAN_POINT('',(155.873403253207,230.,-59.9996518063507));
#27483=CARTESIAN_POINT('',(156.873403253207,230.,-58.9996518063507));
#27484=CARTESIAN_POINT('',(156.873403253207,230.,-58.9996518063507));
#27485=CARTESIAN_POINT('',(156.873403253207,230.,-46.9933038977248));
#27486=CARTESIAN_POINT('Origin',(156.375609963127,255.,-46.4955106076453));
#27487=CARTESIAN_POINT('',(156.873403253207,280.,-46.9933038977248));
#27488=CARTESIAN_POINT('',(156.873403253207,255.,-46.9933038977248));
#27489=CARTESIAN_POINT('',(156.375609963127,280.,-46.4955106076453));
#27490=CARTESIAN_POINT('',(156.373403253207,280.,-46.4933038977248));
#27491=CARTESIAN_POINT('',(156.375609963127,255.,-46.4955106076453));
#27492=CARTESIAN_POINT('Origin',(156.873403253207,255.,-46.9933038977248));
#27493=CARTESIAN_POINT('',(156.873403253207,280.,-58.9996518063507));
#27494=CARTESIAN_POINT('',(156.873403253207,255.,-58.9996518063507));
#27495=CARTESIAN_POINT('',(156.873403253207,280.,-46.9933038977248));
#27496=CARTESIAN_POINT('Origin',(156.873403253207,255.,-58.9996518063507));
#27497=CARTESIAN_POINT('',(155.873403253207,280.,-59.9996518063507));
#27498=CARTESIAN_POINT('',(155.873403253207,255.,-59.9996518063507));
#27499=CARTESIAN_POINT('',(156.873403253207,280.,-58.9996518063507));
#27500=CARTESIAN_POINT('Origin',(155.873403253207,255.,-59.9996518063507));
#27501=CARTESIAN_POINT('',(146.869163947974,280.,-59.9996518063508));
#27502=CARTESIAN_POINT('',(146.869163947974,255.,-59.9996518063508));
#27503=CARTESIAN_POINT('',(155.873403253207,280.,-59.9996518063507));
#27504=CARTESIAN_POINT('',(154.37128360059,270.562970493524,-59.9996518063507));
#27505=CARTESIAN_POINT('Origin',(151.37128360059,270.562970493524,-59.9996518063507));
#27506=CARTESIAN_POINT('',(154.37128360059,238.562970493524,-59.9996518063507));
#27507=CARTESIAN_POINT('Origin',(151.37128360059,238.562970493524,-59.9996518063507));
#27508=CARTESIAN_POINT('Origin',(145.466250243448,255.,-61.6506638626042));
#27509=CARTESIAN_POINT('',(145.466250243448,280.,-59.4840979918677));
#27510=CARTESIAN_POINT('',(145.466250243448,255.,-59.4840979918677));
#27511=CARTESIAN_POINT('Origin',(145.466250243448,280.,-61.6506638626042));
#27512=CARTESIAN_POINT('Origin',(145.466250243448,255.,-59.4840979918677));
#27513=CARTESIAN_POINT('',(124.265819387872,280.,-59.4840979918677));
#27514=CARTESIAN_POINT('',(124.265819387872,255.,-59.4840979918677));
#27515=CARTESIAN_POINT('',(124.265819387872,280.,-59.4840979918677));
#27516=CARTESIAN_POINT('Origin',(145.869719034433,280.,-53.247581206998));
#27517=CARTESIAN_POINT('',(122.862905683347,280.,-59.9996518063507));
#27518=CARTESIAN_POINT('Origin',(124.265819387872,280.,-61.6506638626042));
#27519=CARTESIAN_POINT('',(113.858666378113,280.,-59.9996518063507));
#27520=CARTESIAN_POINT('',(113.858666378113,280.,-59.9996518063507));
#27521=CARTESIAN_POINT('',(112.858666378113,280.,-58.9996518063507));
#27522=CARTESIAN_POINT('',(112.858666378113,280.,-58.9996518063507));
#27523=CARTESIAN_POINT('',(112.858666378114,280.,-46.9933038977248));
#27524=CARTESIAN_POINT('',(112.858666378114,280.,-46.9933038977248));
#27525=CARTESIAN_POINT('',(113.356459668193,280.,-46.4955106076453));
#27526=CARTESIAN_POINT('',(113.358666378114,280.,-46.4933038977248));
#27527=CARTESIAN_POINT('',(113.356459668193,280.,-36.0032237681315));
#27528=CARTESIAN_POINT('',(113.356459668193,280.,-29.0455312583968));
#27529=CARTESIAN_POINT('',(114.856459668193,280.,-34.5032237681315));
#27530=CARTESIAN_POINT('',(120.131896739857,280.,-29.2277866964671));
#27531=CARTESIAN_POINT('',(125.314401519217,280.,-34.5032237681315));
#27532=CARTESIAN_POINT('',(109.655721927456,280.,-34.5032237681315));
#27533=CARTESIAN_POINT('',(127.968500624638,280.,-37.1752157277839));
#27534=CARTESIAN_POINT('',(111.508973864096,280.,-20.6047255475076));
#27535=CARTESIAN_POINT('',(128.273548427401,280.,-37.9151793916432));
#27536=CARTESIAN_POINT('Origin',(127.223548427401,280.,-37.9151793916432));
#27537=CARTESIAN_POINT('',(128.273548427401,280.,-39.4187321117283));
#27538=CARTESIAN_POINT('',(128.273548427401,280.,-18.9575896958216));
#27539=CARTESIAN_POINT('',(127.971127263844,280.,-40.1560420081102));
#27540=CARTESIAN_POINT('Origin',(127.223548427401,280.,-39.4187321117283));
#27541=CARTESIAN_POINT('',(127.333356762198,280.,-40.8026951072716));
#27542=CARTESIAN_POINT('',(132.211452368059,280.,-35.85665945119));
#27543=CARTESIAN_POINT('',(126.997701127708,280.,-41.3560806824536));
#27544=CARTESIAN_POINT('Origin',(128.330128544122,280.,-41.785774969114));
#27545=CARTESIAN_POINT('',(125.328762843953,280.,-42.9220241352404));
#27546=CARTESIAN_POINT('Origin',(124.747780443448,280.,-40.6305041508116));
#27547=CARTESIAN_POINT('',(124.876218876064,280.,-43.5036225521864));
#27548=CARTESIAN_POINT('Origin',(125.476218876064,280.,-43.5036225521863));
#27549=CARTESIAN_POINT('',(124.876218876064,280.,-44.4226470147914));
#27550=CARTESIAN_POINT('',(124.876218876064,280.,-21.751811276093));
#27551=CARTESIAN_POINT('',(125.387243744723,280.,-45.1153516005764));
#27552=CARTESIAN_POINT('Origin',(125.601218876064,280.,-44.4226470147914));
#27553=CARTESIAN_POINT('',(127.036092546462,280.,-46.8112703207193));
#27554=CARTESIAN_POINT('Origin',(124.659008759128,280.,-47.4728765656934));
#27555=CARTESIAN_POINT('',(127.149786002621,280.,-47.007169160326));
#27556=CARTESIAN_POINT('Origin',(127.469614165074,280.,-46.690609613792));
#27557=CARTESIAN_POINT('',(127.637659789347,280.,-47.5000804575095));
#27558=CARTESIAN_POINT('',(109.783194287684,280.,-29.4612597821981));
#27559=CARTESIAN_POINT('',(116.046321988033,280.,-47.5000804575095));
#27560=CARTESIAN_POINT('',(142.398712869122,280.,-40.8026951072716));
#27561=CARTESIAN_POINT('Origin',(141.401941087198,280.,-41.7857749691141));
#27562=CARTESIAN_POINT('',(141.760942367476,280.,-40.1560420081102));
#27563=CARTESIAN_POINT('',(122.844278695199,280.,-20.9759150534898));
#27564=CARTESIAN_POINT('',(141.458521203919,280.,-39.4187321117283));
#27565=CARTESIAN_POINT('Origin',(142.508521203919,280.,-39.4187321117283));
#27566=CARTESIAN_POINT('',(141.458521203919,280.,-37.9151793916432));
#27567=CARTESIAN_POINT('',(141.45852120392,280.,-19.7093660558643));
#27568=CARTESIAN_POINT('',(141.763569006683,280.,-37.1752157277839));
#27569=CARTESIAN_POINT('Origin',(142.508521203919,280.,-37.9151793916432));
#27570=CARTESIAN_POINT('',(144.417668112103,280.,-34.5032237681314));
#27571=CARTESIAN_POINT('',(141.792684822546,280.,-37.1459036249592));
#27572=CARTESIAN_POINT('',(154.875609963127,280.,-34.5032237681314));
#27573=CARTESIAN_POINT('',(124.436326149411,280.,-34.5032237681314));
#27574=CARTESIAN_POINT('',(156.375609963127,280.,-36.0032237681314));
#27575=CARTESIAN_POINT('',(133.644647576992,280.,-13.2722613819965));
#27576=CARTESIAN_POINT('',(156.375609963127,280.,-18.0016118840657));
#27577=CARTESIAN_POINT('Origin',(113.356459668193,255.,-46.4955106076453));
#27578=CARTESIAN_POINT('',(112.858666378114,255.,-46.9933038977248));
#27579=CARTESIAN_POINT('',(113.356459668193,255.,-46.4955106076453));
#27580=CARTESIAN_POINT('Origin',(112.858666378114,255.,-46.9933038977248));
#27581=CARTESIAN_POINT('',(112.858666378113,255.,-58.9996518063507));
#27582=CARTESIAN_POINT('Origin',(112.858666378113,255.,-58.9996518063507));
#27583=CARTESIAN_POINT('',(113.858666378113,255.,-59.9996518063507));
#27584=CARTESIAN_POINT('Origin',(113.858666378113,255.,-59.9996518063507));
#27585=CARTESIAN_POINT('',(122.862905683347,255.,-59.9996518063507));
#27586=CARTESIAN_POINT('',(121.37128360059,270.562970493524,-59.9996518063507));
#27587=CARTESIAN_POINT('Origin',(118.37128360059,270.562970493524,-59.9996518063507));
#27588=CARTESIAN_POINT('',(121.37128360059,238.562970493524,-59.9996518063507));
#27589=CARTESIAN_POINT('Origin',(118.37128360059,238.562970493524,-59.9996518063507));
#27590=CARTESIAN_POINT('Origin',(124.265819387872,255.,-61.6506638626042));
#27591=CARTESIAN_POINT('Origin',(151.37128360059,238.562970493524,-59.9996518063507));
#27592=CARTESIAN_POINT('',(154.37128360059,238.562970493524,-34.5032237681314));
#27593=CARTESIAN_POINT('',(154.37128360059,238.562970493524,-59.9996518063507));
#27594=CARTESIAN_POINT('Origin',(151.37128360059,238.562970493524,-34.5032237681314));
#27595=CARTESIAN_POINT('Origin',(118.37128360059,238.562970493524,-59.9996518063507));
#27596=CARTESIAN_POINT('',(121.37128360059,238.562970493524,-34.5032237681315));
#27597=CARTESIAN_POINT('',(121.37128360059,238.562970493524,-59.9996518063507));
#27598=CARTESIAN_POINT('Origin',(118.37128360059,238.562970493524,-34.5032237681315));
#27599=CARTESIAN_POINT('Origin',(151.37128360059,270.562970493524,-59.9996518063507));
#27600=CARTESIAN_POINT('',(154.37128360059,270.562970493524,-34.5032237681314));
#27601=CARTESIAN_POINT('',(154.37128360059,270.562970493524,-59.9996518063507));
#27602=CARTESIAN_POINT('Origin',(151.37128360059,270.562970493524,-34.5032237681314));
#27603=CARTESIAN_POINT('Origin',(118.37128360059,270.562970493524,-59.9996518063507));
#27604=CARTESIAN_POINT('',(121.37128360059,270.562970493524,-34.5032237681315));
#27605=CARTESIAN_POINT('',(121.37128360059,270.562970493524,-59.9996518063507));
#27606=CARTESIAN_POINT('Origin',(118.37128360059,270.562970493524,-34.5032237681315));
#27607=CARTESIAN_POINT('Origin',(156.375609963127,255.,-36.0032237681314));
#27608=CARTESIAN_POINT('',(156.375609963127,255.,-36.0032237681314));
#27609=CARTESIAN_POINT('Origin',(154.875609963127,255.,-34.5032237681314));
#27610=CARTESIAN_POINT('',(154.875609963127,255.,-34.5032237681314));
#27611=CARTESIAN_POINT('Origin',(144.417668112103,255.,-34.5032237681314));
#27612=CARTESIAN_POINT('',(144.417668112103,255.,-34.5032237681314));
#27613=CARTESIAN_POINT('Origin',(141.763569006683,255.,-37.1752157277839));
#27614=CARTESIAN_POINT('',(141.763569006683,255.,-37.1752157277839));
#27615=CARTESIAN_POINT('Origin',(142.508521203919,255.,-37.9151793916432));
#27616=CARTESIAN_POINT('',(141.458521203919,255.,-37.9151793916432));
#27617=CARTESIAN_POINT('Origin',(141.458521203919,255.,-39.4187321117283));
#27618=CARTESIAN_POINT('',(141.458521203919,255.,-39.4187321117283));
#27619=CARTESIAN_POINT('Origin',(142.508521203919,255.,-39.4187321117283));
#27620=CARTESIAN_POINT('',(141.760942367476,255.,-40.1560420081102));
#27621=CARTESIAN_POINT('Origin',(142.398712869122,255.,-40.8026951072716));
#27622=CARTESIAN_POINT('',(142.398712869122,255.,-40.8026951072716));
#27623=CARTESIAN_POINT('Origin',(141.401941087198,255.,-41.7857749691141));
#27624=CARTESIAN_POINT('Origin',(113.356459668193,255.,-58.0910625167937));
#27625=CARTESIAN_POINT('',(113.356459668193,255.,-36.0032237681315));
#27626=CARTESIAN_POINT('Origin',(113.356459668193,255.,-36.0032237681315));
#27627=CARTESIAN_POINT('',(114.856459668193,255.,-34.5032237681315));
#27628=CARTESIAN_POINT('Origin',(114.856459668193,255.,-34.5032237681315));
#27629=CARTESIAN_POINT('',(125.314401519217,255.,-34.5032237681315));
#27630=CARTESIAN_POINT('Origin',(125.314401519217,255.,-34.5032237681315));
#27631=CARTESIAN_POINT('',(127.968500624638,255.,-37.1752157277839));
#27632=CARTESIAN_POINT('Origin',(127.223548427401,255.,-37.9151793916432));
#27633=CARTESIAN_POINT('',(128.273548427401,255.,-37.9151793916432));
#27634=CARTESIAN_POINT('Origin',(128.273548427401,255.,-37.9151793916432));
#27635=CARTESIAN_POINT('',(128.273548427401,255.,-39.4187321117283));
#27636=CARTESIAN_POINT('Origin',(127.223548427401,255.,-39.4187321117283));
#27637=CARTESIAN_POINT('',(127.971127263844,255.,-40.1560420081102));
#27638=CARTESIAN_POINT('Origin',(127.971127263844,255.,-40.1560420081102));
#27639=CARTESIAN_POINT('',(127.333356762198,255.,-40.8026951072716));
#27640=CARTESIAN_POINT('Origin',(128.330128544122,255.,-41.785774969114));
#27641=CARTESIAN_POINT('',(126.997701127708,255.,-41.3560806824536));
#27642=CARTESIAN_POINT('Origin',(124.747780443448,255.,-40.6305041508116));
#27643=CARTESIAN_POINT('',(125.328762843953,255.,-42.9220241352404));
#27644=CARTESIAN_POINT('Origin',(125.476218876064,255.,-43.5036225521863));
#27645=CARTESIAN_POINT('',(124.876218876064,255.,-43.5036225521864));
#27646=CARTESIAN_POINT('Origin',(124.876218876064,255.,-43.5036225521864));
#27647=CARTESIAN_POINT('',(124.876218876064,255.,-44.4226470147914));
#27648=CARTESIAN_POINT('Origin',(125.601218876064,255.,-44.4226470147914));
#27649=CARTESIAN_POINT('',(125.387243744723,255.,-45.1153516005764));
#27650=CARTESIAN_POINT('Origin',(124.659008759128,255.,-47.4728765656934));
#27651=CARTESIAN_POINT('',(127.036092546462,255.,-46.8112703207193));
#27652=CARTESIAN_POINT('Origin',(127.469614165074,255.,-46.690609613792));
#27653=CARTESIAN_POINT('',(127.149786002621,255.,-47.007169160326));
#27654=CARTESIAN_POINT('Origin',(127.149786002621,255.,-47.007169160326));
#27655=CARTESIAN_POINT('',(127.637659789347,255.,-47.5000804575095));
#27656=CARTESIAN_POINT('Origin',(127.637659789347,255.,-47.5000804575095));
#27657=CARTESIAN_POINT('Origin',(141.401941087198,255.,-41.7857749691141));
#27658=CARTESIAN_POINT('',(142.734368503612,280.,-41.3560806824536));
#27659=CARTESIAN_POINT('',(142.398712869122,280.,-40.8026951072716));
#27660=CARTESIAN_POINT('Origin',(141.401941087198,280.,-41.7857749691141));
#27661=CARTESIAN_POINT('',(142.398712869122,294.,-40.8026951072716));
#27662=CARTESIAN_POINT('',(142.398712869122,255.,-40.8026951072716));
#27663=CARTESIAN_POINT('',(142.734368503612,294.,-41.3560806824536));
#27664=CARTESIAN_POINT('Origin',(141.401941087198,294.,-41.7857749691141));
#27665=CARTESIAN_POINT('',(142.734368503612,255.,-41.3560806824536));
#27666=CARTESIAN_POINT('Origin',(142.398712869122,255.,-40.8026951072716));
#27667=CARTESIAN_POINT('',(141.760942367476,280.,-40.1560420081102));
#27668=CARTESIAN_POINT('',(122.844278695199,280.,-20.9759150534898));
#27669=CARTESIAN_POINT('',(141.760942367476,294.,-40.1560420081102));
#27670=CARTESIAN_POINT('',(141.760942367476,255.,-40.1560420081102));
#27671=CARTESIAN_POINT('',(141.760942367476,294.,-40.1560420081102));
#27672=CARTESIAN_POINT('Origin',(142.508521203919,255.,-39.4187321117283));
#27673=CARTESIAN_POINT('',(141.458521203919,280.,-39.4187321117283));
#27674=CARTESIAN_POINT('Origin',(142.508521203919,280.,-39.4187321117283));
#27675=CARTESIAN_POINT('',(141.458521203919,294.,-39.4187321117283));
#27676=CARTESIAN_POINT('',(141.458521203919,255.,-39.4187321117283));
#27677=CARTESIAN_POINT('Origin',(142.508521203919,294.,-39.4187321117283));
#27678=CARTESIAN_POINT('Origin',(141.458521203919,255.,-39.4187321117283));
#27679=CARTESIAN_POINT('',(141.458521203919,280.,-37.9151793916432));
#27680=CARTESIAN_POINT('',(141.45852120392,280.,-19.7093660558643));
#27681=CARTESIAN_POINT('',(141.458521203919,294.,-37.9151793916432));
#27682=CARTESIAN_POINT('',(141.458521203919,255.,-37.9151793916432));
#27683=CARTESIAN_POINT('',(141.458521203919,294.,-37.9151793916432));
#27684=CARTESIAN_POINT('Origin',(142.508521203919,255.,-37.9151793916432));
#27685=CARTESIAN_POINT('',(141.763569006683,280.,-37.1752157277839));
#27686=CARTESIAN_POINT('Origin',(142.508521203919,280.,-37.9151793916432));
#27687=CARTESIAN_POINT('',(141.763569006683,294.,-37.1752157277839));
#27688=CARTESIAN_POINT('',(141.763569006683,255.,-37.1752157277839));
#27689=CARTESIAN_POINT('Origin',(142.508521203919,294.,-37.9151793916432));
#27690=CARTESIAN_POINT('Origin',(141.763569006683,255.,-37.1752157277839));
#27691=CARTESIAN_POINT('',(144.417668112103,280.,-34.5032237681314));
#27692=CARTESIAN_POINT('',(141.792684822546,280.,-37.1459036249592));
#27693=CARTESIAN_POINT('',(144.417668112103,294.,-34.5032237681314));
#27694=CARTESIAN_POINT('',(144.417668112103,255.,-34.5032237681314));
#27695=CARTESIAN_POINT('',(144.544688744748,294.,-34.375346814161));
#27696=CARTESIAN_POINT('Origin',(144.417668112103,255.,-34.5032237681314));
#27697=CARTESIAN_POINT('',(154.875609963127,280.,-34.5032237681314));
#27698=CARTESIAN_POINT('',(124.436326149411,280.,-34.5032237681314));
#27699=CARTESIAN_POINT('',(154.875609963127,294.,-34.5032237681314));
#27700=CARTESIAN_POINT('',(154.875609963127,255.,-34.5032237681314));
#27701=CARTESIAN_POINT('',(134.86603481566,294.,-34.5032237681314));
#27702=CARTESIAN_POINT('Origin',(154.875609963127,255.,-34.5032237681314));
#27703=CARTESIAN_POINT('',(156.375609963127,280.,-36.0032237681314));
#27704=CARTESIAN_POINT('',(133.644647576992,280.,-13.2722613819965));
#27705=CARTESIAN_POINT('',(156.375609963127,294.,-36.0032237681314));
#27706=CARTESIAN_POINT('',(156.375609963127,255.,-36.0032237681314));
#27707=CARTESIAN_POINT('',(154.875609963127,294.,-34.5032237681314));
#27708=CARTESIAN_POINT('Origin',(156.375609963127,255.,-58.0910625167936));
#27709=CARTESIAN_POINT('',(155.375609963127,280.,-59.0910625167936));
#27710=CARTESIAN_POINT('',(156.375609963127,280.,-58.0910625167936));
#27711=CARTESIAN_POINT('',(154.960007558403,280.,-59.5066649215182));
#27712=CARTESIAN_POINT('',(155.375609963127,294.,-59.0910625167936));
#27713=CARTESIAN_POINT('',(155.375609963127,255.,-59.0910625167936));
#27714=CARTESIAN_POINT('',(156.375609963127,294.,-58.0910625167936));
#27715=CARTESIAN_POINT('',(156.375609963127,294.,-58.0910625167936));
#27716=CARTESIAN_POINT('',(156.375609963127,255.,-58.0910625167936));
#27717=CARTESIAN_POINT('Origin',(155.375609963127,255.,-59.0910625167936));
#27718=CARTESIAN_POINT('',(114.356459668193,280.,-59.0910625167936));
#27719=CARTESIAN_POINT('',(150.62266449878,280.,-59.0910625167936));
#27720=CARTESIAN_POINT('',(114.356459668193,294.,-59.0910625167936));
#27721=CARTESIAN_POINT('',(114.356459668193,255.,-59.0910625167936));
#27722=CARTESIAN_POINT('',(155.375609963127,294.,-59.0910625167936));
#27723=CARTESIAN_POINT('Origin',(114.356459668193,255.,-59.0910625167936));
#27724=CARTESIAN_POINT('',(113.356459668193,280.,-58.0910625167936));
#27725=CARTESIAN_POINT('',(120.773904182304,280.,-65.5085070309049));
#27726=CARTESIAN_POINT('',(113.356459668193,294.,-58.0910625167937));
#27727=CARTESIAN_POINT('',(113.356459668193,255.,-58.0910625167937));
#27728=CARTESIAN_POINT('',(113.356459668193,294.,-58.0910625167937));
#27729=CARTESIAN_POINT('Origin',(113.356459668193,255.,-58.0910625167937));
#27730=CARTESIAN_POINT('',(113.356459668193,280.,-36.0032237681315));
#27731=CARTESIAN_POINT('',(113.356459668193,280.,-29.0455312583968));
#27732=CARTESIAN_POINT('',(113.356459668193,294.,-36.0032237681315));
#27733=CARTESIAN_POINT('',(113.356459668193,255.,-36.0032237681315));
#27734=CARTESIAN_POINT('',(113.356459668193,294.,-36.0032237681315));
#27735=CARTESIAN_POINT('Origin',(113.356459668193,255.,-36.0032237681315));
#27736=CARTESIAN_POINT('',(114.856459668193,280.,-34.5032237681315));
#27737=CARTESIAN_POINT('',(120.131896739857,280.,-29.2277866964671));
#27738=CARTESIAN_POINT('',(114.856459668193,294.,-34.5032237681315));
#27739=CARTESIAN_POINT('',(114.856459668193,255.,-34.5032237681315));
#27740=CARTESIAN_POINT('',(114.856459668193,294.,-34.5032237681315));
#27741=CARTESIAN_POINT('Origin',(114.856459668193,255.,-34.5032237681315));
#27742=CARTESIAN_POINT('',(125.314401519217,280.,-34.5032237681315));
#27743=CARTESIAN_POINT('',(109.655721927456,280.,-34.5032237681315));
#27744=CARTESIAN_POINT('',(125.314401519217,294.,-34.5032237681315));
#27745=CARTESIAN_POINT('',(125.314401519217,255.,-34.5032237681315));
#27746=CARTESIAN_POINT('',(134.86603481566,294.,-34.5032237681314));
#27747=CARTESIAN_POINT('Origin',(125.314401519217,255.,-34.5032237681315));
#27748=CARTESIAN_POINT('',(127.968500624638,280.,-37.1752157277839));
#27749=CARTESIAN_POINT('',(111.508973864096,280.,-20.6047255475076));
#27750=CARTESIAN_POINT('',(127.968500624638,294.,-37.1752157277839));
#27751=CARTESIAN_POINT('',(127.968500624638,255.,-37.1752157277839));
#27752=CARTESIAN_POINT('',(127.968500624638,294.,-37.1752157277839));
#27753=CARTESIAN_POINT('Origin',(127.223548427401,255.,-37.9151793916432));
#27754=CARTESIAN_POINT('',(128.273548427401,280.,-37.9151793916432));
#27755=CARTESIAN_POINT('Origin',(127.223548427401,280.,-37.9151793916432));
#27756=CARTESIAN_POINT('',(128.273548427401,294.,-37.9151793916432));
#27757=CARTESIAN_POINT('',(128.273548427401,255.,-37.9151793916432));
#27758=CARTESIAN_POINT('Origin',(127.223548427401,294.,-37.9151793916432));
#27759=CARTESIAN_POINT('Origin',(134.86603481566,294.,-46.7971431424625));
#27760=CARTESIAN_POINT('',(127.971127263844,294.,-40.1560420081102));
#27761=CARTESIAN_POINT('',(128.273548427401,294.,-39.4187321117283));
#27762=CARTESIAN_POINT('Origin',(127.223548427401,294.,-39.4187321117283));
#27763=CARTESIAN_POINT('',(127.333356762198,294.,-40.8026951072716));
#27764=CARTESIAN_POINT('',(127.333356762198,294.,-40.8026951072716));
#27765=CARTESIAN_POINT('',(126.997701127708,294.,-41.3560806824536));
#27766=CARTESIAN_POINT('Origin',(128.330128544122,294.,-41.785774969114));
#27767=CARTESIAN_POINT('',(125.328762843953,294.,-42.9220241352404));
#27768=CARTESIAN_POINT('Origin',(124.747780443448,294.,-40.6305041508116));
#27769=CARTESIAN_POINT('',(124.876218876064,294.,-43.5036225521864));
#27770=CARTESIAN_POINT('Origin',(125.476218876064,294.,-43.5036225521863));
#27771=CARTESIAN_POINT('',(124.876218876064,294.,-44.4226470147914));
#27772=CARTESIAN_POINT('',(124.876218876064,294.,-44.4226470147914));
#27773=CARTESIAN_POINT('',(125.387243744723,294.,-45.1153516005764));
#27774=CARTESIAN_POINT('Origin',(125.601218876064,294.,-44.4226470147914));
#27775=CARTESIAN_POINT('',(127.036092546462,294.,-46.8112703207193));
#27776=CARTESIAN_POINT('Origin',(124.659008759128,294.,-47.4728765656934));
#27777=CARTESIAN_POINT('',(127.149786002621,294.,-47.007169160326));
#27778=CARTESIAN_POINT('Origin',(127.469614165074,294.,-46.690609613792));
#27779=CARTESIAN_POINT('',(127.637659789347,294.,-47.5000804575095));
#27780=CARTESIAN_POINT('',(127.637659789347,294.,-47.5000804575095));
#27781=CARTESIAN_POINT('',(142.094409841973,294.,-47.5000804575095));
#27782=CARTESIAN_POINT('',(142.094409841973,294.,-47.5000804575095));
#27783=CARTESIAN_POINT('',(142.5822836287,294.,-47.007169160326));
#27784=CARTESIAN_POINT('',(142.5822836287,294.,-47.007169160326));
#27785=CARTESIAN_POINT('',(142.695977084858,294.,-46.8112703207193));
#27786=CARTESIAN_POINT('Origin',(142.262455466246,294.,-46.690609613792));
#27787=CARTESIAN_POINT('',(144.344825886597,294.,-45.1153516005764));
#27788=CARTESIAN_POINT('Origin',(145.073060872192,294.,-47.4728765656934));
#27789=CARTESIAN_POINT('',(144.855850755256,294.,-44.4226470147914));
#27790=CARTESIAN_POINT('Origin',(144.130850755256,294.,-44.4226470147914));
#27791=CARTESIAN_POINT('',(144.855850755256,294.,-43.5036225521863));
#27792=CARTESIAN_POINT('',(144.855850755256,294.,-43.5036225521863));
#27793=CARTESIAN_POINT('',(144.403306787367,294.,-42.9220241352404));
#27794=CARTESIAN_POINT('Origin',(144.255850755256,294.,-43.5036225521863));
#27795=CARTESIAN_POINT('Origin',(144.984289187872,294.,-40.6305041508117));
#27796=CARTESIAN_POINT('',(156.375609963127,294.,-36.0032237681314));
#27797=CARTESIAN_POINT('',(128.273548427401,294.,-39.4187321117283));
#27798=CARTESIAN_POINT('Origin',(156.375609963127,255.,-36.0032237681314));
#27799=CARTESIAN_POINT('',(156.375609963127,280.,-18.0016118840657));
#27800=CARTESIAN_POINT('Origin',(128.273548427401,255.,-37.9151793916432));
#27801=CARTESIAN_POINT('',(128.273548427401,280.,-39.4187321117283));
#27802=CARTESIAN_POINT('',(128.273548427401,280.,-18.9575896958216));
#27803=CARTESIAN_POINT('',(128.273548427401,255.,-39.4187321117283));
#27804=CARTESIAN_POINT('Origin',(127.223548427401,255.,-39.4187321117283));
#27805=CARTESIAN_POINT('',(127.971127263844,280.,-40.1560420081102));
#27806=CARTESIAN_POINT('Origin',(127.223548427401,280.,-39.4187321117283));
#27807=CARTESIAN_POINT('',(127.971127263844,255.,-40.1560420081102));
#27808=CARTESIAN_POINT('Origin',(127.971127263844,255.,-40.1560420081102));
#27809=CARTESIAN_POINT('',(127.333356762198,280.,-40.8026951072716));
#27810=CARTESIAN_POINT('',(132.211452368059,280.,-35.85665945119));
#27811=CARTESIAN_POINT('',(127.333356762198,255.,-40.8026951072716));
#27812=CARTESIAN_POINT('Origin',(128.330128544122,255.,-41.785774969114));
#27813=CARTESIAN_POINT('',(126.997701127708,280.,-41.3560806824536));
#27814=CARTESIAN_POINT('Origin',(128.330128544122,280.,-41.785774969114));
#27815=CARTESIAN_POINT('',(126.997701127708,255.,-41.3560806824536));
#27816=CARTESIAN_POINT('Origin',(124.747780443448,255.,-40.6305041508116));
#27817=CARTESIAN_POINT('',(125.328762843953,280.,-42.9220241352404));
#27818=CARTESIAN_POINT('Origin',(124.747780443448,280.,-40.6305041508116));
#27819=CARTESIAN_POINT('',(125.328762843953,255.,-42.9220241352404));
#27820=CARTESIAN_POINT('Origin',(125.476218876064,255.,-43.5036225521863));
#27821=CARTESIAN_POINT('',(124.876218876064,280.,-43.5036225521864));
#27822=CARTESIAN_POINT('Origin',(125.476218876064,280.,-43.5036225521863));
#27823=CARTESIAN_POINT('',(124.876218876064,255.,-43.5036225521864));
#27824=CARTESIAN_POINT('Origin',(124.876218876064,255.,-43.5036225521864));
#27825=CARTESIAN_POINT('',(124.876218876064,280.,-44.4226470147914));
#27826=CARTESIAN_POINT('',(124.876218876064,280.,-21.751811276093));
#27827=CARTESIAN_POINT('',(124.876218876064,255.,-44.4226470147914));
#27828=CARTESIAN_POINT('Origin',(125.601218876064,255.,-44.4226470147914));
#27829=CARTESIAN_POINT('',(125.387243744723,280.,-45.1153516005764));
#27830=CARTESIAN_POINT('Origin',(125.601218876064,280.,-44.4226470147914));
#27831=CARTESIAN_POINT('',(125.387243744723,255.,-45.1153516005764));
#27832=CARTESIAN_POINT('Origin',(124.659008759128,255.,-47.4728765656934));
#27833=CARTESIAN_POINT('',(127.036092546462,280.,-46.8112703207193));
#27834=CARTESIAN_POINT('Origin',(124.659008759128,280.,-47.4728765656934));
#27835=CARTESIAN_POINT('',(127.036092546462,255.,-46.8112703207193));
#27836=CARTESIAN_POINT('Origin',(127.469614165074,255.,-46.690609613792));
#27837=CARTESIAN_POINT('',(127.149786002621,280.,-47.007169160326));
#27838=CARTESIAN_POINT('Origin',(127.469614165074,280.,-46.690609613792));
#27839=CARTESIAN_POINT('',(127.149786002621,255.,-47.007169160326));
#27840=CARTESIAN_POINT('Origin',(127.149786002621,255.,-47.007169160326));
#27841=CARTESIAN_POINT('',(127.637659789347,280.,-47.5000804575095));
#27842=CARTESIAN_POINT('',(109.783194287684,280.,-29.4612597821981));
#27843=CARTESIAN_POINT('',(127.637659789347,255.,-47.5000804575095));
#27844=CARTESIAN_POINT('Origin',(127.637659789347,255.,-47.5000804575095));
#27845=CARTESIAN_POINT('',(142.094409841973,280.,-47.5000804575095));
#27846=CARTESIAN_POINT('',(116.046321988033,280.,-47.5000804575095));
#27847=CARTESIAN_POINT('',(142.094409841973,255.,-47.5000804575095));
#27848=CARTESIAN_POINT('Origin',(142.094409841973,255.,-47.5000804575095));
#27849=CARTESIAN_POINT('',(142.5822836287,280.,-47.007169160326));
#27850=CARTESIAN_POINT('',(144.655606318974,280.,-44.9124385054979));
#27851=CARTESIAN_POINT('',(142.5822836287,255.,-47.007169160326));
#27852=CARTESIAN_POINT('Origin',(142.262455466246,255.,-46.690609613792));
#27853=CARTESIAN_POINT('',(142.695977084858,280.,-46.8112703207193));
#27854=CARTESIAN_POINT('Origin',(142.262455466246,280.,-46.690609613792));
#27855=CARTESIAN_POINT('',(142.695977084858,255.,-46.8112703207193));
#27856=CARTESIAN_POINT('Origin',(145.073060872192,255.,-47.4728765656934));
#27857=CARTESIAN_POINT('',(144.344825886597,280.,-45.1153516005764));
#27858=CARTESIAN_POINT('Origin',(145.073060872192,280.,-47.4728765656934));
#27859=CARTESIAN_POINT('',(144.344825886597,255.,-45.1153516005764));
#27860=CARTESIAN_POINT('Origin',(144.130850755256,255.,-44.4226470147914));
#27861=CARTESIAN_POINT('',(144.855850755256,280.,-44.4226470147914));
#27862=CARTESIAN_POINT('Origin',(144.130850755256,280.,-44.4226470147914));
#27863=CARTESIAN_POINT('',(144.855850755256,255.,-44.4226470147914));
#27864=CARTESIAN_POINT('Origin',(144.855850755256,255.,-44.4226470147914));
#27865=CARTESIAN_POINT('',(144.855850755256,280.,-43.5036225521863));
#27866=CARTESIAN_POINT('',(144.855850755256,280.,-22.2113235073957));
#27867=CARTESIAN_POINT('',(144.855850755256,255.,-43.5036225521863));
#27868=CARTESIAN_POINT('Origin',(144.255850755256,255.,-43.5036225521863));
#27869=CARTESIAN_POINT('',(144.403306787367,280.,-42.9220241352404));
#27870=CARTESIAN_POINT('Origin',(144.255850755256,280.,-43.5036225521863));
#27871=CARTESIAN_POINT('',(144.403306787367,255.,-42.9220241352404));
#27872=CARTESIAN_POINT('Origin',(144.984289187872,255.,-40.6305041508117));
#27873=CARTESIAN_POINT('Origin',(144.984289187872,280.,-40.6305041508117));
#27874=CARTESIAN_POINT('Origin',(104.454984186719,280.,0.));
#27875=CARTESIAN_POINT('',(0.,0.,0.));
#27876=CARTESIAN_POINT('Origin',(103.778785519041,230.,0.));
#27877=CARTESIAN_POINT('',(113.356459668193,230.,58.0910625167936));
#27878=CARTESIAN_POINT('',(113.356459668193,230.,36.0032237681315));
#27879=CARTESIAN_POINT('',(113.356459668193,230.,29.0455312583968));
#27880=CARTESIAN_POINT('',(114.356459668193,230.,59.0910625167936));
#27881=CARTESIAN_POINT('',(120.773904182304,230.,65.5085070309049));
#27882=CARTESIAN_POINT('',(155.375609963127,230.,59.0910625167936));
#27883=CARTESIAN_POINT('',(150.62266449878,230.,59.0910625167936));
#27884=CARTESIAN_POINT('',(156.375609963127,230.,58.0910625167936));
#27885=CARTESIAN_POINT('',(154.960007558403,230.,59.5066649215182));
#27886=CARTESIAN_POINT('',(156.375609963127,230.,36.0032237681314));
#27887=CARTESIAN_POINT('',(156.375609963127,230.,18.0016118840657));
#27888=CARTESIAN_POINT('',(154.875609963127,230.,34.5032237681314));
#27889=CARTESIAN_POINT('',(133.475597910073,230.,13.1032117150771));
#27890=CARTESIAN_POINT('',(144.417668112103,230.,34.5032237681314));
#27891=CARTESIAN_POINT('',(124.098226815572,230.,34.5032237681314));
#27892=CARTESIAN_POINT('',(141.763569006683,230.,37.1752157277839));
#27893=CARTESIAN_POINT('',(141.62477097808,230.,37.3149494761148));
#27894=CARTESIAN_POINT('',(141.458521203919,230.,37.9151793916432));
#27895=CARTESIAN_POINT('Origin',(142.508521203919,230.,37.9151793916432));
#27896=CARTESIAN_POINT('',(141.458521203919,230.,39.4187321117283));
#27897=CARTESIAN_POINT('',(141.45852120392,230.,19.7093660558644));
#27898=CARTESIAN_POINT('',(141.760942367476,230.,40.1560420081102));
#27899=CARTESIAN_POINT('Origin',(142.508521203919,230.,39.4187321117283));
#27900=CARTESIAN_POINT('',(142.398712869122,230.,40.8026951072716));
#27901=CARTESIAN_POINT('',(122.677567086127,230.,20.8068815557118));
#27902=CARTESIAN_POINT('',(142.734368503612,230.,41.3560806824536));
#27903=CARTESIAN_POINT('Origin',(141.401941087198,230.,41.7857749691141));
#27904=CARTESIAN_POINT('',(144.403306787367,230.,42.9220241352404));
#27905=CARTESIAN_POINT('Origin',(144.984289187872,230.,40.6305041508117));
#27906=CARTESIAN_POINT('',(144.855850755256,230.,43.5036225521863));
#27907=CARTESIAN_POINT('Origin',(144.255850755256,230.,43.5036225521863));
#27908=CARTESIAN_POINT('',(144.855850755256,230.,44.4226470147914));
#27909=CARTESIAN_POINT('',(144.855850755256,230.,22.2113235073957));
#27910=CARTESIAN_POINT('',(144.344825886597,230.,45.1153516005764));
#27911=CARTESIAN_POINT('Origin',(144.130850755256,230.,44.4226470147914));
#27912=CARTESIAN_POINT('',(142.695977084858,230.,46.8112703207193));
#27913=CARTESIAN_POINT('Origin',(145.073060872192,230.,47.4728765656934));
#27914=CARTESIAN_POINT('',(142.5822836287,230.,47.007169160326));
#27915=CARTESIAN_POINT('Origin',(142.262455466246,230.,46.690609613792));
#27916=CARTESIAN_POINT('',(142.094409841973,230.,47.5000804575095));
#27917=CARTESIAN_POINT('',(144.48829315277,230.,45.0814792533986));
#27918=CARTESIAN_POINT('',(127.637659789347,230.,47.5000804575095));
#27919=CARTESIAN_POINT('',(115.708222654194,230.,47.5000804575095));
#27920=CARTESIAN_POINT('',(127.149786002621,230.,47.007169160326));
#27921=CARTESIAN_POINT('',(109.61588112148,230.,29.2922190342974));
#27922=CARTESIAN_POINT('',(127.036092546462,230.,46.8112703207193));
#27923=CARTESIAN_POINT('Origin',(127.469614165074,230.,46.690609613792));
#27924=CARTESIAN_POINT('',(125.387243744723,230.,45.1153516005764));
#27925=CARTESIAN_POINT('Origin',(124.659008759128,230.,47.4728765656934));
#27926=CARTESIAN_POINT('',(124.876218876064,230.,44.4226470147914));
#27927=CARTESIAN_POINT('Origin',(125.601218876064,230.,44.4226470147914));
#27928=CARTESIAN_POINT('',(124.876218876064,230.,43.5036225521864));
#27929=CARTESIAN_POINT('',(124.876218876064,230.,21.751811276093));
#27930=CARTESIAN_POINT('',(125.328762843953,230.,42.9220241352404));
#27931=CARTESIAN_POINT('Origin',(125.476218876064,230.,43.5036225521863));
#27932=CARTESIAN_POINT('',(126.997701127708,230.,41.3560806824536));
#27933=CARTESIAN_POINT('Origin',(124.747780443448,230.,40.6305041508116));
#27934=CARTESIAN_POINT('',(127.333356762198,230.,40.8026951072716));
#27935=CARTESIAN_POINT('Origin',(128.330128544122,230.,41.785774969114));
#27936=CARTESIAN_POINT('',(127.971127263844,230.,40.1560420081102));
#27937=CARTESIAN_POINT('',(132.044740758987,230.,36.025692948968));
#27938=CARTESIAN_POINT('',(128.273548427401,230.,39.4187321117283));
#27939=CARTESIAN_POINT('Origin',(127.223548427401,230.,39.4187321117283));
#27940=CARTESIAN_POINT('',(128.273548427401,230.,37.9151793916432));
#27941=CARTESIAN_POINT('',(128.273548427401,230.,18.9575896958216));
#27942=CARTESIAN_POINT('',(127.968500624638,230.,37.1752157277839));
#27943=CARTESIAN_POINT('Origin',(127.223548427401,230.,37.9151793916432));
#27944=CARTESIAN_POINT('',(125.314401519217,230.,34.5032237681315));
#27945=CARTESIAN_POINT('',(111.34106001963,230.,20.435679696352));
#27946=CARTESIAN_POINT('',(114.856459668193,230.,34.5032237681315));
#27947=CARTESIAN_POINT('',(109.317622593617,230.,34.5032237681315));
#27948=CARTESIAN_POINT('',(119.962847072938,230.,29.3968363633866));
#27949=CARTESIAN_POINT('Origin',(142.094409841973,255.,47.5000804575095));
#27950=CARTESIAN_POINT('',(142.5822836287,216.,47.007169160326));
#27951=CARTESIAN_POINT('',(142.5822836287,255.,47.007169160326));
#27952=CARTESIAN_POINT('',(142.094409841973,216.,47.5000804575095));
#27953=CARTESIAN_POINT('',(142.5822836287,216.,47.007169160326));
#27954=CARTESIAN_POINT('',(142.094409841973,255.,47.5000804575095));
#27955=CARTESIAN_POINT('Origin',(142.262455466246,255.,46.690609613792));
#27956=CARTESIAN_POINT('',(142.695977084858,216.,46.8112703207193));
#27957=CARTESIAN_POINT('',(142.695977084858,255.,46.8112703207193));
#27958=CARTESIAN_POINT('Origin',(142.262455466246,216.,46.690609613792));
#27959=CARTESIAN_POINT('Origin',(145.073060872192,255.,47.4728765656934));
#27960=CARTESIAN_POINT('',(144.344825886597,216.,45.1153516005764));
#27961=CARTESIAN_POINT('',(144.344825886597,255.,45.1153516005764));
#27962=CARTESIAN_POINT('Origin',(145.073060872192,216.,47.4728765656934));
#27963=CARTESIAN_POINT('Origin',(144.130850755256,255.,44.4226470147914));
#27964=CARTESIAN_POINT('',(144.855850755256,216.,44.4226470147914));
#27965=CARTESIAN_POINT('',(144.855850755256,255.,44.4226470147914));
#27966=CARTESIAN_POINT('Origin',(144.130850755256,216.,44.4226470147914));
#27967=CARTESIAN_POINT('Origin',(144.855850755256,255.,44.4226470147914));
#27968=CARTESIAN_POINT('',(144.855850755256,216.,43.5036225521863));
#27969=CARTESIAN_POINT('',(144.855850755256,255.,43.5036225521863));
#27970=CARTESIAN_POINT('',(144.855850755256,216.,43.5036225521863));
#27971=CARTESIAN_POINT('Origin',(144.255850755256,255.,43.5036225521863));
#27972=CARTESIAN_POINT('',(144.403306787367,216.,42.9220241352404));
#27973=CARTESIAN_POINT('',(144.403306787367,255.,42.9220241352404));
#27974=CARTESIAN_POINT('Origin',(144.255850755256,216.,43.5036225521863));
#27975=CARTESIAN_POINT('Origin',(144.984289187872,255.,40.6305041508117));
#27976=CARTESIAN_POINT('',(142.734368503612,216.,41.3560806824536));
#27977=CARTESIAN_POINT('',(142.734368503612,255.,41.3560806824536));
#27978=CARTESIAN_POINT('Origin',(144.984289187872,216.,40.6305041508117));
#27979=CARTESIAN_POINT('Origin',(141.401941087198,255.,41.7857749691141));
#27980=CARTESIAN_POINT('',(142.398712869122,216.,40.8026951072716));
#27981=CARTESIAN_POINT('',(142.398712869122,255.,40.8026951072716));
#27982=CARTESIAN_POINT('Origin',(141.401941087198,216.,41.7857749691141));
#27983=CARTESIAN_POINT('Origin',(142.398712869122,255.,40.8026951072716));
#27984=CARTESIAN_POINT('',(141.760942367476,216.,40.1560420081102));
#27985=CARTESIAN_POINT('',(141.760942367476,255.,40.1560420081102));
#27986=CARTESIAN_POINT('',(141.760942367476,216.,40.1560420081102));
#27987=CARTESIAN_POINT('Origin',(142.508521203919,255.,39.4187321117283));
#27988=CARTESIAN_POINT('',(141.458521203919,216.,39.4187321117283));
#27989=CARTESIAN_POINT('',(141.458521203919,255.,39.4187321117283));
#27990=CARTESIAN_POINT('Origin',(142.508521203919,216.,39.4187321117283));
#27991=CARTESIAN_POINT('Origin',(141.458521203919,255.,39.4187321117283));
#27992=CARTESIAN_POINT('',(141.458521203919,216.,37.9151793916432));
#27993=CARTESIAN_POINT('',(141.458521203919,255.,37.9151793916432));
#27994=CARTESIAN_POINT('',(141.458521203919,216.,37.9151793916432));
#27995=CARTESIAN_POINT('Origin',(142.508521203919,255.,37.9151793916432));
#27996=CARTESIAN_POINT('',(141.763569006683,216.,37.1752157277839));
#27997=CARTESIAN_POINT('',(141.763569006683,255.,37.1752157277839));
#27998=CARTESIAN_POINT('Origin',(142.508521203919,216.,37.9151793916432));
#27999=CARTESIAN_POINT('Origin',(141.763569006683,255.,37.1752157277839));
#28000=CARTESIAN_POINT('',(144.417668112103,216.,34.5032237681314));
#28001=CARTESIAN_POINT('',(144.417668112103,255.,34.5032237681314));
#28002=CARTESIAN_POINT('',(144.544688744748,216.,34.375346814161));
#28003=CARTESIAN_POINT('Origin',(144.417668112103,255.,34.5032237681314));
#28004=CARTESIAN_POINT('',(154.875609963127,216.,34.5032237681314));
#28005=CARTESIAN_POINT('',(154.875609963127,255.,34.5032237681314));
#28006=CARTESIAN_POINT('',(134.86603481566,216.,34.5032237681314));
#28007=CARTESIAN_POINT('Origin',(154.875609963127,255.,34.5032237681314));
#28008=CARTESIAN_POINT('',(156.375609963127,216.,36.0032237681314));
#28009=CARTESIAN_POINT('',(156.375609963127,255.,36.0032237681314));
#28010=CARTESIAN_POINT('',(154.875609963127,216.,34.5032237681314));
#28011=CARTESIAN_POINT('Origin',(156.375609963127,255.,36.0032237681314));
#28012=CARTESIAN_POINT('',(156.375609963127,216.,58.0910625167936));
#28013=CARTESIAN_POINT('',(156.375609963127,255.,58.0910625167936));
#28014=CARTESIAN_POINT('',(156.375609963127,216.,36.0032237681314));
#28015=CARTESIAN_POINT('Origin',(113.356459668193,255.,58.0910625167937));
#28016=CARTESIAN_POINT('',(113.356459668193,216.,36.0032237681315));
#28017=CARTESIAN_POINT('',(113.356459668193,255.,36.0032237681315));
#28018=CARTESIAN_POINT('',(113.356459668193,216.,58.0910625167937));
#28019=CARTESIAN_POINT('',(113.356459668193,216.,36.0032237681315));
#28020=CARTESIAN_POINT('',(113.356459668193,255.,58.0910625167937));
#28021=CARTESIAN_POINT('Origin',(113.356459668193,255.,36.0032237681315));
#28022=CARTESIAN_POINT('',(114.856459668193,216.,34.5032237681315));
#28023=CARTESIAN_POINT('',(114.856459668193,255.,34.5032237681315));
#28024=CARTESIAN_POINT('',(114.856459668193,216.,34.5032237681315));
#28025=CARTESIAN_POINT('Origin',(114.856459668193,255.,34.5032237681315));
#28026=CARTESIAN_POINT('',(125.314401519217,216.,34.5032237681315));
#28027=CARTESIAN_POINT('',(125.314401519217,255.,34.5032237681315));
#28028=CARTESIAN_POINT('',(134.86603481566,216.,34.5032237681314));
#28029=CARTESIAN_POINT('Origin',(125.314401519217,255.,34.5032237681315));
#28030=CARTESIAN_POINT('',(127.968500624638,216.,37.1752157277839));
#28031=CARTESIAN_POINT('',(127.968500624638,255.,37.1752157277839));
#28032=CARTESIAN_POINT('',(127.968500624638,216.,37.1752157277839));
#28033=CARTESIAN_POINT('Origin',(127.223548427401,255.,37.9151793916432));
#28034=CARTESIAN_POINT('',(128.273548427401,216.,37.9151793916432));
#28035=CARTESIAN_POINT('',(128.273548427401,255.,37.9151793916432));
#28036=CARTESIAN_POINT('Origin',(127.223548427401,216.,37.9151793916432));
#28037=CARTESIAN_POINT('Origin',(156.375609963127,255.,58.0910625167936));
#28038=CARTESIAN_POINT('',(155.375609963127,216.,59.0910625167936));
#28039=CARTESIAN_POINT('',(155.375609963127,255.,59.0910625167936));
#28040=CARTESIAN_POINT('',(156.375609963127,216.,58.0910625167936));
#28041=CARTESIAN_POINT('Origin',(155.375609963127,255.,59.0910625167936));
#28042=CARTESIAN_POINT('',(114.356459668193,216.,59.0910625167936));
#28043=CARTESIAN_POINT('',(114.356459668193,255.,59.0910625167936));
#28044=CARTESIAN_POINT('',(155.375609963127,216.,59.0910625167936));
#28045=CARTESIAN_POINT('Origin',(114.356459668193,255.,59.0910625167936));
#28046=CARTESIAN_POINT('',(113.356459668193,216.,58.0910625167937));
#28047=CARTESIAN_POINT('Origin',(128.273548427401,255.,37.9151793916432));
#28048=CARTESIAN_POINT('',(128.273548427401,216.,39.4187321117283));
#28049=CARTESIAN_POINT('',(128.273548427401,255.,39.4187321117283));
#28050=CARTESIAN_POINT('',(128.273548427401,216.,39.4187321117283));
#28051=CARTESIAN_POINT('Origin',(127.637659789347,255.,47.5000804575095));
#28052=CARTESIAN_POINT('',(127.637659789347,216.,47.5000804575095));
#28053=CARTESIAN_POINT('',(142.094409841973,216.,47.5000804575095));
#28054=CARTESIAN_POINT('',(127.637659789347,255.,47.5000804575095));
#28055=CARTESIAN_POINT('Origin',(127.149786002621,255.,47.007169160326));
#28056=CARTESIAN_POINT('',(127.149786002621,216.,47.007169160326));
#28057=CARTESIAN_POINT('',(127.637659789347,216.,47.5000804575095));
#28058=CARTESIAN_POINT('',(127.149786002621,255.,47.007169160326));
#28059=CARTESIAN_POINT('Origin',(127.469614165074,255.,46.690609613792));
#28060=CARTESIAN_POINT('',(127.036092546462,216.,46.8112703207193));
#28061=CARTESIAN_POINT('Origin',(127.469614165074,216.,46.690609613792));
#28062=CARTESIAN_POINT('',(127.036092546462,255.,46.8112703207193));
#28063=CARTESIAN_POINT('Origin',(124.659008759128,255.,47.4728765656934));
#28064=CARTESIAN_POINT('',(125.387243744723,216.,45.1153516005764));
#28065=CARTESIAN_POINT('Origin',(124.659008759128,216.,47.4728765656934));
#28066=CARTESIAN_POINT('',(125.387243744723,255.,45.1153516005764));
#28067=CARTESIAN_POINT('Origin',(125.601218876064,255.,44.4226470147914));
#28068=CARTESIAN_POINT('',(124.876218876064,216.,44.4226470147914));
#28069=CARTESIAN_POINT('Origin',(125.601218876064,216.,44.4226470147914));
#28070=CARTESIAN_POINT('',(124.876218876064,255.,44.4226470147914));
#28071=CARTESIAN_POINT('Origin',(124.876218876064,255.,43.5036225521864));
#28072=CARTESIAN_POINT('',(124.876218876064,216.,43.5036225521864));
#28073=CARTESIAN_POINT('',(124.876218876064,216.,44.4226470147914));
#28074=CARTESIAN_POINT('',(124.876218876064,255.,43.5036225521864));
#28075=CARTESIAN_POINT('Origin',(125.476218876064,255.,43.5036225521863));
#28076=CARTESIAN_POINT('',(125.328762843953,216.,42.9220241352404));
#28077=CARTESIAN_POINT('Origin',(125.476218876064,216.,43.5036225521863));
#28078=CARTESIAN_POINT('',(125.328762843953,255.,42.9220241352404));
#28079=CARTESIAN_POINT('Origin',(124.747780443448,255.,40.6305041508116));
#28080=CARTESIAN_POINT('',(126.997701127708,216.,41.3560806824536));
#28081=CARTESIAN_POINT('Origin',(124.747780443448,216.,40.6305041508116));
#28082=CARTESIAN_POINT('',(126.997701127708,255.,41.3560806824536));
#28083=CARTESIAN_POINT('Origin',(128.330128544122,255.,41.785774969114));
#28084=CARTESIAN_POINT('',(127.333356762198,216.,40.8026951072716));
#28085=CARTESIAN_POINT('Origin',(128.330128544122,216.,41.785774969114));
#28086=CARTESIAN_POINT('',(127.333356762198,255.,40.8026951072716));
#28087=CARTESIAN_POINT('Origin',(127.971127263844,255.,40.1560420081102));
#28088=CARTESIAN_POINT('',(127.971127263844,216.,40.1560420081102));
#28089=CARTESIAN_POINT('',(127.333356762198,216.,40.8026951072716));
#28090=CARTESIAN_POINT('',(127.971127263844,255.,40.1560420081102));
#28091=CARTESIAN_POINT('Origin',(127.223548427401,255.,39.4187321117283));
#28092=CARTESIAN_POINT('Origin',(127.223548427401,216.,39.4187321117283));
#28093=CARTESIAN_POINT('Origin',(134.86603481566,216.,46.7971431424625));
#28094=CARTESIAN_POINT('Origin',(142.094409841973,255.,47.5000804575095));
#28095=CARTESIAN_POINT('',(142.094409841973,230.,47.5000804575095));
#28096=CARTESIAN_POINT('',(142.5822836287,230.,47.007169160326));
#28097=CARTESIAN_POINT('',(144.48829315277,230.,45.0814792533986));
#28098=CARTESIAN_POINT('',(142.094409841973,280.,47.5000804575095));
#28099=CARTESIAN_POINT('',(142.094409841973,255.,47.5000804575095));
#28100=CARTESIAN_POINT('',(142.5822836287,280.,47.007169160326));
#28101=CARTESIAN_POINT('',(144.655606318974,280.,44.9124385054979));
#28102=CARTESIAN_POINT('',(142.5822836287,255.,47.007169160326));
#28103=CARTESIAN_POINT('Origin',(142.262455466246,255.,46.690609613792));
#28104=CARTESIAN_POINT('',(142.695977084858,230.,46.8112703207193));
#28105=CARTESIAN_POINT('Origin',(142.262455466246,230.,46.690609613792));
#28106=CARTESIAN_POINT('',(142.695977084858,280.,46.8112703207193));
#28107=CARTESIAN_POINT('Origin',(142.262455466246,280.,46.690609613792));
#28108=CARTESIAN_POINT('',(142.695977084858,255.,46.8112703207193));
#28109=CARTESIAN_POINT('Origin',(145.073060872192,255.,47.4728765656934));
#28110=CARTESIAN_POINT('',(144.344825886597,230.,45.1153516005764));
#28111=CARTESIAN_POINT('Origin',(145.073060872192,230.,47.4728765656934));
#28112=CARTESIAN_POINT('',(144.344825886597,280.,45.1153516005764));
#28113=CARTESIAN_POINT('Origin',(145.073060872192,280.,47.4728765656934));
#28114=CARTESIAN_POINT('',(144.344825886597,255.,45.1153516005764));
#28115=CARTESIAN_POINT('Origin',(144.130850755256,255.,44.4226470147914));
#28116=CARTESIAN_POINT('',(144.855850755256,230.,44.4226470147914));
#28117=CARTESIAN_POINT('Origin',(144.130850755256,230.,44.4226470147914));
#28118=CARTESIAN_POINT('',(144.855850755256,280.,44.4226470147914));
#28119=CARTESIAN_POINT('Origin',(144.130850755256,280.,44.4226470147914));
#28120=CARTESIAN_POINT('',(144.855850755256,255.,44.4226470147914));
#28121=CARTESIAN_POINT('Origin',(144.855850755256,255.,44.4226470147914));
#28122=CARTESIAN_POINT('',(144.855850755256,230.,43.5036225521863));
#28123=CARTESIAN_POINT('',(144.855850755256,230.,22.2113235073957));
#28124=CARTESIAN_POINT('',(144.855850755256,280.,43.5036225521863));
#28125=CARTESIAN_POINT('',(144.855850755256,280.,22.2113235073957));
#28126=CARTESIAN_POINT('',(144.855850755256,255.,43.5036225521863));
#28127=CARTESIAN_POINT('Origin',(144.255850755256,255.,43.5036225521863));
#28128=CARTESIAN_POINT('',(144.403306787367,230.,42.9220241352404));
#28129=CARTESIAN_POINT('Origin',(144.255850755256,230.,43.5036225521863));
#28130=CARTESIAN_POINT('',(144.403306787367,280.,42.9220241352404));
#28131=CARTESIAN_POINT('Origin',(144.255850755256,280.,43.5036225521863));
#28132=CARTESIAN_POINT('',(144.403306787367,255.,42.9220241352404));
#28133=CARTESIAN_POINT('Origin',(144.984289187872,255.,40.6305041508117));
#28134=CARTESIAN_POINT('',(142.734368503612,230.,41.3560806824536));
#28135=CARTESIAN_POINT('Origin',(144.984289187872,230.,40.6305041508117));
#28136=CARTESIAN_POINT('',(142.734368503612,280.,41.3560806824536));
#28137=CARTESIAN_POINT('Origin',(144.984289187872,280.,40.6305041508117));
#28138=CARTESIAN_POINT('',(142.734368503612,255.,41.3560806824536));
#28139=CARTESIAN_POINT('Origin',(145.869719034433,230.,53.247581206998));
#28140=CARTESIAN_POINT('',(156.375609963127,230.,46.4955106076453));
#28141=CARTESIAN_POINT('',(156.873403253207,230.,46.9933038977248));
#28142=CARTESIAN_POINT('',(156.373403253207,230.,46.4933038977248));
#28143=CARTESIAN_POINT('',(156.873403253207,230.,58.9996518063507));
#28144=CARTESIAN_POINT('',(156.873403253207,230.,46.9933038977248));
#28145=CARTESIAN_POINT('',(155.873403253207,230.,59.9996518063507));
#28146=CARTESIAN_POINT('',(156.873403253207,230.,58.9996518063507));
#28147=CARTESIAN_POINT('',(146.869163947974,230.,59.9996518063508));
#28148=CARTESIAN_POINT('',(155.873403253207,230.,59.9996518063507));
#28149=CARTESIAN_POINT('',(145.466250243448,230.,59.4840979918677));
#28150=CARTESIAN_POINT('Origin',(145.466250243448,230.,61.6506638626042));
#28151=CARTESIAN_POINT('',(124.265819387872,230.,59.4840979918677));
#28152=CARTESIAN_POINT('',(145.466250243448,230.,59.4840979918677));
#28153=CARTESIAN_POINT('',(122.862905683347,230.,59.9996518063507));
#28154=CARTESIAN_POINT('Origin',(124.265819387872,230.,61.6506638626042));
#28155=CARTESIAN_POINT('',(113.858666378113,230.,59.9996518063507));
#28156=CARTESIAN_POINT('',(113.858666378113,230.,59.9996518063507));
#28157=CARTESIAN_POINT('',(112.858666378113,230.,58.9996518063507));
#28158=CARTESIAN_POINT('',(112.858666378113,230.,58.9996518063507));
#28159=CARTESIAN_POINT('',(112.858666378114,230.,46.9933038977248));
#28160=CARTESIAN_POINT('',(112.858666378114,230.,46.9933038977248));
#28161=CARTESIAN_POINT('',(113.356459668193,230.,46.4955106076453));
#28162=CARTESIAN_POINT('',(113.358666378114,230.,46.4933038977248));
#28163=CARTESIAN_POINT('',(113.356459668193,230.,36.0032237681315));
#28164=CARTESIAN_POINT('',(113.356459668193,230.,29.0455312583968));
#28165=CARTESIAN_POINT('',(114.856459668193,230.,34.5032237681315));
#28166=CARTESIAN_POINT('',(119.962847072938,230.,29.3968363633866));
#28167=CARTESIAN_POINT('',(125.314401519217,230.,34.5032237681315));
#28168=CARTESIAN_POINT('',(109.317622593617,230.,34.5032237681315));
#28169=CARTESIAN_POINT('',(127.968500624638,230.,37.1752157277839));
#28170=CARTESIAN_POINT('',(111.34106001963,230.,20.435679696352));
#28171=CARTESIAN_POINT('',(128.273548427401,230.,37.9151793916432));
#28172=CARTESIAN_POINT('Origin',(127.223548427401,230.,37.9151793916432));
#28173=CARTESIAN_POINT('',(128.273548427401,230.,39.4187321117283));
#28174=CARTESIAN_POINT('',(128.273548427401,230.,18.9575896958216));
#28175=CARTESIAN_POINT('',(127.971127263844,230.,40.1560420081102));
#28176=CARTESIAN_POINT('Origin',(127.223548427401,230.,39.4187321117283));
#28177=CARTESIAN_POINT('',(127.333356762198,230.,40.8026951072716));
#28178=CARTESIAN_POINT('',(132.044740758987,230.,36.025692948968));
#28179=CARTESIAN_POINT('',(126.997701127708,230.,41.3560806824536));
#28180=CARTESIAN_POINT('Origin',(128.330128544122,230.,41.785774969114));
#28181=CARTESIAN_POINT('',(125.328762843953,230.,42.9220241352404));
#28182=CARTESIAN_POINT('Origin',(124.747780443448,230.,40.6305041508116));
#28183=CARTESIAN_POINT('',(124.876218876064,230.,43.5036225521864));
#28184=CARTESIAN_POINT('Origin',(125.476218876064,230.,43.5036225521863));
#28185=CARTESIAN_POINT('',(124.876218876064,230.,44.4226470147914));
#28186=CARTESIAN_POINT('',(124.876218876064,230.,21.751811276093));
#28187=CARTESIAN_POINT('',(125.387243744723,230.,45.1153516005764));
#28188=CARTESIAN_POINT('Origin',(125.601218876064,230.,44.4226470147914));
#28189=CARTESIAN_POINT('',(127.036092546462,230.,46.8112703207193));
#28190=CARTESIAN_POINT('Origin',(124.659008759128,230.,47.4728765656934));
#28191=CARTESIAN_POINT('',(127.149786002621,230.,47.007169160326));
#28192=CARTESIAN_POINT('Origin',(127.469614165074,230.,46.690609613792));
#28193=CARTESIAN_POINT('',(127.637659789347,230.,47.5000804575095));
#28194=CARTESIAN_POINT('',(109.61588112148,230.,29.2922190342974));
#28195=CARTESIAN_POINT('',(115.708222654194,230.,47.5000804575095));
#28196=CARTESIAN_POINT('',(142.398712869122,230.,40.8026951072716));
#28197=CARTESIAN_POINT('Origin',(141.401941087198,230.,41.7857749691141));
#28198=CARTESIAN_POINT('',(141.760942367476,230.,40.1560420081102));
#28199=CARTESIAN_POINT('',(122.677567086127,230.,20.8068815557118));
#28200=CARTESIAN_POINT('',(141.458521203919,230.,39.4187321117283));
#28201=CARTESIAN_POINT('Origin',(142.508521203919,230.,39.4187321117283));
#28202=CARTESIAN_POINT('',(141.458521203919,230.,37.9151793916432));
#28203=CARTESIAN_POINT('',(141.45852120392,230.,19.7093660558644));
#28204=CARTESIAN_POINT('',(141.763569006683,230.,37.1752157277839));
#28205=CARTESIAN_POINT('Origin',(142.508521203919,230.,37.9151793916432));
#28206=CARTESIAN_POINT('',(144.417668112103,230.,34.5032237681314));
#28207=CARTESIAN_POINT('',(141.62477097808,230.,37.3149494761148));
#28208=CARTESIAN_POINT('',(154.875609963127,230.,34.5032237681314));
#28209=CARTESIAN_POINT('',(124.098226815572,230.,34.5032237681314));
#28210=CARTESIAN_POINT('',(156.375609963127,230.,36.0032237681314));
#28211=CARTESIAN_POINT('',(133.475597910073,230.,13.1032117150771));
#28212=CARTESIAN_POINT('',(156.375609963127,230.,18.0016118840657));
#28213=CARTESIAN_POINT('Origin',(156.375609963127,255.,46.4955106076453));
#28214=CARTESIAN_POINT('',(156.873403253207,280.,46.9933038977248));
#28215=CARTESIAN_POINT('',(156.873403253207,255.,46.9933038977248));
#28216=CARTESIAN_POINT('',(156.375609963127,280.,46.4955106076453));
#28217=CARTESIAN_POINT('',(156.375609963127,255.,46.4955106076453));
#28218=CARTESIAN_POINT('',(156.373403253207,280.,46.4933038977248));
#28219=CARTESIAN_POINT('Origin',(156.873403253207,255.,46.9933038977248));
#28220=CARTESIAN_POINT('',(156.873403253207,280.,58.9996518063507));
#28221=CARTESIAN_POINT('',(156.873403253207,255.,58.9996518063507));
#28222=CARTESIAN_POINT('',(156.873403253207,280.,46.9933038977248));
#28223=CARTESIAN_POINT('Origin',(156.873403253207,255.,58.9996518063507));
#28224=CARTESIAN_POINT('',(155.873403253207,280.,59.9996518063507));
#28225=CARTESIAN_POINT('',(155.873403253207,255.,59.9996518063507));
#28226=CARTESIAN_POINT('',(156.873403253207,280.,58.9996518063507));
#28227=CARTESIAN_POINT('Origin',(155.873403253207,255.,59.9996518063507));
#28228=CARTESIAN_POINT('',(146.869163947974,280.,59.9996518063508));
#28229=CARTESIAN_POINT('',(146.869163947974,255.,59.9996518063508));
#28230=CARTESIAN_POINT('',(155.873403253207,280.,59.9996518063507));
#28231=CARTESIAN_POINT('',(154.37128360059,270.562970493524,59.9996518063507));
#28232=CARTESIAN_POINT('Origin',(151.37128360059,270.562970493524,59.9996518063507));
#28233=CARTESIAN_POINT('',(154.37128360059,238.562970493524,59.9996518063507));
#28234=CARTESIAN_POINT('Origin',(151.37128360059,238.562970493524,59.9996518063507));
#28235=CARTESIAN_POINT('Origin',(145.466250243448,255.,61.6506638626042));
#28236=CARTESIAN_POINT('',(145.466250243448,280.,59.4840979918677));
#28237=CARTESIAN_POINT('',(145.466250243448,255.,59.4840979918677));
#28238=CARTESIAN_POINT('Origin',(145.466250243448,280.,61.6506638626042));
#28239=CARTESIAN_POINT('Origin',(145.466250243448,255.,59.4840979918677));
#28240=CARTESIAN_POINT('',(124.265819387872,280.,59.4840979918677));
#28241=CARTESIAN_POINT('',(124.265819387872,280.,59.4840979918677));
#28242=CARTESIAN_POINT('',(124.265819387872,255.,59.4840979918677));
#28243=CARTESIAN_POINT('Origin',(145.869719034433,280.,53.247581206998));
#28244=CARTESIAN_POINT('',(156.375609963127,280.,36.0032237681314));
#28245=CARTESIAN_POINT('',(156.375609963127,280.,18.0016118840657));
#28246=CARTESIAN_POINT('',(154.875609963127,280.,34.5032237681314));
#28247=CARTESIAN_POINT('',(133.644647576992,280.,13.2722613819965));
#28248=CARTESIAN_POINT('',(144.417668112103,280.,34.5032237681314));
#28249=CARTESIAN_POINT('',(124.436326149411,280.,34.5032237681314));
#28250=CARTESIAN_POINT('',(141.763569006683,280.,37.1752157277839));
#28251=CARTESIAN_POINT('',(141.792684822546,280.,37.1459036249592));
#28252=CARTESIAN_POINT('',(141.458521203919,280.,37.9151793916432));
#28253=CARTESIAN_POINT('Origin',(142.508521203919,280.,37.9151793916432));
#28254=CARTESIAN_POINT('',(141.458521203919,280.,39.4187321117283));
#28255=CARTESIAN_POINT('',(141.45852120392,280.,19.7093660558643));
#28256=CARTESIAN_POINT('',(141.760942367476,280.,40.1560420081102));
#28257=CARTESIAN_POINT('Origin',(142.508521203919,280.,39.4187321117283));
#28258=CARTESIAN_POINT('',(142.398712869122,280.,40.8026951072716));
#28259=CARTESIAN_POINT('',(122.844278695199,280.,20.9759150534898));
#28260=CARTESIAN_POINT('Origin',(141.401941087198,280.,41.7857749691141));
#28261=CARTESIAN_POINT('',(127.637659789347,280.,47.5000804575095));
#28262=CARTESIAN_POINT('',(116.046321988033,280.,47.5000804575095));
#28263=CARTESIAN_POINT('',(127.149786002621,280.,47.007169160326));
#28264=CARTESIAN_POINT('',(109.783194287684,280.,29.4612597821981));
#28265=CARTESIAN_POINT('',(127.036092546462,280.,46.8112703207193));
#28266=CARTESIAN_POINT('Origin',(127.469614165074,280.,46.690609613792));
#28267=CARTESIAN_POINT('',(125.387243744723,280.,45.1153516005764));
#28268=CARTESIAN_POINT('Origin',(124.659008759128,280.,47.4728765656934));
#28269=CARTESIAN_POINT('',(124.876218876064,280.,44.4226470147914));
#28270=CARTESIAN_POINT('Origin',(125.601218876064,280.,44.4226470147914));
#28271=CARTESIAN_POINT('',(124.876218876064,280.,43.5036225521864));
#28272=CARTESIAN_POINT('',(124.876218876064,280.,21.751811276093));
#28273=CARTESIAN_POINT('',(125.328762843953,280.,42.9220241352404));
#28274=CARTESIAN_POINT('Origin',(125.476218876064,280.,43.5036225521863));
#28275=CARTESIAN_POINT('',(126.997701127708,280.,41.3560806824536));
#28276=CARTESIAN_POINT('Origin',(124.747780443448,280.,40.6305041508116));
#28277=CARTESIAN_POINT('',(127.333356762198,280.,40.8026951072716));
#28278=CARTESIAN_POINT('Origin',(128.330128544122,280.,41.785774969114));
#28279=CARTESIAN_POINT('',(127.971127263844,280.,40.1560420081102));
#28280=CARTESIAN_POINT('',(132.211452368059,280.,35.85665945119));
#28281=CARTESIAN_POINT('',(128.273548427401,280.,39.4187321117283));
#28282=CARTESIAN_POINT('Origin',(127.223548427401,280.,39.4187321117283));
#28283=CARTESIAN_POINT('',(128.273548427401,280.,37.9151793916432));
#28284=CARTESIAN_POINT('',(128.273548427401,280.,18.9575896958216));
#28285=CARTESIAN_POINT('',(127.968500624638,280.,37.1752157277839));
#28286=CARTESIAN_POINT('Origin',(127.223548427401,280.,37.9151793916432));
#28287=CARTESIAN_POINT('',(125.314401519217,280.,34.5032237681315));
#28288=CARTESIAN_POINT('',(111.508973864096,280.,20.6047255475076));
#28289=CARTESIAN_POINT('',(114.856459668193,280.,34.5032237681315));
#28290=CARTESIAN_POINT('',(109.655721927456,280.,34.5032237681315));
#28291=CARTESIAN_POINT('',(113.356459668193,280.,36.0032237681315));
#28292=CARTESIAN_POINT('',(120.131896739857,280.,29.2277866964671));
#28293=CARTESIAN_POINT('',(113.356459668193,280.,46.4955106076453));
#28294=CARTESIAN_POINT('',(113.356459668193,280.,29.0455312583968));
#28295=CARTESIAN_POINT('',(112.858666378114,280.,46.9933038977248));
#28296=CARTESIAN_POINT('',(113.358666378114,280.,46.4933038977248));
#28297=CARTESIAN_POINT('',(112.858666378113,280.,58.9996518063507));
#28298=CARTESIAN_POINT('',(112.858666378114,280.,46.9933038977248));
#28299=CARTESIAN_POINT('',(113.858666378113,280.,59.9996518063507));
#28300=CARTESIAN_POINT('',(112.858666378113,280.,58.9996518063507));
#28301=CARTESIAN_POINT('',(122.862905683347,280.,59.9996518063507));
#28302=CARTESIAN_POINT('',(113.858666378113,280.,59.9996518063507));
#28303=CARTESIAN_POINT('Origin',(124.265819387872,280.,61.6506638626042));
#28304=CARTESIAN_POINT('Origin',(113.356459668193,255.,46.4955106076453));
#28305=CARTESIAN_POINT('',(112.858666378114,255.,46.9933038977248));
#28306=CARTESIAN_POINT('',(113.356459668193,255.,46.4955106076453));
#28307=CARTESIAN_POINT('Origin',(112.858666378114,255.,46.9933038977248));
#28308=CARTESIAN_POINT('',(112.858666378113,255.,58.9996518063507));
#28309=CARTESIAN_POINT('Origin',(112.858666378113,255.,58.9996518063507));
#28310=CARTESIAN_POINT('',(113.858666378113,255.,59.9996518063507));
#28311=CARTESIAN_POINT('Origin',(113.858666378113,255.,59.9996518063507));
#28312=CARTESIAN_POINT('',(122.862905683347,255.,59.9996518063507));
#28313=CARTESIAN_POINT('',(121.37128360059,270.562970493524,59.9996518063507));
#28314=CARTESIAN_POINT('Origin',(118.37128360059,270.562970493524,59.9996518063507));
#28315=CARTESIAN_POINT('',(121.37128360059,238.562970493524,59.9996518063507));
#28316=CARTESIAN_POINT('Origin',(118.37128360059,238.562970493524,59.9996518063507));
#28317=CARTESIAN_POINT('Origin',(124.265819387872,255.,61.6506638626042));
#28318=CARTESIAN_POINT('Origin',(151.37128360059,238.562970493524,59.9996518063507));
#28319=CARTESIAN_POINT('',(154.37128360059,238.562970493524,34.5032237681314));
#28320=CARTESIAN_POINT('',(154.37128360059,238.562970493524,59.9996518063507));
#28321=CARTESIAN_POINT('Origin',(151.37128360059,238.562970493524,34.5032237681314));
#28322=CARTESIAN_POINT('Origin',(118.37128360059,238.562970493524,59.9996518063507));
#28323=CARTESIAN_POINT('',(121.37128360059,238.562970493524,34.5032237681315));
#28324=CARTESIAN_POINT('',(121.37128360059,238.562970493524,59.9996518063507));
#28325=CARTESIAN_POINT('Origin',(118.37128360059,238.562970493524,34.5032237681315));
#28326=CARTESIAN_POINT('Origin',(151.37128360059,270.562970493524,59.9996518063507));
#28327=CARTESIAN_POINT('',(154.37128360059,270.562970493524,34.5032237681314));
#28328=CARTESIAN_POINT('',(154.37128360059,270.562970493524,59.9996518063507));
#28329=CARTESIAN_POINT('Origin',(151.37128360059,270.562970493524,34.5032237681314));
#28330=CARTESIAN_POINT('Origin',(118.37128360059,270.562970493524,59.9996518063507));
#28331=CARTESIAN_POINT('',(121.37128360059,270.562970493524,34.5032237681315));
#28332=CARTESIAN_POINT('',(121.37128360059,270.562970493524,59.9996518063507));
#28333=CARTESIAN_POINT('Origin',(118.37128360059,270.562970493524,34.5032237681315));
#28334=CARTESIAN_POINT('Origin',(156.375609963127,255.,36.0032237681314));
#28335=CARTESIAN_POINT('',(156.375609963127,255.,36.0032237681314));
#28336=CARTESIAN_POINT('Origin',(154.875609963127,255.,34.5032237681314));
#28337=CARTESIAN_POINT('',(154.875609963127,255.,34.5032237681314));
#28338=CARTESIAN_POINT('Origin',(144.417668112103,255.,34.5032237681314));
#28339=CARTESIAN_POINT('',(144.417668112103,255.,34.5032237681314));
#28340=CARTESIAN_POINT('Origin',(141.763569006683,255.,37.1752157277839));
#28341=CARTESIAN_POINT('',(141.763569006683,255.,37.1752157277839));
#28342=CARTESIAN_POINT('Origin',(142.508521203919,255.,37.9151793916432));
#28343=CARTESIAN_POINT('',(141.458521203919,255.,37.9151793916432));
#28344=CARTESIAN_POINT('Origin',(141.458521203919,255.,39.4187321117283));
#28345=CARTESIAN_POINT('',(141.458521203919,255.,39.4187321117283));
#28346=CARTESIAN_POINT('Origin',(142.508521203919,255.,39.4187321117283));
#28347=CARTESIAN_POINT('',(141.760942367476,255.,40.1560420081102));
#28348=CARTESIAN_POINT('Origin',(142.398712869122,255.,40.8026951072716));
#28349=CARTESIAN_POINT('',(142.398712869122,255.,40.8026951072716));
#28350=CARTESIAN_POINT('Origin',(141.401941087198,255.,41.7857749691141));
#28351=CARTESIAN_POINT('Origin',(113.356459668193,255.,58.0910625167937));
#28352=CARTESIAN_POINT('',(113.356459668193,255.,36.0032237681315));
#28353=CARTESIAN_POINT('Origin',(113.356459668193,255.,36.0032237681315));
#28354=CARTESIAN_POINT('',(114.856459668193,255.,34.5032237681315));
#28355=CARTESIAN_POINT('Origin',(114.856459668193,255.,34.5032237681315));
#28356=CARTESIAN_POINT('',(125.314401519217,255.,34.5032237681315));
#28357=CARTESIAN_POINT('Origin',(125.314401519217,255.,34.5032237681315));
#28358=CARTESIAN_POINT('',(127.968500624638,255.,37.1752157277839));
#28359=CARTESIAN_POINT('Origin',(127.223548427401,255.,37.9151793916432));
#28360=CARTESIAN_POINT('',(128.273548427401,255.,37.9151793916432));
#28361=CARTESIAN_POINT('Origin',(128.273548427401,255.,37.9151793916432));
#28362=CARTESIAN_POINT('',(128.273548427401,255.,39.4187321117283));
#28363=CARTESIAN_POINT('Origin',(127.223548427401,255.,39.4187321117283));
#28364=CARTESIAN_POINT('',(127.971127263844,255.,40.1560420081102));
#28365=CARTESIAN_POINT('Origin',(127.971127263844,255.,40.1560420081102));
#28366=CARTESIAN_POINT('',(127.333356762198,255.,40.8026951072716));
#28367=CARTESIAN_POINT('Origin',(128.330128544122,255.,41.785774969114));
#28368=CARTESIAN_POINT('',(126.997701127708,255.,41.3560806824536));
#28369=CARTESIAN_POINT('Origin',(124.747780443448,255.,40.6305041508116));
#28370=CARTESIAN_POINT('',(125.328762843953,255.,42.9220241352404));
#28371=CARTESIAN_POINT('Origin',(125.476218876064,255.,43.5036225521863));
#28372=CARTESIAN_POINT('',(124.876218876064,255.,43.5036225521864));
#28373=CARTESIAN_POINT('Origin',(124.876218876064,255.,43.5036225521864));
#28374=CARTESIAN_POINT('',(124.876218876064,255.,44.4226470147914));
#28375=CARTESIAN_POINT('Origin',(125.601218876064,255.,44.4226470147914));
#28376=CARTESIAN_POINT('',(125.387243744723,255.,45.1153516005764));
#28377=CARTESIAN_POINT('Origin',(124.659008759128,255.,47.4728765656934));
#28378=CARTESIAN_POINT('',(127.036092546462,255.,46.8112703207193));
#28379=CARTESIAN_POINT('Origin',(127.469614165074,255.,46.690609613792));
#28380=CARTESIAN_POINT('',(127.149786002621,255.,47.007169160326));
#28381=CARTESIAN_POINT('Origin',(127.149786002621,255.,47.007169160326));
#28382=CARTESIAN_POINT('',(127.637659789347,255.,47.5000804575095));
#28383=CARTESIAN_POINT('Origin',(127.637659789347,255.,47.5000804575095));
#28384=CARTESIAN_POINT('Origin',(141.401941087198,255.,41.7857749691141));
#28385=CARTESIAN_POINT('',(142.734368503612,280.,41.3560806824536));
#28386=CARTESIAN_POINT('',(142.398712869122,280.,40.8026951072716));
#28387=CARTESIAN_POINT('Origin',(141.401941087198,280.,41.7857749691141));
#28388=CARTESIAN_POINT('',(142.734368503612,294.,41.3560806824536));
#28389=CARTESIAN_POINT('',(142.734368503612,255.,41.3560806824536));
#28390=CARTESIAN_POINT('',(142.398712869122,294.,40.8026951072716));
#28391=CARTESIAN_POINT('Origin',(141.401941087198,294.,41.7857749691141));
#28392=CARTESIAN_POINT('',(142.398712869122,255.,40.8026951072716));
#28393=CARTESIAN_POINT('Origin',(142.398712869122,255.,40.8026951072716));
#28394=CARTESIAN_POINT('',(141.760942367476,280.,40.1560420081102));
#28395=CARTESIAN_POINT('',(122.844278695199,280.,20.9759150534898));
#28396=CARTESIAN_POINT('',(141.760942367476,294.,40.1560420081102));
#28397=CARTESIAN_POINT('',(141.760942367476,294.,40.1560420081102));
#28398=CARTESIAN_POINT('',(141.760942367476,255.,40.1560420081102));
#28399=CARTESIAN_POINT('Origin',(142.508521203919,255.,39.4187321117283));
#28400=CARTESIAN_POINT('',(141.458521203919,280.,39.4187321117283));
#28401=CARTESIAN_POINT('Origin',(142.508521203919,280.,39.4187321117283));
#28402=CARTESIAN_POINT('',(141.458521203919,294.,39.4187321117283));
#28403=CARTESIAN_POINT('Origin',(142.508521203919,294.,39.4187321117283));
#28404=CARTESIAN_POINT('',(141.458521203919,255.,39.4187321117283));
#28405=CARTESIAN_POINT('Origin',(141.458521203919,255.,39.4187321117283));
#28406=CARTESIAN_POINT('',(141.458521203919,280.,37.9151793916432));
#28407=CARTESIAN_POINT('',(141.45852120392,280.,19.7093660558643));
#28408=CARTESIAN_POINT('',(141.458521203919,294.,37.9151793916432));
#28409=CARTESIAN_POINT('',(141.458521203919,294.,37.9151793916432));
#28410=CARTESIAN_POINT('',(141.458521203919,255.,37.9151793916432));
#28411=CARTESIAN_POINT('Origin',(142.508521203919,255.,37.9151793916432));
#28412=CARTESIAN_POINT('',(141.763569006683,280.,37.1752157277839));
#28413=CARTESIAN_POINT('Origin',(142.508521203919,280.,37.9151793916432));
#28414=CARTESIAN_POINT('',(141.763569006683,294.,37.1752157277839));
#28415=CARTESIAN_POINT('Origin',(142.508521203919,294.,37.9151793916432));
#28416=CARTESIAN_POINT('',(141.763569006683,255.,37.1752157277839));
#28417=CARTESIAN_POINT('Origin',(141.763569006683,255.,37.1752157277839));
#28418=CARTESIAN_POINT('',(144.417668112103,280.,34.5032237681314));
#28419=CARTESIAN_POINT('',(141.792684822546,280.,37.1459036249592));
#28420=CARTESIAN_POINT('',(144.417668112103,294.,34.5032237681314));
#28421=CARTESIAN_POINT('',(144.544688744748,294.,34.375346814161));
#28422=CARTESIAN_POINT('',(144.417668112103,255.,34.5032237681314));
#28423=CARTESIAN_POINT('Origin',(144.417668112103,255.,34.5032237681314));
#28424=CARTESIAN_POINT('',(154.875609963127,280.,34.5032237681314));
#28425=CARTESIAN_POINT('',(124.436326149411,280.,34.5032237681314));
#28426=CARTESIAN_POINT('',(154.875609963127,294.,34.5032237681314));
#28427=CARTESIAN_POINT('',(134.86603481566,294.,34.5032237681314));
#28428=CARTESIAN_POINT('',(154.875609963127,255.,34.5032237681314));
#28429=CARTESIAN_POINT('Origin',(154.875609963127,255.,34.5032237681314));
#28430=CARTESIAN_POINT('',(156.375609963127,280.,36.0032237681314));
#28431=CARTESIAN_POINT('',(133.644647576992,280.,13.2722613819965));
#28432=CARTESIAN_POINT('',(156.375609963127,294.,36.0032237681314));
#28433=CARTESIAN_POINT('',(154.875609963127,294.,34.5032237681314));
#28434=CARTESIAN_POINT('',(156.375609963127,255.,36.0032237681314));
#28435=CARTESIAN_POINT('Origin',(156.375609963127,255.,58.0910625167936));
#28436=CARTESIAN_POINT('',(155.375609963127,280.,59.0910625167936));
#28437=CARTESIAN_POINT('',(156.375609963127,280.,58.0910625167936));
#28438=CARTESIAN_POINT('',(154.960007558403,280.,59.5066649215182));
#28439=CARTESIAN_POINT('',(156.375609963127,294.,58.0910625167936));
#28440=CARTESIAN_POINT('',(156.375609963127,255.,58.0910625167936));
#28441=CARTESIAN_POINT('',(155.375609963127,294.,59.0910625167936));
#28442=CARTESIAN_POINT('',(156.375609963127,294.,58.0910625167936));
#28443=CARTESIAN_POINT('',(155.375609963127,255.,59.0910625167936));
#28444=CARTESIAN_POINT('Origin',(155.375609963127,255.,59.0910625167936));
#28445=CARTESIAN_POINT('',(114.356459668193,280.,59.0910625167936));
#28446=CARTESIAN_POINT('',(150.62266449878,280.,59.0910625167936));
#28447=CARTESIAN_POINT('',(114.356459668193,294.,59.0910625167936));
#28448=CARTESIAN_POINT('',(155.375609963127,294.,59.0910625167936));
#28449=CARTESIAN_POINT('',(114.356459668193,255.,59.0910625167936));
#28450=CARTESIAN_POINT('Origin',(114.356459668193,255.,59.0910625167936));
#28451=CARTESIAN_POINT('',(113.356459668193,280.,58.0910625167936));
#28452=CARTESIAN_POINT('',(120.773904182304,280.,65.5085070309049));
#28453=CARTESIAN_POINT('',(113.356459668193,294.,58.0910625167937));
#28454=CARTESIAN_POINT('',(113.356459668193,294.,58.0910625167937));
#28455=CARTESIAN_POINT('',(113.356459668193,255.,58.0910625167937));
#28456=CARTESIAN_POINT('Origin',(113.356459668193,255.,58.0910625167937));
#28457=CARTESIAN_POINT('',(113.356459668193,280.,36.0032237681315));
#28458=CARTESIAN_POINT('',(113.356459668193,280.,29.0455312583968));
#28459=CARTESIAN_POINT('',(113.356459668193,294.,36.0032237681315));
#28460=CARTESIAN_POINT('',(113.356459668193,294.,36.0032237681315));
#28461=CARTESIAN_POINT('',(113.356459668193,255.,36.0032237681315));
#28462=CARTESIAN_POINT('Origin',(113.356459668193,255.,36.0032237681315));
#28463=CARTESIAN_POINT('',(114.856459668193,280.,34.5032237681315));
#28464=CARTESIAN_POINT('',(120.131896739857,280.,29.2277866964671));
#28465=CARTESIAN_POINT('',(114.856459668193,294.,34.5032237681315));
#28466=CARTESIAN_POINT('',(114.856459668193,294.,34.5032237681315));
#28467=CARTESIAN_POINT('',(114.856459668193,255.,34.5032237681315));
#28468=CARTESIAN_POINT('Origin',(114.856459668193,255.,34.5032237681315));
#28469=CARTESIAN_POINT('',(125.314401519217,280.,34.5032237681315));
#28470=CARTESIAN_POINT('',(109.655721927456,280.,34.5032237681315));
#28471=CARTESIAN_POINT('',(125.314401519217,294.,34.5032237681315));
#28472=CARTESIAN_POINT('',(134.86603481566,294.,34.5032237681314));
#28473=CARTESIAN_POINT('',(125.314401519217,255.,34.5032237681315));
#28474=CARTESIAN_POINT('Origin',(125.314401519217,255.,34.5032237681315));
#28475=CARTESIAN_POINT('',(127.968500624638,280.,37.1752157277839));
#28476=CARTESIAN_POINT('',(111.508973864096,280.,20.6047255475076));
#28477=CARTESIAN_POINT('',(127.968500624638,294.,37.1752157277839));
#28478=CARTESIAN_POINT('',(127.968500624638,294.,37.1752157277839));
#28479=CARTESIAN_POINT('',(127.968500624638,255.,37.1752157277839));
#28480=CARTESIAN_POINT('Origin',(127.223548427401,255.,37.9151793916432));
#28481=CARTESIAN_POINT('',(128.273548427401,280.,37.9151793916432));
#28482=CARTESIAN_POINT('Origin',(127.223548427401,280.,37.9151793916432));
#28483=CARTESIAN_POINT('',(128.273548427401,294.,37.9151793916432));
#28484=CARTESIAN_POINT('Origin',(127.223548427401,294.,37.9151793916432));
#28485=CARTESIAN_POINT('',(128.273548427401,255.,37.9151793916432));
#28486=CARTESIAN_POINT('Origin',(134.86603481566,294.,46.7971431424625));
#28487=CARTESIAN_POINT('',(127.971127263844,294.,40.1560420081102));
#28488=CARTESIAN_POINT('',(128.273548427401,294.,39.4187321117283));
#28489=CARTESIAN_POINT('Origin',(127.223548427401,294.,39.4187321117283));
#28490=CARTESIAN_POINT('',(128.273548427401,294.,39.4187321117283));
#28491=CARTESIAN_POINT('',(156.375609963127,294.,36.0032237681314));
#28492=CARTESIAN_POINT('',(144.403306787367,294.,42.9220241352404));
#28493=CARTESIAN_POINT('Origin',(144.984289187872,294.,40.6305041508117));
#28494=CARTESIAN_POINT('',(144.855850755256,294.,43.5036225521863));
#28495=CARTESIAN_POINT('Origin',(144.255850755256,294.,43.5036225521863));
#28496=CARTESIAN_POINT('',(144.855850755256,294.,44.4226470147914));
#28497=CARTESIAN_POINT('',(144.855850755256,294.,43.5036225521863));
#28498=CARTESIAN_POINT('',(144.344825886597,294.,45.1153516005764));
#28499=CARTESIAN_POINT('Origin',(144.130850755256,294.,44.4226470147914));
#28500=CARTESIAN_POINT('',(142.695977084858,294.,46.8112703207193));
#28501=CARTESIAN_POINT('Origin',(145.073060872192,294.,47.4728765656934));
#28502=CARTESIAN_POINT('',(142.5822836287,294.,47.007169160326));
#28503=CARTESIAN_POINT('Origin',(142.262455466246,294.,46.690609613792));
#28504=CARTESIAN_POINT('',(142.094409841973,294.,47.5000804575095));
#28505=CARTESIAN_POINT('',(142.5822836287,294.,47.007169160326));
#28506=CARTESIAN_POINT('',(127.637659789347,294.,47.5000804575095));
#28507=CARTESIAN_POINT('',(142.094409841973,294.,47.5000804575095));
#28508=CARTESIAN_POINT('',(127.149786002621,294.,47.007169160326));
#28509=CARTESIAN_POINT('',(127.637659789347,294.,47.5000804575095));
#28510=CARTESIAN_POINT('',(127.036092546462,294.,46.8112703207193));
#28511=CARTESIAN_POINT('Origin',(127.469614165074,294.,46.690609613792));
#28512=CARTESIAN_POINT('',(125.387243744723,294.,45.1153516005764));
#28513=CARTESIAN_POINT('Origin',(124.659008759128,294.,47.4728765656934));
#28514=CARTESIAN_POINT('',(124.876218876064,294.,44.4226470147914));
#28515=CARTESIAN_POINT('Origin',(125.601218876064,294.,44.4226470147914));
#28516=CARTESIAN_POINT('',(124.876218876064,294.,43.5036225521864));
#28517=CARTESIAN_POINT('',(124.876218876064,294.,44.4226470147914));
#28518=CARTESIAN_POINT('',(125.328762843953,294.,42.9220241352404));
#28519=CARTESIAN_POINT('Origin',(125.476218876064,294.,43.5036225521863));
#28520=CARTESIAN_POINT('',(126.997701127708,294.,41.3560806824536));
#28521=CARTESIAN_POINT('Origin',(124.747780443448,294.,40.6305041508116));
#28522=CARTESIAN_POINT('',(127.333356762198,294.,40.8026951072716));
#28523=CARTESIAN_POINT('Origin',(128.330128544122,294.,41.785774969114));
#28524=CARTESIAN_POINT('',(127.333356762198,294.,40.8026951072716));
#28525=CARTESIAN_POINT('Origin',(156.375609963127,255.,36.0032237681314));
#28526=CARTESIAN_POINT('',(156.375609963127,280.,18.0016118840657));
#28527=CARTESIAN_POINT('Origin',(128.273548427401,255.,37.9151793916432));
#28528=CARTESIAN_POINT('',(128.273548427401,280.,39.4187321117283));
#28529=CARTESIAN_POINT('',(128.273548427401,280.,18.9575896958216));
#28530=CARTESIAN_POINT('',(128.273548427401,255.,39.4187321117283));
#28531=CARTESIAN_POINT('Origin',(127.223548427401,255.,39.4187321117283));
#28532=CARTESIAN_POINT('',(127.971127263844,280.,40.1560420081102));
#28533=CARTESIAN_POINT('Origin',(127.223548427401,280.,39.4187321117283));
#28534=CARTESIAN_POINT('',(127.971127263844,255.,40.1560420081102));
#28535=CARTESIAN_POINT('Origin',(127.971127263844,255.,40.1560420081102));
#28536=CARTESIAN_POINT('',(127.333356762198,280.,40.8026951072716));
#28537=CARTESIAN_POINT('',(132.211452368059,280.,35.85665945119));
#28538=CARTESIAN_POINT('',(127.333356762198,255.,40.8026951072716));
#28539=CARTESIAN_POINT('Origin',(128.330128544122,255.,41.785774969114));
#28540=CARTESIAN_POINT('',(126.997701127708,280.,41.3560806824536));
#28541=CARTESIAN_POINT('Origin',(128.330128544122,280.,41.785774969114));
#28542=CARTESIAN_POINT('',(126.997701127708,255.,41.3560806824536));
#28543=CARTESIAN_POINT('Origin',(124.747780443448,255.,40.6305041508116));
#28544=CARTESIAN_POINT('',(125.328762843953,280.,42.9220241352404));
#28545=CARTESIAN_POINT('Origin',(124.747780443448,280.,40.6305041508116));
#28546=CARTESIAN_POINT('',(125.328762843953,255.,42.9220241352404));
#28547=CARTESIAN_POINT('Origin',(125.476218876064,255.,43.5036225521863));
#28548=CARTESIAN_POINT('',(124.876218876064,280.,43.5036225521864));
#28549=CARTESIAN_POINT('Origin',(125.476218876064,280.,43.5036225521863));
#28550=CARTESIAN_POINT('',(124.876218876064,255.,43.5036225521864));
#28551=CARTESIAN_POINT('Origin',(124.876218876064,255.,43.5036225521864));
#28552=CARTESIAN_POINT('',(124.876218876064,280.,44.4226470147914));
#28553=CARTESIAN_POINT('',(124.876218876064,280.,21.751811276093));
#28554=CARTESIAN_POINT('',(124.876218876064,255.,44.4226470147914));
#28555=CARTESIAN_POINT('Origin',(125.601218876064,255.,44.4226470147914));
#28556=CARTESIAN_POINT('',(125.387243744723,280.,45.1153516005764));
#28557=CARTESIAN_POINT('Origin',(125.601218876064,280.,44.4226470147914));
#28558=CARTESIAN_POINT('',(125.387243744723,255.,45.1153516005764));
#28559=CARTESIAN_POINT('Origin',(124.659008759128,255.,47.4728765656934));
#28560=CARTESIAN_POINT('',(127.036092546462,280.,46.8112703207193));
#28561=CARTESIAN_POINT('Origin',(124.659008759128,280.,47.4728765656934));
#28562=CARTESIAN_POINT('',(127.036092546462,255.,46.8112703207193));
#28563=CARTESIAN_POINT('Origin',(127.469614165074,255.,46.690609613792));
#28564=CARTESIAN_POINT('',(127.149786002621,280.,47.007169160326));
#28565=CARTESIAN_POINT('Origin',(127.469614165074,280.,46.690609613792));
#28566=CARTESIAN_POINT('',(127.149786002621,255.,47.007169160326));
#28567=CARTESIAN_POINT('Origin',(127.149786002621,255.,47.007169160326));
#28568=CARTESIAN_POINT('',(127.637659789347,280.,47.5000804575095));
#28569=CARTESIAN_POINT('',(109.783194287684,280.,29.4612597821981));
#28570=CARTESIAN_POINT('',(127.637659789347,255.,47.5000804575095));
#28571=CARTESIAN_POINT('Origin',(127.637659789347,255.,47.5000804575095));
#28572=CARTESIAN_POINT('',(142.094409841973,280.,47.5000804575095));
#28573=CARTESIAN_POINT('',(116.046321988033,280.,47.5000804575095));
#28574=CARTESIAN_POINT('',(142.094409841973,255.,47.5000804575095));
#28575=CARTESIAN_POINT('Origin',(142.094409841973,255.,47.5000804575095));
#28576=CARTESIAN_POINT('',(142.5822836287,280.,47.007169160326));
#28577=CARTESIAN_POINT('',(144.655606318974,280.,44.9124385054979));
#28578=CARTESIAN_POINT('',(142.5822836287,255.,47.007169160326));
#28579=CARTESIAN_POINT('Origin',(142.262455466246,255.,46.690609613792));
#28580=CARTESIAN_POINT('',(142.695977084858,280.,46.8112703207193));
#28581=CARTESIAN_POINT('Origin',(142.262455466246,280.,46.690609613792));
#28582=CARTESIAN_POINT('',(142.695977084858,255.,46.8112703207193));
#28583=CARTESIAN_POINT('Origin',(145.073060872192,255.,47.4728765656934));
#28584=CARTESIAN_POINT('',(144.344825886597,280.,45.1153516005764));
#28585=CARTESIAN_POINT('Origin',(145.073060872192,280.,47.4728765656934));
#28586=CARTESIAN_POINT('',(144.344825886597,255.,45.1153516005764));
#28587=CARTESIAN_POINT('Origin',(144.130850755256,255.,44.4226470147914));
#28588=CARTESIAN_POINT('',(144.855850755256,280.,44.4226470147914));
#28589=CARTESIAN_POINT('Origin',(144.130850755256,280.,44.4226470147914));
#28590=CARTESIAN_POINT('',(144.855850755256,255.,44.4226470147914));
#28591=CARTESIAN_POINT('Origin',(144.855850755256,255.,44.4226470147914));
#28592=CARTESIAN_POINT('',(144.855850755256,280.,43.5036225521863));
#28593=CARTESIAN_POINT('',(144.855850755256,280.,22.2113235073957));
#28594=CARTESIAN_POINT('',(144.855850755256,255.,43.5036225521863));
#28595=CARTESIAN_POINT('Origin',(144.255850755256,255.,43.5036225521863));
#28596=CARTESIAN_POINT('',(144.403306787367,280.,42.9220241352404));
#28597=CARTESIAN_POINT('Origin',(144.255850755256,280.,43.5036225521863));
#28598=CARTESIAN_POINT('',(144.403306787367,255.,42.9220241352404));
#28599=CARTESIAN_POINT('Origin',(144.984289187872,255.,40.6305041508117));
#28600=CARTESIAN_POINT('Origin',(144.984289187872,280.,40.6305041508117));
#28601=CARTESIAN_POINT('Origin',(104.454984186719,280.,0.));
#28602=CARTESIAN_POINT('',(0.,0.,0.));
#28603=CARTESIAN_POINT('Origin',(0.,0.,0.));
#28604=CARTESIAN_POINT('',(8.671875,1.0619983961356E-15,-5.39));
#28605=CARTESIAN_POINT('Origin',(0.,0.,-5.39));
#28606=CARTESIAN_POINT('',(8.671875,1.0619983961356E-15,-4.95));
#28607=CARTESIAN_POINT('',(8.671875,1.0619983961356E-15,0.));
#28608=CARTESIAN_POINT('Origin',(0.,0.,-4.95));
#28609=CARTESIAN_POINT('Origin',(0.,0.,-5.39));
#28610=CARTESIAN_POINT('',(8.781875,1.07546951092622E-15,-5.5));
#28611=CARTESIAN_POINT('Origin',(0.,0.,-5.5));
#28612=CARTESIAN_POINT('Origin',(8.781875,1.07546951092622E-15,-5.39));
#28613=CARTESIAN_POINT('Origin',(0.,0.,-0.10725138426002));
#28614=CARTESIAN_POINT('',(13.0772848379569,1.60150550183421E-15,-4.30142548471451));
#28615=CARTESIAN_POINT('Origin',(0.,0.,-4.30142548471451));
#28616=CARTESIAN_POINT('',(9.6875,1.186376586674E-15,-5.5));
#28617=CARTESIAN_POINT('Origin',(9.6875,1.186376586674E-15,-0.10725138426002));
#28618=CARTESIAN_POINT('Origin',(0.,0.,-5.5));
#28619=CARTESIAN_POINT('Origin',(0.,0.,-3.66302186693758));
#28620=CARTESIAN_POINT('',(13.867180376262,1.69823980609882E-15,-3.66302186693758));
#28621=CARTESIAN_POINT('Origin',(0.,0.,-3.66302186693758));
#28622=CARTESIAN_POINT('',(13.867180376262,1.69823980609882E-15,-3.66302186693758));
#28623=CARTESIAN_POINT('Origin',(0.,0.,-4.22788751277274));
#28624=CARTESIAN_POINT('',(-14.9183171404923,-0.0999999999998437,-4.64446921070048));
#28625=CARTESIAN_POINT('',(-14.9183171404923,0.100000000000156,-4.64446921070048));
#28626=CARTESIAN_POINT('Origin',(0.,0.,-4.64446921070048));
#28627=CARTESIAN_POINT('',(-10.6195538920522,10.4781325358151,-4.64446921070048));
#28628=CARTESIAN_POINT('Origin',(0.,0.,-4.64446921070048));
#28629=CARTESIAN_POINT('',(-10.4781325358149,10.6195538920524,-4.64446921070048));
#28630=CARTESIAN_POINT('Origin',(0.,0.,-4.64446921070048));
#28631=CARTESIAN_POINT('',(-0.0999999999999999,14.9183171404923,-4.64446921070048));
#28632=CARTESIAN_POINT('Origin',(0.,0.,-4.64446921070048));
#28633=CARTESIAN_POINT('',(0.0999999999999999,14.9183171404923,-4.64446921070048));
#28634=CARTESIAN_POINT('Origin',(0.,0.,-4.64446921070048));
#28635=CARTESIAN_POINT('',(10.478132535815,10.6195538920523,-4.64446921070048));
#28636=CARTESIAN_POINT('Origin',(0.,0.,-4.64446921070048));
#28637=CARTESIAN_POINT('',(10.6195538920523,10.478132535815,-4.64446921070048));
#28638=CARTESIAN_POINT('Origin',(0.,0.,-4.64446921070048));
#28639=CARTESIAN_POINT('',(14.9183171404923,0.0999999999999478,-4.64446921070048));
#28640=CARTESIAN_POINT('Origin',(0.,0.,-4.64446921070048));
#28641=CARTESIAN_POINT('',(14.9186522951742,1.82700797808774E-15,-4.64446921070048));
#28642=CARTESIAN_POINT('Origin',(0.,0.,-4.64446921070048));
#28643=CARTESIAN_POINT('Origin',(14.3237119736335,1.75414880204189E-15,
-4.22788751277274));
#28644=CARTESIAN_POINT('',(14.9183171404923,-0.100000000000052,-4.64446921070048));
#28645=CARTESIAN_POINT('Origin',(0.,0.,-4.64446921070048));
#28646=CARTESIAN_POINT('',(10.6195538920522,-10.478132535815,-4.64446921070048));
#28647=CARTESIAN_POINT('Origin',(0.,0.,-4.64446921070048));
#28648=CARTESIAN_POINT('',(10.4781325358149,-10.6195538920523,-4.64446921070048));
#28649=CARTESIAN_POINT('Origin',(0.,0.,-4.64446921070048));
#28650=CARTESIAN_POINT('',(0.0999999999999999,-14.9183171404923,-4.64446921070048));
#28651=CARTESIAN_POINT('Origin',(0.,0.,-4.64446921070048));
#28652=CARTESIAN_POINT('',(-0.0999999999999999,-14.9183171404923,-4.64446921070048));
#28653=CARTESIAN_POINT('Origin',(0.,0.,-4.64446921070048));
#28654=CARTESIAN_POINT('',(-10.4781325358151,-10.6195538920522,-4.64446921070048));
#28655=CARTESIAN_POINT('Origin',(0.,0.,-4.64446921070048));
#28656=CARTESIAN_POINT('',(-10.6195538920524,-10.4781325358149,-4.64446921070048));
#28657=CARTESIAN_POINT('Origin',(0.,0.,-4.64446921070048));
#28658=CARTESIAN_POINT('Origin',(0.,0.,-4.64446921070048));
#28659=CARTESIAN_POINT('Origin',(0.,0.,-3.87366667012467));
#28660=CARTESIAN_POINT('',(12.7315647249454,1.55916699885417E-15,-3.87366667012467));
#28661=CARTESIAN_POINT('Origin',(0.,0.,-3.87366667012467));
#28662=CARTESIAN_POINT('',(13.5214602632505,1.65590130311878E-15,-3.23526305234773));
#28663=CARTESIAN_POINT('',(12.7315647249454,1.55916699885417E-15,-3.87366667012467));
#28664=CARTESIAN_POINT('Origin',(0.,0.,-3.23526305234774));
#28665=CARTESIAN_POINT('Origin',(0.,0.,-0.10725138426002));
#28666=CARTESIAN_POINT('',(9.6875,1.186376586674E-15,-4.95));
#28667=CARTESIAN_POINT('Origin',(0.,0.,-4.95));
#28668=CARTESIAN_POINT('Origin',(9.6875,1.186376586674E-15,-0.10725138426002));
#28669=CARTESIAN_POINT('Origin',(0.,0.,-4.22788751277274));
#28670=CARTESIAN_POINT('',(15.5300994798678,1.901888661846E-15,-4.64446921070048));
#28671=CARTESIAN_POINT('Origin',(14.3237119736335,1.75414880204189E-15,
-4.22788751277274));
#28672=CARTESIAN_POINT('',(15.5297775210912,0.0999999999999458,-4.64446921070048));
#28673=CARTESIAN_POINT('Origin',(0.,0.,-4.64446921070048));
#28674=CARTESIAN_POINT('',(14.7598894352984,0.0999999999999484,-5.42720595314676));
#28675=CARTESIAN_POINT('Origin',(14.3233829927518,0.0999999999999847,-4.22787124085886));
#28676=CARTESIAN_POINT('',(10.5075285873819,10.3661072311445,-5.42720595314676));
#28677=CARTESIAN_POINT('Origin',(0.,0.,-5.42720595314676));
#28678=CARTESIAN_POINT('',(11.0519216736007,10.9105003173633,-4.64446921070048));
#28679=CARTESIAN_POINT('Origin',(10.1988719278759,10.0574505716386,-4.22787124927498));
#28680=CARTESIAN_POINT('',(10.9105003173634,11.0519216736006,-4.64446921070048));
#28681=CARTESIAN_POINT('Origin',(0.,0.,-4.64446921070048));
#28682=CARTESIAN_POINT('',(10.3661072311446,10.5075285873818,-5.42720595314676));
#28683=CARTESIAN_POINT('Origin',(10.0574505655882,10.1988719218255,-4.22787124085886));
#28684=CARTESIAN_POINT('',(0.0999999999999999,14.7598894352984,-5.42720595314676));
#28685=CARTESIAN_POINT('Origin',(0.,0.,-5.42720595314676));
#28686=CARTESIAN_POINT('',(0.1,15.5297775210912,-4.64446921070048));
#28687=CARTESIAN_POINT('Origin',(0.100000000000003,14.3233830013084,-4.22787124927497));
#28688=CARTESIAN_POINT('',(-0.1,15.5297775210912,-4.64446921070048));
#28689=CARTESIAN_POINT('Origin',(0.,0.,-4.64446921070048));
#28690=CARTESIAN_POINT('',(-0.0999999999999999,14.7598894352984,-5.42720595314676));
#28691=CARTESIAN_POINT('Origin',(-0.100000000000018,14.3233829927518,-4.22787124085886));
#28692=CARTESIAN_POINT('',(-10.3661072311444,10.507528587382,-5.42720595314676));
#28693=CARTESIAN_POINT('Origin',(0.,0.,-5.42720595314676));
#28694=CARTESIAN_POINT('',(-10.9105003173632,11.0519216736008,-4.64446921070048));
#28695=CARTESIAN_POINT('Origin',(-10.0574505716385,10.1988719278761,-4.22787124927498));
#28696=CARTESIAN_POINT('',(-11.0519216736005,10.9105003173635,-4.64446921070048));
#28697=CARTESIAN_POINT('Origin',(0.,0.,-4.64446921070048));
#28698=CARTESIAN_POINT('',(-10.5075285873817,10.3661072311447,-5.42720595314676));
#28699=CARTESIAN_POINT('Origin',(-10.1988719218254,10.0574505655883,-4.22787124085886));
#28700=CARTESIAN_POINT('',(-14.7598894352984,0.100000000000155,-5.42720595314676));
#28701=CARTESIAN_POINT('Origin',(0.,0.,-5.42720595314676));
#28702=CARTESIAN_POINT('',(-15.5297775210912,0.100000000000163,-4.64446921070048));
#28703=CARTESIAN_POINT('Origin',(-14.3233830013084,0.10000000000015,-4.227871249275));
#28704=CARTESIAN_POINT('',(-15.5297775210912,-0.0999999999998373,-4.64446921070048));
#28705=CARTESIAN_POINT('Origin',(0.,0.,-4.64446921070048));
#28706=CARTESIAN_POINT('',(-14.7598894352984,-0.0999999999998453,-5.42720595314676));
#28707=CARTESIAN_POINT('Origin',(-14.3233829927518,-0.0999999999998497,
-4.22787124085885));
#28708=CARTESIAN_POINT('',(-10.5075285873819,-10.3661072311445,-5.42720595314676));
#28709=CARTESIAN_POINT('Origin',(0.,0.,-5.42720595314676));
#28710=CARTESIAN_POINT('',(-11.0519216736007,-10.9105003173632,-4.64446921070048));
#28711=CARTESIAN_POINT('Origin',(-10.198871927876,-10.0574505716385,-4.22787124927499));
#28712=CARTESIAN_POINT('',(-10.9105003173634,-11.0519216736006,-4.64446921070048));
#28713=CARTESIAN_POINT('Origin',(0.,0.,-4.64446921070048));
#28714=CARTESIAN_POINT('',(-10.3661072311446,-10.5075285873818,-5.42720595314676));
#28715=CARTESIAN_POINT('Origin',(-10.0574505655883,-10.1988719218254,-4.22787124085886));
#28716=CARTESIAN_POINT('',(-0.0999999999999999,-14.7598894352984,-5.42720595314676));
#28717=CARTESIAN_POINT('Origin',(0.,0.,-5.42720595314676));
#28718=CARTESIAN_POINT('',(-0.1,-15.5297775210912,-4.64446921070048));
#28719=CARTESIAN_POINT('Origin',(-0.100000000000002,-14.3233830013084,-4.22787124927497));
#28720=CARTESIAN_POINT('',(0.1,-15.5297775210912,-4.64446921070048));
#28721=CARTESIAN_POINT('Origin',(0.,0.,-4.64446921070048));
#28722=CARTESIAN_POINT('',(0.0999999999999999,-14.7598894352984,-5.42720595314676));
#28723=CARTESIAN_POINT('Origin',(0.099999999999988,-14.3233829927518,-4.22787124085886));
#28724=CARTESIAN_POINT('',(10.3661072311445,-10.5075285873819,-5.42720595314676));
#28725=CARTESIAN_POINT('Origin',(0.,0.,-5.42720595314676));
#28726=CARTESIAN_POINT('',(10.9105003173633,-11.0519216736007,-4.64446921070048));
#28727=CARTESIAN_POINT('Origin',(10.0574505716385,-10.198871927876,-4.22787124927498));
#28728=CARTESIAN_POINT('',(11.0519216736006,-10.9105003173634,-4.64446921070048));
#28729=CARTESIAN_POINT('Origin',(0.,0.,-4.64446921070048));
#28730=CARTESIAN_POINT('',(10.5075285873818,-10.3661072311446,-5.42720595314676));
#28731=CARTESIAN_POINT('Origin',(10.1988719218254,-10.0574505655883,-4.22787124085885));
#28732=CARTESIAN_POINT('',(14.7598894352984,-0.100000000000051,-5.42720595314676));
#28733=CARTESIAN_POINT('Origin',(0.,0.,-5.42720595314676));
#28734=CARTESIAN_POINT('',(15.5297775210912,-0.100000000000054,-4.64446921070048));
#28735=CARTESIAN_POINT('Origin',(14.3233830013084,-0.100000000000069,-4.22787124927498));
#28736=CARTESIAN_POINT('Origin',(0.,0.,-4.64446921070048));
#28737=CARTESIAN_POINT('Origin',(0.,0.,-5.42720595314676));
#28738=CARTESIAN_POINT('',(10.3661039408187,-10.2246825845815,-5.5));
#28739=CARTESIAN_POINT('',(10.3661039408187,-10.2246825845815,-5.5));
#28740=CARTESIAN_POINT('',(14.559884782075,-0.100000000000051,-5.5));
#28741=CARTESIAN_POINT('Origin',(0.,0.,-5.5));
#28742=CARTESIAN_POINT('',(14.7598894352984,-0.100000000000051,-5.42720595314676));
#28743=CARTESIAN_POINT('Origin',(0.,0.,-5.42720595314676));
#28744=CARTESIAN_POINT('',(10.3661039408187,10.2246825845814,-5.5));
#28745=CARTESIAN_POINT('',(14.559884782075,0.099999999999949,-5.5));
#28746=CARTESIAN_POINT('Origin',(0.,0.,-5.5));
#28747=CARTESIAN_POINT('',(10.5075285873819,10.3661072311445,-5.42720595314676));
#28748=CARTESIAN_POINT('',(14.559884782075,0.099999999999949,-5.5));
#28749=CARTESIAN_POINT('Origin',(0.,0.,-5.42720595314676));
#28750=CARTESIAN_POINT('',(0.0999999999999999,-14.559884782075,-5.5));
#28751=CARTESIAN_POINT('',(0.0999999999999999,-14.559884782075,-5.5));
#28752=CARTESIAN_POINT('',(10.2246825845814,-10.3661039408188,-5.5));
#28753=CARTESIAN_POINT('Origin',(0.,0.,-5.5));
#28754=CARTESIAN_POINT('',(10.3661072311445,-10.5075285873819,-5.42720595314676));
#28755=CARTESIAN_POINT('Origin',(0.,0.,-5.42720595314676));
#28756=CARTESIAN_POINT('',(-10.2246825845815,-10.3661039408186,-5.5));
#28757=CARTESIAN_POINT('',(-10.2246825845815,-10.3661039408186,-5.5));
#28758=CARTESIAN_POINT('',(-0.0999999999999999,-14.559884782075,-5.5));
#28759=CARTESIAN_POINT('Origin',(0.,0.,-5.5));
#28760=CARTESIAN_POINT('',(-0.0999999999999999,-14.7598894352984,-5.42720595314676));
#28761=CARTESIAN_POINT('Origin',(0.,0.,-5.42720595314676));
#28762=CARTESIAN_POINT('',(-14.559884782075,-0.0999999999998474,-5.5));
#28763=CARTESIAN_POINT('',(-14.559884782075,-0.0999999999998474,-5.5));
#28764=CARTESIAN_POINT('',(-10.3661039408188,-10.2246825845813,-5.5));
#28765=CARTESIAN_POINT('Origin',(0.,0.,-5.5));
#28766=CARTESIAN_POINT('',(-10.5075285873819,-10.3661072311445,-5.42720595314676));
#28767=CARTESIAN_POINT('Origin',(0.,0.,-5.42720595314676));
#28768=CARTESIAN_POINT('',(-10.3661039408186,10.2246825845815,-5.5));
#28769=CARTESIAN_POINT('',(-10.3661039408186,10.2246825845815,-5.5));
#28770=CARTESIAN_POINT('',(-14.559884782075,0.100000000000152,-5.5));
#28771=CARTESIAN_POINT('Origin',(0.,0.,-5.5));
#28772=CARTESIAN_POINT('',(-14.7598894352984,0.100000000000155,-5.42720595314676));
#28773=CARTESIAN_POINT('Origin',(0.,0.,-5.42720595314676));
#28774=CARTESIAN_POINT('',(-0.0999999999999999,14.559884782075,-5.5));
#28775=CARTESIAN_POINT('',(-0.0999999999999999,14.559884782075,-5.5));
#28776=CARTESIAN_POINT('',(-10.2246825845813,10.3661039408188,-5.5));
#28777=CARTESIAN_POINT('Origin',(0.,0.,-5.5));
#28778=CARTESIAN_POINT('',(-10.3661072311444,10.507528587382,-5.42720595314676));
#28779=CARTESIAN_POINT('Origin',(0.,0.,-5.42720595314676));
#28780=CARTESIAN_POINT('',(0.0999999999999999,14.559884782075,-5.5));
#28781=CARTESIAN_POINT('',(10.2246825845814,10.3661039408187,-5.5));
#28782=CARTESIAN_POINT('Origin',(0.,0.,-5.5));
#28783=CARTESIAN_POINT('',(0.0999999999999999,14.7598894352984,-5.42720595314676));
#28784=CARTESIAN_POINT('',(10.2246825845814,10.3661039408187,-5.5));
#28785=CARTESIAN_POINT('Origin',(0.,0.,-5.5));
#28786=CARTESIAN_POINT('',(10.3079086644596,-10.1664873082224,-5.27388646312339));
#28787=CARTESIAN_POINT('',(10.3079086644596,-10.1664873082224,-5.27388646312339));
#28788=CARTESIAN_POINT('',(14.477584232982,-0.10000000000005,-5.27388646312339));
#28789=CARTESIAN_POINT('Origin',(0.,0.,-5.27388646312339));
#28790=CARTESIAN_POINT('',(14.559884782075,-0.100000000000051,-5.5));
#28791=CARTESIAN_POINT('Origin',(0.,0.,-5.5));
#28792=CARTESIAN_POINT('',(10.3079086644597,10.1664873082223,-5.27388646312339));
#28793=CARTESIAN_POINT('',(14.477584232982,0.0999999999999493,-5.27388646312339));
#28794=CARTESIAN_POINT('Origin',(0.,0.,-5.27388646312339));
#28795=CARTESIAN_POINT('',(10.3661039408187,10.2246825845814,-5.5));
#28796=CARTESIAN_POINT('',(14.477584232982,0.0999999999999493,-5.27388646312339));
#28797=CARTESIAN_POINT('Origin',(0.,0.,-5.5));
#28798=CARTESIAN_POINT('',(0.0999999999999999,-14.477584232982,-5.27388646312339));
#28799=CARTESIAN_POINT('',(0.0999999999999999,-14.477584232982,-5.27388646312339));
#28800=CARTESIAN_POINT('',(10.1664873082223,-10.3079086644597,-5.27388646312339));
#28801=CARTESIAN_POINT('Origin',(0.,0.,-5.27388646312339));
#28802=CARTESIAN_POINT('',(10.2246825845814,-10.3661039408188,-5.5));
#28803=CARTESIAN_POINT('Origin',(0.,0.,-5.5));
#28804=CARTESIAN_POINT('',(-10.1664873082224,-10.3079086644595,-5.27388646312339));
#28805=CARTESIAN_POINT('',(-10.1664873082224,-10.3079086644595,-5.27388646312339));
#28806=CARTESIAN_POINT('',(-0.0999999999999999,-14.477584232982,-5.27388646312339));
#28807=CARTESIAN_POINT('Origin',(0.,0.,-5.27388646312339));
#28808=CARTESIAN_POINT('',(-0.0999999999999999,-14.559884782075,-5.5));
#28809=CARTESIAN_POINT('Origin',(0.,0.,-5.5));
#28810=CARTESIAN_POINT('',(-14.477584232982,-0.0999999999998482,-5.27388646312339));
#28811=CARTESIAN_POINT('',(-14.477584232982,-0.0999999999998482,-5.27388646312339));
#28812=CARTESIAN_POINT('',(-10.3079086644597,-10.1664873082222,-5.27388646312339));
#28813=CARTESIAN_POINT('Origin',(0.,0.,-5.27388646312339));
#28814=CARTESIAN_POINT('',(-10.3661039408188,-10.2246825845813,-5.5));
#28815=CARTESIAN_POINT('Origin',(0.,0.,-5.5));
#28816=CARTESIAN_POINT('',(-10.3079086644595,10.1664873082225,-5.27388646312339));
#28817=CARTESIAN_POINT('',(-10.3079086644595,10.1664873082225,-5.27388646312339));
#28818=CARTESIAN_POINT('',(-14.477584232982,0.100000000000151,-5.27388646312339));
#28819=CARTESIAN_POINT('Origin',(0.,0.,-5.27388646312339));
#28820=CARTESIAN_POINT('',(-14.559884782075,0.100000000000152,-5.5));
#28821=CARTESIAN_POINT('Origin',(0.,0.,-5.5));
#28822=CARTESIAN_POINT('',(-0.0999999999999999,14.477584232982,-5.27388646312339));
#28823=CARTESIAN_POINT('',(-0.0999999999999999,14.477584232982,-5.27388646312339));
#28824=CARTESIAN_POINT('',(-10.1664873082222,10.3079086644598,-5.27388646312339));
#28825=CARTESIAN_POINT('Origin',(0.,0.,-5.27388646312339));
#28826=CARTESIAN_POINT('',(-10.2246825845813,10.3661039408188,-5.5));
#28827=CARTESIAN_POINT('Origin',(0.,0.,-5.5));
#28828=CARTESIAN_POINT('',(0.0999999999999999,14.477584232982,-5.27388646312339));
#28829=CARTESIAN_POINT('',(10.1664873082223,10.3079086644596,-5.27388646312339));
#28830=CARTESIAN_POINT('Origin',(0.,0.,-5.27388646312339));
#28831=CARTESIAN_POINT('',(0.0999999999999999,14.559884782075,-5.5));
#28832=CARTESIAN_POINT('',(10.1664873082223,10.3079086644596,-5.27388646312339));
#28833=CARTESIAN_POINT('Origin',(0.,0.,-5.27388646312339));
#28834=CARTESIAN_POINT('',(10.6195538920522,-10.478132535815,-4.64446921070048));
#28835=CARTESIAN_POINT('',(14.477584232982,-0.10000000000005,-5.27388646312339));
#28836=CARTESIAN_POINT('Origin',(0.,0.,-5.27388646312339));
#28837=CARTESIAN_POINT('',(10.3079086644597,10.1664873082223,-5.27388646312339));
#28838=CARTESIAN_POINT('',(14.9183171404923,0.0999999999999478,-4.64446921070048));
#28839=CARTESIAN_POINT('Origin',(0.,0.,-5.27388646312339));
#28840=CARTESIAN_POINT('',(0.0999999999999999,-14.9183171404923,-4.64446921070048));
#28841=CARTESIAN_POINT('',(10.1664873082223,-10.3079086644597,-5.27388646312339));
#28842=CARTESIAN_POINT('Origin',(0.,0.,-5.27388646312339));
#28843=CARTESIAN_POINT('',(-10.4781325358151,-10.6195538920522,-4.64446921070048));
#28844=CARTESIAN_POINT('',(-0.0999999999999999,-14.477584232982,-5.27388646312339));
#28845=CARTESIAN_POINT('Origin',(0.,0.,-5.27388646312339));
#28846=CARTESIAN_POINT('',(-14.9183171404923,-0.0999999999998437,-4.64446921070048));
#28847=CARTESIAN_POINT('',(-10.3079086644597,-10.1664873082222,-5.27388646312339));
#28848=CARTESIAN_POINT('Origin',(0.,0.,-5.27388646312339));
#28849=CARTESIAN_POINT('',(-10.6195538920522,10.4781325358151,-4.64446921070048));
#28850=CARTESIAN_POINT('',(-14.477584232982,0.100000000000151,-5.27388646312339));
#28851=CARTESIAN_POINT('Origin',(0.,0.,-5.27388646312339));
#28852=CARTESIAN_POINT('',(-0.0999999999999999,14.9183171404923,-4.64446921070048));
#28853=CARTESIAN_POINT('',(-10.1664873082222,10.3079086644598,-5.27388646312339));
#28854=CARTESIAN_POINT('Origin',(0.,0.,-5.27388646312339));
#28855=CARTESIAN_POINT('',(0.0999999999999999,14.477584232982,-5.27388646312339));
#28856=CARTESIAN_POINT('',(10.478132535815,10.6195538920523,-4.64446921070048));
#28857=CARTESIAN_POINT('Origin',(0.,8.781875,-5.5));
#28858=CARTESIAN_POINT('Origin',(0.,9.6875,-4.95));
#28859=CARTESIAN_POINT('Origin',(0.1,15.6,-5.5));
#28860=CARTESIAN_POINT('',(0.1,15.6,-4.64446921070048));
#28861=CARTESIAN_POINT('Origin',(-0.1,15.6,-5.5));
#28862=CARTESIAN_POINT('',(-0.1,15.6,-4.64446921070048));
#28863=CARTESIAN_POINT('Origin',(0.,0.,-4.64446921070048));
#28864=CARTESIAN_POINT('Origin',(11.1015764646288,10.9601551083915,-5.5));
#28865=CARTESIAN_POINT('',(11.1015764646288,10.9601551083915,-4.64446921070048));
#28866=CARTESIAN_POINT('Origin',(10.9601551083915,11.1015764646288,-5.5));
#28867=CARTESIAN_POINT('',(10.9601551083915,11.1015764646288,-4.64446921070048));
#28868=CARTESIAN_POINT('Origin',(0.,0.,-4.64446921070048));
#28869=CARTESIAN_POINT('Origin',(-10.9601551083914,11.1015764646289,-5.5));
#28870=CARTESIAN_POINT('',(-10.9601551083914,11.1015764646289,-4.64446921070048));
#28871=CARTESIAN_POINT('Origin',(-11.1015764646287,10.9601551083916,-5.5));
#28872=CARTESIAN_POINT('',(-11.1015764646287,10.9601551083916,-4.64446921070048));
#28873=CARTESIAN_POINT('Origin',(0.,0.,-4.64446921070048));
#28874=CARTESIAN_POINT('Origin',(-15.6,0.100000000000163,-5.5));
#28875=CARTESIAN_POINT('',(-15.6,0.100000000000163,-4.64446921070048));
#28876=CARTESIAN_POINT('Origin',(-15.6,-0.0999999999998366,-5.5));
#28877=CARTESIAN_POINT('',(-15.6,-0.0999999999998366,-4.64446921070048));
#28878=CARTESIAN_POINT('Origin',(0.,0.,-4.64446921070048));
#28879=CARTESIAN_POINT('Origin',(-11.1015764646289,-10.9601551083914,-5.5));
#28880=CARTESIAN_POINT('',(-11.1015764646289,-10.9601551083914,-4.64446921070048));
#28881=CARTESIAN_POINT('Origin',(-10.9601551083916,-11.1015764646287,-5.5));
#28882=CARTESIAN_POINT('',(-10.9601551083916,-11.1015764646287,-4.64446921070048));
#28883=CARTESIAN_POINT('Origin',(0.,0.,-4.64446921070048));
#28884=CARTESIAN_POINT('Origin',(-0.1,-15.6,-5.5));
#28885=CARTESIAN_POINT('',(-0.1,-15.6,-4.64446921070048));
#28886=CARTESIAN_POINT('Origin',(0.1,-15.6,-5.5));
#28887=CARTESIAN_POINT('',(0.1,-15.6,-4.64446921070048));
#28888=CARTESIAN_POINT('Origin',(0.,0.,-4.64446921070048));
#28889=CARTESIAN_POINT('Origin',(10.9601551083914,-11.1015764646289,-5.5));
#28890=CARTESIAN_POINT('',(10.9601551083914,-11.1015764646289,-4.64446921070048));
#28891=CARTESIAN_POINT('Origin',(11.1015764646287,-10.9601551083915,-5.5));
#28892=CARTESIAN_POINT('',(11.1015764646287,-10.9601551083915,-4.64446921070048));
#28893=CARTESIAN_POINT('Origin',(0.,0.,-4.64446921070048));
#28894=CARTESIAN_POINT('Origin',(15.6,-0.100000000000054,-5.5));
#28895=CARTESIAN_POINT('',(15.6,-0.100000000000054,-4.64446921070048));
#28896=CARTESIAN_POINT('Origin',(15.6,0.0999999999999455,-5.5));
#28897=CARTESIAN_POINT('',(15.6,0.0999999999999455,-4.64446921070048));
#28898=CARTESIAN_POINT('Origin',(0.,0.,-4.64446921070048));
#28899=CARTESIAN_POINT('Origin',(0.,12.03125,4.29391783951041E-16));
#28900=CARTESIAN_POINT('',(3.828125,12.03125,1.94986732551743E-16));
#28901=CARTESIAN_POINT('',(-3.828125,12.03125,1.94986732551743E-16));
#28902=CARTESIAN_POINT('Origin',(0.,12.03125,4.29391783951041E-16));
#28903=CARTESIAN_POINT('Origin',(0.,0.,4.29391783951041E-16));
#28904=CARTESIAN_POINT('',(-8.4375,1.03329573678058E-15,1.31890179813549));
#28905=CARTESIAN_POINT('Origin',(0.,0.,1.31890179813549));
#28906=CARTESIAN_POINT('',(-8.4375,-1.03329573678058E-15,-1.31890179813548));
#28907=CARTESIAN_POINT('Origin',(-12.03125,-1.47340318022416E-15,4.29391783951041E-16));
#28908=CARTESIAN_POINT('Origin',(0.,0.,-1.31890179813548));
#28909=CARTESIAN_POINT('Origin',(0.,0.,-4.99331957165859));
#28910=CARTESIAN_POINT('',(-5.44,-6.6620785873616E-16,-5.5));
#28911=CARTESIAN_POINT('Origin',(0.,0.,-5.5));
#28912=CARTESIAN_POINT('',(-5.10805041359455,-6.25555758889188E-16,-5.06034771053142));
#28913=CARTESIAN_POINT('Origin',(-5.65395079699728,-6.92409274607934E-16,
-4.99331957165859));
#28914=CARTESIAN_POINT('',(5.10805041359455,6.25555758889188E-16,-5.06034771053142));
#28915=CARTESIAN_POINT('Origin',(0.,0.,-5.06034771053142));
#28916=CARTESIAN_POINT('Origin',(0.,0.,-5.06034771053142));
#28917=CARTESIAN_POINT('Origin',(0.,0.,-4.18034771053142));
#28918=CARTESIAN_POINT('',(-5.,6.12323399573677E-16,-4.18034771053142));
#28919=CARTESIAN_POINT('',(5.,-6.12323399573677E-16,-4.18034771053142));
#28920=CARTESIAN_POINT('Origin',(0.,0.,-4.18034771053142));
#28921=CARTESIAN_POINT('',(5.,-6.12323399573677E-16,-4.18034771053142));
#28922=CARTESIAN_POINT('Origin',(0.,0.,-4.18034771053142));
#28923=CARTESIAN_POINT('Origin',(0.,0.,5.5));
#28924=CARTESIAN_POINT('',(-5.,-6.12323399573677E-16,4.18034771053142));
#28925=CARTESIAN_POINT('',(-5.,-6.12323399573677E-16,5.5));
#28926=CARTESIAN_POINT('Origin',(0.,0.,4.18034771053142));
#28927=CARTESIAN_POINT('Origin',(0.,0.,5.06034771053142));
#28928=CARTESIAN_POINT('',(-5.10805041359455,-6.25555758889188E-16,5.06034771053142));
#28929=CARTESIAN_POINT('',(-5.10805041359455,-6.25555758889188E-16,5.06034771053142));
#28930=CARTESIAN_POINT('Origin',(0.,0.,5.06034771053142));
#28931=CARTESIAN_POINT('Origin',(0.,0.,4.99331957165859));
#28932=CARTESIAN_POINT('',(-5.44,-6.6620785873616E-16,5.5));
#28933=CARTESIAN_POINT('Origin',(-5.65395079699728,-6.92409274607934E-16,
4.99331957165859));
#28934=CARTESIAN_POINT('Origin',(0.,0.,5.5));
#28935=CARTESIAN_POINT('Origin',(0.,0.,5.06034771053142));
#28936=CARTESIAN_POINT('',(-8.21796310590599,-1.00641022131588E-15,5.5));
#28937=CARTESIAN_POINT('Origin',(0.,0.,5.5));
#28938=CARTESIAN_POINT('',(-8.4375,-1.03329573678058E-15,5.06034771053142));
#28939=CARTESIAN_POINT('Origin',(-7.8875,-9.65940162827475E-16,5.06034771053142));
#28940=CARTESIAN_POINT('Origin',(0.,0.,5.06034771053142));
#28941=CARTESIAN_POINT('Origin',(0.,0.,-5.06034771053142));
#28942=CARTESIAN_POINT('',(-8.4375,-1.03329573678058E-15,-5.06034771053142));
#28943=CARTESIAN_POINT('Origin',(0.,0.,-5.06034771053142));
#28944=CARTESIAN_POINT('',(-8.21796310590599,-1.00641022131588E-15,-5.5));
#28945=CARTESIAN_POINT('Origin',(-7.8875,-9.65940162827475E-16,-5.06034771053142));
#28946=CARTESIAN_POINT('Origin',(0.,0.,-5.5));
#28947=CARTESIAN_POINT('Origin',(0.,0.,5.5));
#28948=CARTESIAN_POINT('',(-8.4375,-1.03329573678058E-15,5.5));
#28949=CARTESIAN_POINT('Origin',(0.,0.,5.5));
#28950=CARTESIAN_POINT('',(-8.4375,-1.03329573678058E-15,5.5));
#28951=CARTESIAN_POINT('Origin',(0.,8.21796310590599,5.5));
#28952=CARTESIAN_POINT('Origin',(0.,8.21796310590599,-5.5));
#28953=CARTESIAN_POINT('Origin',(0.,0.,4.29391783951041E-16));
#28954=CARTESIAN_POINT('',(-15.625,-1.91351062366774E-15,-1.31890179813548));
#28955=CARTESIAN_POINT('Origin',(0.,0.,-1.31890179813548));
#28956=CARTESIAN_POINT('',(-15.625,-1.91351062366774E-15,1.31890179813549));
#28957=CARTESIAN_POINT('Origin',(-12.03125,-1.47340318022416E-15,4.29391783951041E-16));
#28958=CARTESIAN_POINT('Origin',(0.,0.,1.31890179813549));
#28959=CARTESIAN_POINT('Origin',(0.,0.,5.5));
#28960=CARTESIAN_POINT('',(-17.5,-2.14313189850787E-15,4.92706821010937));
#28961=CARTESIAN_POINT('Origin',(0.,0.,4.92706821010937));
#28962=CARTESIAN_POINT('',(-17.5,-2.14313189850787E-15,-4.92706821010937));
#28963=CARTESIAN_POINT('',(-17.5,-2.14313189850787E-15,5.5));
#28964=CARTESIAN_POINT('Origin',(0.,0.,-4.92706821010937));
#28965=CARTESIAN_POINT('Origin',(0.,0.,-4.92706821010937));
#28966=CARTESIAN_POINT('',(-17.0170281388728,-2.08398490412711E-15,-5.4729685935121));
#28967=CARTESIAN_POINT('Origin',(-16.95,-2.07577632455476E-15,-4.92706821010937));
#28968=CARTESIAN_POINT('Origin',(0.,0.,-5.4729685935121));
#28969=CARTESIAN_POINT('Origin',(0.,0.,-5.5));
#28970=CARTESIAN_POINT('',(-16.796875,-2.05702392044282E-15,-5.5));
#28971=CARTESIAN_POINT('',(-16.796875,-2.05702392044282E-15,-5.5));
#28972=CARTESIAN_POINT('Origin',(0.,0.,-5.5));
#28973=CARTESIAN_POINT('Origin',(0.,0.,5.4729685935121));
#28974=CARTESIAN_POINT('',(-17.0170281388728,2.11355840131749E-15,5.4729685935121));
#28975=CARTESIAN_POINT('',(17.0170281388728,-2.08398490412711E-15,5.4729685935121));
#28976=CARTESIAN_POINT('Origin',(0.,0.,5.4729685935121));
#28977=CARTESIAN_POINT('',(16.796875,-2.05702392044282E-15,5.5));
#28978=CARTESIAN_POINT('',(17.0170281388728,-2.08398490412711E-15,5.4729685935121));
#28979=CARTESIAN_POINT('Origin',(0.,0.,5.5));
#28980=CARTESIAN_POINT('Origin',(0.,0.,5.4729685935121));
#28981=CARTESIAN_POINT('Origin',(0.,0.,4.92706821010937));
#28982=CARTESIAN_POINT('Origin',(-16.95,-2.07577632455476E-15,4.92706821010937));
#28983=CARTESIAN_POINT('Origin',(0.,0.,5.5));
#28984=CARTESIAN_POINT('',(-15.625,-1.91351062366774E-15,-5.5));
#28985=CARTESIAN_POINT('Origin',(0.,0.,-5.5));
#28986=CARTESIAN_POINT('',(-15.625,-1.91351062366774E-15,5.5));
#28987=CARTESIAN_POINT('Origin',(0.,0.,5.5));
#28988=CARTESIAN_POINT('',(-15.625,-1.91351062366774E-15,5.5));
#28989=CARTESIAN_POINT('',(-15.625,-1.91351062366774E-15,5.5));
#28990=CARTESIAN_POINT('Origin',(0.,0.,5.5));
#28991=CARTESIAN_POINT('Origin',(0.,16.796875,5.5));
#28992=CARTESIAN_POINT('Origin',(0.,16.796875,-5.5));
#28993=CARTESIAN_POINT('Origin',(8.50737846115067,8.50737846115064,4.29391783951041E-16));
#28994=CARTESIAN_POINT('',(11.2142716078804,5.80048531442088,1.94986732551743E-16));
#28995=CARTESIAN_POINT('',(5.80048531442092,11.2142716078804,1.94986732551743E-16));
#28996=CARTESIAN_POINT('Origin',(8.50737846115067,8.50737846115064,4.29391783951041E-16));
#28997=CARTESIAN_POINT('Origin',(12.03125,-4.20068848579565E-14,4.29391783951041E-16));
#28998=CARTESIAN_POINT('',(12.03125,-3.82812500000004,1.94986732551743E-16));
#28999=CARTESIAN_POINT('',(12.03125,3.82812499999996,1.94986732551743E-16));
#29000=CARTESIAN_POINT('Origin',(12.03125,-4.20068848579565E-14,4.29391783951041E-16));
#29001=CARTESIAN_POINT('Origin',(8.5073784611506,-8.5073784611507,4.29391783951041E-16));
#29002=CARTESIAN_POINT('',(5.80048531442084,-11.2142716078804,1.94986732551743E-16));
#29003=CARTESIAN_POINT('',(11.2142716078804,-5.80048531442096,1.94986732551743E-16));
#29004=CARTESIAN_POINT('Origin',(8.5073784611506,-8.5073784611507,4.29391783951041E-16));
#29005=CARTESIAN_POINT('Origin',(0.,-12.03125,4.29391783951041E-16));
#29006=CARTESIAN_POINT('',(-3.828125,-12.03125,1.94986732551743E-16));
#29007=CARTESIAN_POINT('',(3.828125,-12.03125,1.94986732551743E-16));
#29008=CARTESIAN_POINT('Origin',(0.,-12.03125,4.29391783951041E-16));
#29009=CARTESIAN_POINT('Origin',(-8.50737846115072,-8.50737846115057,4.29391783951041E-16));
#29010=CARTESIAN_POINT('',(-11.2142716078805,-5.8004853144208,1.94986732551743E-16));
#29011=CARTESIAN_POINT('',(-5.80048531442099,-11.2142716078804,1.94986732551743E-16));
#29012=CARTESIAN_POINT('Origin',(-8.50737846115072,-8.50737846115057,4.29391783951041E-16));
#29013=CARTESIAN_POINT('Origin',(-12.03125,1.26020654573869E-13,4.29391783951041E-16));
#29014=CARTESIAN_POINT('',(-12.03125,3.82812500000013,1.94986732551743E-16));
#29015=CARTESIAN_POINT('',(-12.03125,-3.82812499999988,1.94986732551743E-16));
#29016=CARTESIAN_POINT('Origin',(-12.03125,1.26020654573869E-13,4.29391783951041E-16));
#29017=CARTESIAN_POINT('Origin',(-8.50737846115055,8.50737846115075,4.29391783951041E-16));
#29018=CARTESIAN_POINT('',(-5.80048531442076,11.2142716078805,1.94986732551743E-16));
#29019=CARTESIAN_POINT('',(-11.2142716078803,5.80048531442103,1.94986732551743E-16));
#29020=CARTESIAN_POINT('Origin',(-8.50737846115055,8.50737846115075,4.29391783951041E-16));
#29021=CARTESIAN_POINT('Origin',(0.,0.,4.29391783951041E-16));
#29022=CARTESIAN_POINT('',(14.46011695371,1.78923010734816E-15,2.95890965336904));
#29023=CARTESIAN_POINT('',(-14.46011695371,-1.77085359426573E-15,2.95890965336904));
#29024=CARTESIAN_POINT('Origin',(0.,0.,2.95890965336904));
#29025=CARTESIAN_POINT('Origin',(0.,0.,2.95890965336904));
#29026=CARTESIAN_POINT('',(-12.9162151497931,-1.58178015402927E-15,3.72442984888649));
#29027=CARTESIAN_POINT('Origin',(-12.03125,-1.47340318022416E-15,4.29391783951041E-16));
#29028=CARTESIAN_POINT('',(12.9162151497931,1.58178015402927E-15,3.72442984888649));
#29029=CARTESIAN_POINT('Origin',(0.,0.,3.72442984888649));
#29030=CARTESIAN_POINT('Origin',(0.,0.,3.72442984888649));
#29031=CARTESIAN_POINT('Origin',(0.,0.,0.));
#29032=CARTESIAN_POINT('',(8.671875,-1.0619983961356E-15,5.39));
#29033=CARTESIAN_POINT('Origin',(0.,0.,5.39));
#29034=CARTESIAN_POINT('',(8.671875,-1.0619983961356E-15,4.95));
#29035=CARTESIAN_POINT('',(8.671875,-1.0619983961356E-15,0.));
#29036=CARTESIAN_POINT('Origin',(0.,0.,4.95));
#29037=CARTESIAN_POINT('Origin',(0.,0.,5.39));
#29038=CARTESIAN_POINT('',(8.781875,-1.07546951092622E-15,5.5));
#29039=CARTESIAN_POINT('Origin',(0.,0.,5.5));
#29040=CARTESIAN_POINT('Origin',(8.781875,-1.07546951092622E-15,5.39));
#29041=CARTESIAN_POINT('Origin',(0.,0.,0.10725138426002));
#29042=CARTESIAN_POINT('',(13.0772848379569,-1.60150550183421E-15,4.30142548471451));
#29043=CARTESIAN_POINT('Origin',(0.,0.,4.30142548471451));
#29044=CARTESIAN_POINT('',(9.6875,-1.186376586674E-15,5.5));
#29045=CARTESIAN_POINT('Origin',(9.6875,-1.186376586674E-15,0.10725138426002));
#29046=CARTESIAN_POINT('Origin',(0.,0.,5.5));
#29047=CARTESIAN_POINT('Origin',(0.,0.,3.66302186693758));
#29048=CARTESIAN_POINT('',(13.867180376262,-1.69823980609882E-15,3.66302186693758));
#29049=CARTESIAN_POINT('Origin',(0.,0.,3.66302186693758));
#29050=CARTESIAN_POINT('',(13.867180376262,-1.69823980609882E-15,3.66302186693758));
#29051=CARTESIAN_POINT('Origin',(0.,0.,4.22788751277274));
#29052=CARTESIAN_POINT('',(-14.9183171404923,-0.0999999999998437,4.64446921070048));
#29053=CARTESIAN_POINT('',(-14.9183171404923,0.100000000000156,4.64446921070048));
#29054=CARTESIAN_POINT('Origin',(0.,0.,4.64446921070048));
#29055=CARTESIAN_POINT('',(-10.6195538920524,-10.4781325358149,4.64446921070048));
#29056=CARTESIAN_POINT('Origin',(0.,0.,4.64446921070048));
#29057=CARTESIAN_POINT('',(-10.4781325358151,-10.6195538920522,4.64446921070048));
#29058=CARTESIAN_POINT('Origin',(0.,0.,4.64446921070048));
#29059=CARTESIAN_POINT('',(-0.0999999999999999,-14.9183171404923,4.64446921070048));
#29060=CARTESIAN_POINT('Origin',(0.,0.,4.64446921070048));
#29061=CARTESIAN_POINT('',(0.0999999999999999,-14.9183171404923,4.64446921070048));
#29062=CARTESIAN_POINT('Origin',(0.,0.,4.64446921070048));
#29063=CARTESIAN_POINT('',(10.4781325358149,-10.6195538920523,4.64446921070048));
#29064=CARTESIAN_POINT('Origin',(0.,0.,4.64446921070048));
#29065=CARTESIAN_POINT('',(10.6195538920522,-10.478132535815,4.64446921070048));
#29066=CARTESIAN_POINT('Origin',(0.,0.,4.64446921070048));
#29067=CARTESIAN_POINT('',(14.9183171404923,-0.100000000000052,4.64446921070048));
#29068=CARTESIAN_POINT('Origin',(0.,0.,4.64446921070048));
#29069=CARTESIAN_POINT('',(14.9186522951742,-1.82700797808774E-15,4.64446921070048));
#29070=CARTESIAN_POINT('Origin',(0.,0.,4.64446921070048));
#29071=CARTESIAN_POINT('Origin',(14.3237119736335,-1.75414880204189E-15,
4.22788751277274));
#29072=CARTESIAN_POINT('',(14.9183171404923,0.0999999999999478,4.64446921070048));
#29073=CARTESIAN_POINT('Origin',(0.,0.,4.64446921070048));
#29074=CARTESIAN_POINT('',(10.6195538920523,10.478132535815,4.64446921070048));
#29075=CARTESIAN_POINT('Origin',(0.,0.,4.64446921070048));
#29076=CARTESIAN_POINT('',(10.478132535815,10.6195538920523,4.64446921070048));
#29077=CARTESIAN_POINT('Origin',(0.,0.,4.64446921070048));
#29078=CARTESIAN_POINT('',(0.0999999999999999,14.9183171404923,4.64446921070048));
#29079=CARTESIAN_POINT('Origin',(0.,0.,4.64446921070048));
#29080=CARTESIAN_POINT('',(-0.0999999999999999,14.9183171404923,4.64446921070048));
#29081=CARTESIAN_POINT('Origin',(0.,0.,4.64446921070048));
#29082=CARTESIAN_POINT('',(-10.4781325358149,10.6195538920524,4.64446921070048));
#29083=CARTESIAN_POINT('Origin',(0.,0.,4.64446921070048));
#29084=CARTESIAN_POINT('',(-10.6195538920522,10.4781325358151,4.64446921070048));
#29085=CARTESIAN_POINT('Origin',(0.,0.,4.64446921070048));
#29086=CARTESIAN_POINT('Origin',(0.,0.,4.64446921070048));
#29087=CARTESIAN_POINT('Origin',(0.,0.,0.10725138426002));
#29088=CARTESIAN_POINT('',(9.6875,-1.186376586674E-15,4.95));
#29089=CARTESIAN_POINT('Origin',(0.,0.,4.95));
#29090=CARTESIAN_POINT('',(12.7315647249454,-1.55916699885417E-15,3.87366667012467));
#29091=CARTESIAN_POINT('Origin',(9.6875,-1.186376586674E-15,0.10725138426002));
#29092=CARTESIAN_POINT('Origin',(0.,0.,3.87366667012467));
#29093=CARTESIAN_POINT('Origin',(0.,0.,3.87366667012467));
#29094=CARTESIAN_POINT('',(12.7315647249454,-1.55916699885417E-15,3.87366667012467));
#29095=CARTESIAN_POINT('Origin',(0.,0.,4.22788751277274));
#29096=CARTESIAN_POINT('',(15.5300994798678,-1.901888661846E-15,4.64446921070048));
#29097=CARTESIAN_POINT('Origin',(14.3237119736335,-1.75414880204189E-15,
4.22788751277274));
#29098=CARTESIAN_POINT('',(15.5297775210912,-0.100000000000054,4.64446921070048));
#29099=CARTESIAN_POINT('Origin',(0.,0.,4.64446921070048));
#29100=CARTESIAN_POINT('',(14.7598894352984,-0.100000000000051,5.42720595314676));
#29101=CARTESIAN_POINT('Origin',(14.3233830013084,-0.100000000000069,4.22787124927498));
#29102=CARTESIAN_POINT('',(10.5075285873818,-10.3661072311446,5.42720595314676));
#29103=CARTESIAN_POINT('Origin',(0.,0.,5.42720595314676));
#29104=CARTESIAN_POINT('',(11.0519216736006,-10.9105003173634,4.64446921070048));
#29105=CARTESIAN_POINT('Origin',(10.1988719218254,-10.0574505655883,4.22787124085885));
#29106=CARTESIAN_POINT('',(10.9105003173633,-11.0519216736007,4.64446921070048));
#29107=CARTESIAN_POINT('Origin',(0.,0.,4.64446921070048));
#29108=CARTESIAN_POINT('',(10.3661072311445,-10.5075285873819,5.42720595314676));
#29109=CARTESIAN_POINT('Origin',(10.0574505716385,-10.198871927876,4.22787124927498));
#29110=CARTESIAN_POINT('',(0.0999999999999999,-14.7598894352984,5.42720595314676));
#29111=CARTESIAN_POINT('Origin',(0.,0.,5.42720595314676));
#29112=CARTESIAN_POINT('',(0.1,-15.5297775210912,4.64446921070048));
#29113=CARTESIAN_POINT('Origin',(0.099999999999988,-14.3233829927518,4.22787124085886));
#29114=CARTESIAN_POINT('',(-0.1,-15.5297775210912,4.64446921070048));
#29115=CARTESIAN_POINT('Origin',(0.,0.,4.64446921070048));
#29116=CARTESIAN_POINT('',(-0.0999999999999999,-14.7598894352984,5.42720595314676));
#29117=CARTESIAN_POINT('Origin',(-0.100000000000002,-14.3233830013084,4.22787124927497));
#29118=CARTESIAN_POINT('',(-10.3661072311446,-10.5075285873818,5.42720595314676));
#29119=CARTESIAN_POINT('Origin',(0.,0.,5.42720595314676));
#29120=CARTESIAN_POINT('',(-10.9105003173634,-11.0519216736006,4.64446921070048));
#29121=CARTESIAN_POINT('Origin',(-10.0574505655883,-10.1988719218254,4.22787124085886));
#29122=CARTESIAN_POINT('',(-11.0519216736007,-10.9105003173632,4.64446921070048));
#29123=CARTESIAN_POINT('Origin',(0.,0.,4.64446921070048));
#29124=CARTESIAN_POINT('',(-10.5075285873819,-10.3661072311445,5.42720595314676));
#29125=CARTESIAN_POINT('Origin',(-10.198871927876,-10.0574505716385,4.22787124927499));
#29126=CARTESIAN_POINT('',(-14.7598894352984,-0.0999999999998453,5.42720595314676));
#29127=CARTESIAN_POINT('Origin',(0.,0.,5.42720595314676));
#29128=CARTESIAN_POINT('',(-15.5297775210912,-0.0999999999998373,4.64446921070048));
#29129=CARTESIAN_POINT('Origin',(-14.3233829927518,-0.0999999999998497,
4.22787124085885));
#29130=CARTESIAN_POINT('',(-15.5297775210912,0.100000000000163,4.64446921070048));
#29131=CARTESIAN_POINT('Origin',(0.,0.,4.64446921070048));
#29132=CARTESIAN_POINT('',(-14.7598894352984,0.100000000000155,5.42720595314676));
#29133=CARTESIAN_POINT('Origin',(-14.3233830013084,0.10000000000015,4.227871249275));
#29134=CARTESIAN_POINT('',(-10.5075285873817,10.3661072311447,5.42720595314676));
#29135=CARTESIAN_POINT('Origin',(0.,0.,5.42720595314676));
#29136=CARTESIAN_POINT('',(-11.0519216736005,10.9105003173635,4.64446921070048));
#29137=CARTESIAN_POINT('Origin',(-10.1988719218254,10.0574505655883,4.22787124085886));
#29138=CARTESIAN_POINT('',(-10.9105003173632,11.0519216736008,4.64446921070048));
#29139=CARTESIAN_POINT('Origin',(0.,0.,4.64446921070048));
#29140=CARTESIAN_POINT('',(-10.3661072311444,10.507528587382,5.42720595314676));
#29141=CARTESIAN_POINT('Origin',(-10.0574505716385,10.1988719278761,4.22787124927498));
#29142=CARTESIAN_POINT('',(-0.0999999999999999,14.7598894352984,5.42720595314676));
#29143=CARTESIAN_POINT('Origin',(0.,0.,5.42720595314676));
#29144=CARTESIAN_POINT('',(-0.1,15.5297775210912,4.64446921070048));
#29145=CARTESIAN_POINT('Origin',(-0.100000000000018,14.3233829927518,4.22787124085886));
#29146=CARTESIAN_POINT('',(0.1,15.5297775210912,4.64446921070048));
#29147=CARTESIAN_POINT('Origin',(0.,0.,4.64446921070048));
#29148=CARTESIAN_POINT('',(0.0999999999999999,14.7598894352984,5.42720595314676));
#29149=CARTESIAN_POINT('Origin',(0.100000000000003,14.3233830013084,4.22787124927497));
#29150=CARTESIAN_POINT('',(10.3661072311446,10.5075285873818,5.42720595314676));
#29151=CARTESIAN_POINT('Origin',(0.,0.,5.42720595314676));
#29152=CARTESIAN_POINT('',(10.9105003173634,11.0519216736006,4.64446921070048));
#29153=CARTESIAN_POINT('Origin',(10.0574505655882,10.1988719218255,4.22787124085886));
#29154=CARTESIAN_POINT('',(11.0519216736007,10.9105003173633,4.64446921070048));
#29155=CARTESIAN_POINT('Origin',(0.,0.,4.64446921070048));
#29156=CARTESIAN_POINT('',(10.5075285873819,10.3661072311445,5.42720595314676));
#29157=CARTESIAN_POINT('Origin',(10.1988719278759,10.0574505716386,4.22787124927498));
#29158=CARTESIAN_POINT('',(14.7598894352984,0.0999999999999484,5.42720595314676));
#29159=CARTESIAN_POINT('Origin',(0.,0.,5.42720595314676));
#29160=CARTESIAN_POINT('',(15.5297775210912,0.0999999999999458,4.64446921070048));
#29161=CARTESIAN_POINT('Origin',(14.3233829927518,0.0999999999999847,4.22787124085886));
#29162=CARTESIAN_POINT('Origin',(0.,0.,4.64446921070048));
#29163=CARTESIAN_POINT('Origin',(0.,0.,5.42720595314676));
#29164=CARTESIAN_POINT('',(14.559884782075,-0.100000000000051,5.5));
#29165=CARTESIAN_POINT('',(14.7598894352984,-0.100000000000051,5.42720595314676));
#29166=CARTESIAN_POINT('',(10.3661039408187,-10.2246825845815,5.5));
#29167=CARTESIAN_POINT('Origin',(0.,0.,5.5));
#29168=CARTESIAN_POINT('',(10.3661039408187,-10.2246825845815,5.5));
#29169=CARTESIAN_POINT('Origin',(0.,0.,5.42720595314676));
#29170=CARTESIAN_POINT('',(10.3661039408187,10.2246825845814,5.5));
#29171=CARTESIAN_POINT('',(14.559884782075,0.099999999999949,5.5));
#29172=CARTESIAN_POINT('Origin',(0.,0.,5.5));
#29173=CARTESIAN_POINT('',(14.559884782075,0.099999999999949,5.5));
#29174=CARTESIAN_POINT('',(10.5075285873819,10.3661072311445,5.42720595314676));
#29175=CARTESIAN_POINT('Origin',(0.,0.,5.42720595314676));
#29176=CARTESIAN_POINT('',(10.2246825845814,-10.3661039408188,5.5));
#29177=CARTESIAN_POINT('',(10.3661072311445,-10.5075285873819,5.42720595314676));
#29178=CARTESIAN_POINT('',(0.0999999999999999,-14.559884782075,5.5));
#29179=CARTESIAN_POINT('Origin',(0.,0.,5.5));
#29180=CARTESIAN_POINT('',(0.0999999999999999,-14.559884782075,5.5));
#29181=CARTESIAN_POINT('Origin',(0.,0.,5.42720595314676));
#29182=CARTESIAN_POINT('',(-0.0999999999999999,-14.559884782075,5.5));
#29183=CARTESIAN_POINT('',(-0.0999999999999999,-14.7598894352984,5.42720595314676));
#29184=CARTESIAN_POINT('',(-10.2246825845815,-10.3661039408186,5.5));
#29185=CARTESIAN_POINT('Origin',(0.,0.,5.5));
#29186=CARTESIAN_POINT('',(-10.2246825845815,-10.3661039408186,5.5));
#29187=CARTESIAN_POINT('Origin',(0.,0.,5.42720595314676));
#29188=CARTESIAN_POINT('',(-10.3661039408188,-10.2246825845813,5.5));
#29189=CARTESIAN_POINT('',(-10.5075285873819,-10.3661072311445,5.42720595314676));
#29190=CARTESIAN_POINT('',(-14.559884782075,-0.0999999999998474,5.5));
#29191=CARTESIAN_POINT('Origin',(0.,0.,5.5));
#29192=CARTESIAN_POINT('',(-14.559884782075,-0.0999999999998474,5.5));
#29193=CARTESIAN_POINT('Origin',(0.,0.,5.42720595314676));
#29194=CARTESIAN_POINT('',(-14.559884782075,0.100000000000152,5.5));
#29195=CARTESIAN_POINT('',(-14.7598894352984,0.100000000000155,5.42720595314676));
#29196=CARTESIAN_POINT('',(-10.3661039408186,10.2246825845815,5.5));
#29197=CARTESIAN_POINT('Origin',(0.,0.,5.5));
#29198=CARTESIAN_POINT('',(-10.3661039408186,10.2246825845815,5.5));
#29199=CARTESIAN_POINT('Origin',(0.,0.,5.42720595314676));
#29200=CARTESIAN_POINT('',(-10.2246825845813,10.3661039408188,5.5));
#29201=CARTESIAN_POINT('',(-10.3661072311444,10.507528587382,5.42720595314676));
#29202=CARTESIAN_POINT('',(-0.0999999999999999,14.559884782075,5.5));
#29203=CARTESIAN_POINT('Origin',(0.,0.,5.5));
#29204=CARTESIAN_POINT('',(-0.0999999999999999,14.559884782075,5.5));
#29205=CARTESIAN_POINT('Origin',(0.,0.,5.42720595314676));
#29206=CARTESIAN_POINT('',(0.0999999999999999,14.559884782075,5.5));
#29207=CARTESIAN_POINT('',(10.2246825845814,10.3661039408187,5.5));
#29208=CARTESIAN_POINT('Origin',(0.,0.,5.5));
#29209=CARTESIAN_POINT('',(10.2246825845814,10.3661039408187,5.5));
#29210=CARTESIAN_POINT('',(0.0999999999999999,14.7598894352984,5.42720595314676));
#29211=CARTESIAN_POINT('Origin',(0.,0.,5.5));
#29212=CARTESIAN_POINT('',(14.477584232982,-0.10000000000005,5.27388646312339));
#29213=CARTESIAN_POINT('',(14.559884782075,-0.100000000000051,5.5));
#29214=CARTESIAN_POINT('',(10.3079086644596,-10.1664873082224,5.27388646312339));
#29215=CARTESIAN_POINT('Origin',(0.,0.,5.27388646312339));
#29216=CARTESIAN_POINT('',(10.3079086644596,-10.1664873082224,5.27388646312339));
#29217=CARTESIAN_POINT('Origin',(0.,0.,5.5));
#29218=CARTESIAN_POINT('',(10.3079086644597,10.1664873082223,5.27388646312339));
#29219=CARTESIAN_POINT('',(14.477584232982,0.0999999999999493,5.27388646312339));
#29220=CARTESIAN_POINT('Origin',(0.,0.,5.27388646312339));
#29221=CARTESIAN_POINT('',(14.477584232982,0.0999999999999493,5.27388646312339));
#29222=CARTESIAN_POINT('',(10.3661039408187,10.2246825845814,5.5));
#29223=CARTESIAN_POINT('Origin',(0.,0.,5.5));
#29224=CARTESIAN_POINT('',(10.1664873082223,-10.3079086644597,5.27388646312339));
#29225=CARTESIAN_POINT('',(10.2246825845814,-10.3661039408188,5.5));
#29226=CARTESIAN_POINT('',(0.0999999999999999,-14.477584232982,5.27388646312339));
#29227=CARTESIAN_POINT('Origin',(0.,0.,5.27388646312339));
#29228=CARTESIAN_POINT('',(0.0999999999999999,-14.477584232982,5.27388646312339));
#29229=CARTESIAN_POINT('Origin',(0.,0.,5.5));
#29230=CARTESIAN_POINT('',(-0.0999999999999999,-14.477584232982,5.27388646312339));
#29231=CARTESIAN_POINT('',(-0.0999999999999999,-14.559884782075,5.5));
#29232=CARTESIAN_POINT('',(-10.1664873082224,-10.3079086644595,5.27388646312339));
#29233=CARTESIAN_POINT('Origin',(0.,0.,5.27388646312339));
#29234=CARTESIAN_POINT('',(-10.1664873082224,-10.3079086644595,5.27388646312339));
#29235=CARTESIAN_POINT('Origin',(0.,0.,5.5));
#29236=CARTESIAN_POINT('',(-10.3079086644597,-10.1664873082222,5.27388646312339));
#29237=CARTESIAN_POINT('',(-10.3661039408188,-10.2246825845813,5.5));
#29238=CARTESIAN_POINT('',(-14.477584232982,-0.0999999999998482,5.27388646312339));
#29239=CARTESIAN_POINT('Origin',(0.,0.,5.27388646312339));
#29240=CARTESIAN_POINT('',(-14.477584232982,-0.0999999999998482,5.27388646312339));
#29241=CARTESIAN_POINT('Origin',(0.,0.,5.5));
#29242=CARTESIAN_POINT('',(-14.477584232982,0.100000000000151,5.27388646312339));
#29243=CARTESIAN_POINT('',(-14.559884782075,0.100000000000152,5.5));
#29244=CARTESIAN_POINT('',(-10.3079086644595,10.1664873082225,5.27388646312339));
#29245=CARTESIAN_POINT('Origin',(0.,0.,5.27388646312339));
#29246=CARTESIAN_POINT('',(-10.3079086644595,10.1664873082225,5.27388646312339));
#29247=CARTESIAN_POINT('Origin',(0.,0.,5.5));
#29248=CARTESIAN_POINT('',(-10.1664873082222,10.3079086644598,5.27388646312339));
#29249=CARTESIAN_POINT('',(-10.2246825845813,10.3661039408188,5.5));
#29250=CARTESIAN_POINT('',(-0.0999999999999999,14.477584232982,5.27388646312339));
#29251=CARTESIAN_POINT('Origin',(0.,0.,5.27388646312339));
#29252=CARTESIAN_POINT('',(-0.0999999999999999,14.477584232982,5.27388646312339));
#29253=CARTESIAN_POINT('Origin',(0.,0.,5.5));
#29254=CARTESIAN_POINT('',(0.0999999999999999,14.477584232982,5.27388646312339));
#29255=CARTESIAN_POINT('',(10.1664873082223,10.3079086644596,5.27388646312339));
#29256=CARTESIAN_POINT('Origin',(0.,0.,5.27388646312339));
#29257=CARTESIAN_POINT('',(10.1664873082223,10.3079086644596,5.27388646312339));
#29258=CARTESIAN_POINT('',(0.0999999999999999,14.559884782075,5.5));
#29259=CARTESIAN_POINT('Origin',(0.,0.,5.27388646312339));
#29260=CARTESIAN_POINT('',(14.477584232982,-0.10000000000005,5.27388646312339));
#29261=CARTESIAN_POINT('',(10.6195538920522,-10.478132535815,4.64446921070048));
#29262=CARTESIAN_POINT('Origin',(0.,0.,5.27388646312339));
#29263=CARTESIAN_POINT('',(14.9183171404923,0.0999999999999478,4.64446921070048));
#29264=CARTESIAN_POINT('',(10.3079086644597,10.1664873082223,5.27388646312339));
#29265=CARTESIAN_POINT('Origin',(0.,0.,5.27388646312339));
#29266=CARTESIAN_POINT('',(10.1664873082223,-10.3079086644597,5.27388646312339));
#29267=CARTESIAN_POINT('',(0.0999999999999999,-14.9183171404923,4.64446921070048));
#29268=CARTESIAN_POINT('Origin',(0.,0.,5.27388646312339));
#29269=CARTESIAN_POINT('',(-0.0999999999999999,-14.477584232982,5.27388646312339));
#29270=CARTESIAN_POINT('',(-10.4781325358151,-10.6195538920522,4.64446921070048));
#29271=CARTESIAN_POINT('Origin',(0.,0.,5.27388646312339));
#29272=CARTESIAN_POINT('',(-10.3079086644597,-10.1664873082222,5.27388646312339));
#29273=CARTESIAN_POINT('',(-14.9183171404923,-0.0999999999998437,4.64446921070048));
#29274=CARTESIAN_POINT('Origin',(0.,0.,5.27388646312339));
#29275=CARTESIAN_POINT('',(-14.477584232982,0.100000000000151,5.27388646312339));
#29276=CARTESIAN_POINT('',(-10.6195538920522,10.4781325358151,4.64446921070048));
#29277=CARTESIAN_POINT('Origin',(0.,0.,5.27388646312339));
#29278=CARTESIAN_POINT('',(-10.1664873082222,10.3079086644598,5.27388646312339));
#29279=CARTESIAN_POINT('',(-0.0999999999999999,14.9183171404923,4.64446921070048));
#29280=CARTESIAN_POINT('Origin',(0.,0.,5.27388646312339));
#29281=CARTESIAN_POINT('',(10.478132535815,10.6195538920523,4.64446921070048));
#29282=CARTESIAN_POINT('',(0.0999999999999999,14.477584232982,5.27388646312339));
#29283=CARTESIAN_POINT('Origin',(0.,8.781875,5.5));
#29284=CARTESIAN_POINT('Origin',(0.,9.6875,4.95));
#29285=CARTESIAN_POINT('Origin',(0.1,15.6,5.5));
#29286=CARTESIAN_POINT('',(0.1,15.6,4.64446921070048));
#29287=CARTESIAN_POINT('Origin',(-0.1,15.6,5.5));
#29288=CARTESIAN_POINT('',(-0.1,15.6,4.64446921070048));
#29289=CARTESIAN_POINT('Origin',(0.,0.,4.64446921070048));
#29290=CARTESIAN_POINT('Origin',(11.1015764646288,10.9601551083915,5.5));
#29291=CARTESIAN_POINT('',(11.1015764646288,10.9601551083915,4.64446921070048));
#29292=CARTESIAN_POINT('Origin',(10.9601551083915,11.1015764646288,5.5));
#29293=CARTESIAN_POINT('',(10.9601551083915,11.1015764646288,4.64446921070048));
#29294=CARTESIAN_POINT('Origin',(0.,0.,4.64446921070048));
#29295=CARTESIAN_POINT('Origin',(-10.9601551083914,11.1015764646289,5.5));
#29296=CARTESIAN_POINT('',(-10.9601551083914,11.1015764646289,4.64446921070048));
#29297=CARTESIAN_POINT('Origin',(-11.1015764646287,10.9601551083916,5.5));
#29298=CARTESIAN_POINT('',(-11.1015764646287,10.9601551083916,4.64446921070048));
#29299=CARTESIAN_POINT('Origin',(0.,0.,4.64446921070048));
#29300=CARTESIAN_POINT('Origin',(-15.6,0.100000000000163,5.5));
#29301=CARTESIAN_POINT('',(-15.6,0.100000000000163,4.64446921070048));
#29302=CARTESIAN_POINT('Origin',(-15.6,-0.0999999999998366,5.5));
#29303=CARTESIAN_POINT('',(-15.6,-0.0999999999998366,4.64446921070048));
#29304=CARTESIAN_POINT('Origin',(0.,0.,4.64446921070048));
#29305=CARTESIAN_POINT('Origin',(-11.1015764646289,-10.9601551083914,5.5));
#29306=CARTESIAN_POINT('',(-11.1015764646289,-10.9601551083914,4.64446921070048));
#29307=CARTESIAN_POINT('Origin',(-10.9601551083916,-11.1015764646287,5.5));
#29308=CARTESIAN_POINT('',(-10.9601551083916,-11.1015764646287,4.64446921070048));
#29309=CARTESIAN_POINT('Origin',(0.,0.,4.64446921070048));
#29310=CARTESIAN_POINT('Origin',(-0.1,-15.6,5.5));
#29311=CARTESIAN_POINT('',(-0.1,-15.6,4.64446921070048));
#29312=CARTESIAN_POINT('Origin',(0.1,-15.6,5.5));
#29313=CARTESIAN_POINT('',(0.1,-15.6,4.64446921070048));
#29314=CARTESIAN_POINT('Origin',(0.,0.,4.64446921070048));
#29315=CARTESIAN_POINT('Origin',(10.9601551083914,-11.1015764646289,5.5));
#29316=CARTESIAN_POINT('',(10.9601551083914,-11.1015764646289,4.64446921070048));
#29317=CARTESIAN_POINT('Origin',(11.1015764646287,-10.9601551083915,5.5));
#29318=CARTESIAN_POINT('',(11.1015764646287,-10.9601551083915,4.64446921070048));
#29319=CARTESIAN_POINT('Origin',(0.,0.,4.64446921070048));
#29320=CARTESIAN_POINT('Origin',(15.6,-0.100000000000054,5.5));
#29321=CARTESIAN_POINT('',(15.6,-0.100000000000054,4.64446921070048));
#29322=CARTESIAN_POINT('Origin',(15.6,0.0999999999999455,5.5));
#29323=CARTESIAN_POINT('',(15.6,0.0999999999999455,4.64446921070048));
#29324=CARTESIAN_POINT('Origin',(0.,0.,4.64446921070048));
#29325=CARTESIAN_POINT('',(0.,0.,0.));
#29326=CARTESIAN_POINT('Origin',(94.9508316648812,0.,1.95651033903146));
#29327=CARTESIAN_POINT('',(94.9508316648812,15.,1.95651033903146));
#29328=CARTESIAN_POINT('',(94.9508316648812,15.,6.95083166488121));
#29329=CARTESIAN_POINT('',(94.9508316648812,15.,4.72825516951573));
#29330=CARTESIAN_POINT('',(94.9508316648812,495.,6.95083166488121));
#29331=CARTESIAN_POINT('',(94.9508316648812,0.,6.95083166488121));
#29332=CARTESIAN_POINT('',(94.9508316648812,495.,1.95651033903146));
#29333=CARTESIAN_POINT('',(94.9508316648812,495.,6.95083166488121));
#29334=CARTESIAN_POINT('',(94.9508316648812,0.,1.95651033903146));
#29335=CARTESIAN_POINT('Origin',(94.9508316648812,0.,6.95083166488121));
#29336=CARTESIAN_POINT('',(95.6258960932749,15.,6.95083166488121));
#29337=CARTESIAN_POINT('',(96.2254158324406,15.,6.95083166488121));
#29338=CARTESIAN_POINT('',(95.6258960932749,495.,6.95083166488121));
#29339=CARTESIAN_POINT('',(95.6258960932749,0.,6.95083166488121));
#29340=CARTESIAN_POINT('',(96.9508316648812,495.,6.95083166488121));
#29341=CARTESIAN_POINT('Origin',(95.6258960932749,0.,6.95083166488121));
#29342=CARTESIAN_POINT('',(99.25,15.,10.6122749602376));
#29343=CARTESIAN_POINT('',(96.2269045529402,15.,7.55803235551558));
#29344=CARTESIAN_POINT('',(99.25,495.,10.6122749602376));
#29345=CARTESIAN_POINT('',(99.25,0.,10.6122749602376));
#29346=CARTESIAN_POINT('',(95.6258960932749,495.,6.95083166488121));
#29347=CARTESIAN_POINT('Origin',(99.936778624571,0.,0.978255169515729));
#29348=CARTESIAN_POINT('',(99.936778624571,15.,0.978255169515729));
#29349=CARTESIAN_POINT('',(99.936778624571,15.,0.));
#29350=CARTESIAN_POINT('',(99.936778624571,15.,4.23912758475787));
#29351=CARTESIAN_POINT('',(99.936778624571,495.,0.));
#29352=CARTESIAN_POINT('',(99.936778624571,0.,0.));
#29353=CARTESIAN_POINT('',(99.936778624571,495.,0.978255169515729));
#29354=CARTESIAN_POINT('',(99.936778624571,495.,0.978255169515729));
#29355=CARTESIAN_POINT('',(99.936778624571,0.,0.978255169515729));
#29356=CARTESIAN_POINT('Origin',(100.797592784069,0.,0.978255169515729));
#29357=CARTESIAN_POINT('',(100.797592784069,15.,0.978255169515729));
#29358=CARTESIAN_POINT('',(99.1487963920345,15.,0.978255169515729));
#29359=CARTESIAN_POINT('',(100.797592784069,495.,0.978255169515729));
#29360=CARTESIAN_POINT('',(100.797592784069,495.,0.978255169515729));
#29361=CARTESIAN_POINT('',(100.797592784069,0.,0.978255169515729));
#29362=CARTESIAN_POINT('Origin',(100.797592784069,0.,1.95651033903146));
#29363=CARTESIAN_POINT('',(100.797592784069,15.,1.95651033903146));
#29364=CARTESIAN_POINT('',(100.797592784069,15.,4.72825516951573));
#29365=CARTESIAN_POINT('',(100.797592784069,495.,1.95651033903146));
#29366=CARTESIAN_POINT('',(100.797592784069,495.,1.95651033903146));
#29367=CARTESIAN_POINT('',(100.797592784069,0.,1.95651033903146));
#29368=CARTESIAN_POINT('Origin',(96.9508316648812,0.,1.95651033903146));
#29369=CARTESIAN_POINT('',(96.9508316648812,15.,1.95651033903146));
#29370=CARTESIAN_POINT('',(97.2254158324406,15.,1.95651033903146));
#29371=CARTESIAN_POINT('',(96.9508316648812,495.,1.95651033903146));
#29372=CARTESIAN_POINT('',(96.9508316648812,495.,1.95651033903146));
#29373=CARTESIAN_POINT('',(96.9508316648812,0.,1.95651033903146));
#29374=CARTESIAN_POINT('Origin',(96.9508316648812,0.,5.44638293630937));
#29375=CARTESIAN_POINT('',(96.9508316648812,15.,5.44638293630937));
#29376=CARTESIAN_POINT('',(96.9508316648812,15.,6.47319146815469));
#29377=CARTESIAN_POINT('',(96.9508316648812,495.,5.44638293630937));
#29378=CARTESIAN_POINT('',(96.9508316648812,495.,6.95083166488121));
#29379=CARTESIAN_POINT('',(96.9508316648812,0.,5.44638293630937));
#29380=CARTESIAN_POINT('Origin',(100.715659452243,0.,9.25));
#29381=CARTESIAN_POINT('',(100.715659452243,15.,9.25));
#29382=CARTESIAN_POINT('',(99.4825076947727,15.,8.00414299624016));
#29383=CARTESIAN_POINT('',(100.715659452243,495.,9.25));
#29384=CARTESIAN_POINT('',(96.9508316648812,495.,5.44638293630937));
#29385=CARTESIAN_POINT('',(100.715659452243,0.,9.25));
#29386=CARTESIAN_POINT('Origin',(115.049168335119,0.,1.95651033903146));
#29387=CARTESIAN_POINT('',(115.049168335119,15.,1.95651033903146));
#29388=CARTESIAN_POINT('',(115.049168335119,15.,6.95083166488121));
#29389=CARTESIAN_POINT('',(115.049168335119,15.,4.72825516951573));
#29390=CARTESIAN_POINT('',(115.049168335119,495.,1.95651033903146));
#29391=CARTESIAN_POINT('',(115.049168335119,0.,1.95651033903146));
#29392=CARTESIAN_POINT('',(115.049168335119,495.,6.95083166488121));
#29393=CARTESIAN_POINT('',(115.049168335119,495.,6.95083166488121));
#29394=CARTESIAN_POINT('',(115.049168335119,0.,6.95083166488121));
#29395=CARTESIAN_POINT('Origin',(115.049168335119,0.,6.95083166488121));
#29396=CARTESIAN_POINT('',(114.374103906725,15.,6.95083166488121));
#29397=CARTESIAN_POINT('',(113.774584167559,15.,6.95083166488121));
#29398=CARTESIAN_POINT('',(114.374103906725,495.,6.95083166488121));
#29399=CARTESIAN_POINT('',(113.049168335119,495.,6.95083166488121));
#29400=CARTESIAN_POINT('',(114.374103906725,0.,6.95083166488121));
#29401=CARTESIAN_POINT('Origin',(114.374103906725,0.,6.95083166488121));
#29402=CARTESIAN_POINT('',(110.75,15.,10.6122749602376));
#29403=CARTESIAN_POINT('',(113.77309544706,15.,7.55803235551558));
#29404=CARTESIAN_POINT('',(110.75,495.,10.6122749602376));
#29405=CARTESIAN_POINT('',(114.374103906725,495.,6.95083166488121));
#29406=CARTESIAN_POINT('',(110.75,0.,10.6122749602376));
#29407=CARTESIAN_POINT('Origin',(105.,0.,9.25));
#29408=CARTESIAN_POINT('',(109.284340547757,15.,9.25));
#29409=CARTESIAN_POINT('',(108.75,15.,9.25));
#29410=CARTESIAN_POINT('',(109.284340547757,495.,9.25));
#29411=CARTESIAN_POINT('',(110.75,495.,9.25));
#29412=CARTESIAN_POINT('',(109.284340547757,0.,9.25));
#29413=CARTESIAN_POINT('Origin',(110.063221375429,0.,0.978255169515729));
#29414=CARTESIAN_POINT('',(110.063221375429,15.,0.978255169515729));
#29415=CARTESIAN_POINT('',(110.063221375429,15.,0.));
#29416=CARTESIAN_POINT('',(110.063221375429,15.,4.23912758475787));
#29417=CARTESIAN_POINT('',(110.063221375429,495.,0.978255169515729));
#29418=CARTESIAN_POINT('',(110.063221375429,0.,0.978255169515729));
#29419=CARTESIAN_POINT('',(110.063221375429,495.,0.));
#29420=CARTESIAN_POINT('',(110.063221375429,495.,0.978255169515729));
#29421=CARTESIAN_POINT('',(110.063221375429,0.,0.));
#29422=CARTESIAN_POINT('Origin',(109.202407215931,0.,0.978255169515729));
#29423=CARTESIAN_POINT('',(109.202407215931,15.,0.978255169515729));
#29424=CARTESIAN_POINT('',(110.851203607966,15.,0.978255169515729));
#29425=CARTESIAN_POINT('',(109.202407215931,495.,0.978255169515729));
#29426=CARTESIAN_POINT('',(109.202407215931,0.,0.978255169515729));
#29427=CARTESIAN_POINT('',(109.202407215931,495.,0.978255169515729));
#29428=CARTESIAN_POINT('Origin',(109.202407215931,0.,1.95651033903146));
#29429=CARTESIAN_POINT('',(109.202407215931,15.,1.95651033903146));
#29430=CARTESIAN_POINT('',(109.202407215931,15.,4.72825516951573));
#29431=CARTESIAN_POINT('',(109.202407215931,495.,1.95651033903146));
#29432=CARTESIAN_POINT('',(109.202407215931,0.,1.95651033903146));
#29433=CARTESIAN_POINT('',(109.202407215931,495.,1.95651033903146));
#29434=CARTESIAN_POINT('Origin',(113.049168335119,0.,1.95651033903146));
#29435=CARTESIAN_POINT('',(113.049168335119,15.,1.95651033903146));
#29436=CARTESIAN_POINT('',(112.774584167559,15.,1.95651033903146));
#29437=CARTESIAN_POINT('',(113.049168335119,495.,1.95651033903146));
#29438=CARTESIAN_POINT('',(113.049168335119,0.,1.95651033903146));
#29439=CARTESIAN_POINT('',(113.049168335119,495.,1.95651033903146));
#29440=CARTESIAN_POINT('Origin',(113.049168335119,0.,5.44638293630937));
#29441=CARTESIAN_POINT('',(113.049168335119,15.,5.44638293630937));
#29442=CARTESIAN_POINT('',(113.049168335119,15.,6.47319146815469));
#29443=CARTESIAN_POINT('',(113.049168335119,495.,5.44638293630937));
#29444=CARTESIAN_POINT('',(113.049168335119,0.,5.44638293630937));
#29445=CARTESIAN_POINT('',(113.049168335119,495.,6.95083166488121));
#29446=CARTESIAN_POINT('Origin',(109.284340547757,0.,9.25));
#29447=CARTESIAN_POINT('',(110.517492305227,15.,8.00414299624016));
#29448=CARTESIAN_POINT('',(113.049168335119,495.,5.44638293630937));
#29449=CARTESIAN_POINT('Origin',(94.9508316648812,0.,28.0434896609685));
#29450=CARTESIAN_POINT('',(94.9508316648812,15.,28.0434896609685));
#29451=CARTESIAN_POINT('',(94.9508316648812,15.,23.0491683351188));
#29452=CARTESIAN_POINT('',(94.9508316648812,15.,25.2717448304843));
#29453=CARTESIAN_POINT('',(94.9508316648812,495.,28.0434896609685));
#29454=CARTESIAN_POINT('',(94.9508316648812,0.,28.0434896609685));
#29455=CARTESIAN_POINT('',(94.9508316648812,495.,23.0491683351188));
#29456=CARTESIAN_POINT('',(94.9508316648812,495.,23.0491683351188));
#29457=CARTESIAN_POINT('',(94.9508316648812,0.,23.0491683351188));
#29458=CARTESIAN_POINT('Origin',(94.9508316648812,0.,23.0491683351188));
#29459=CARTESIAN_POINT('',(95.6258960932749,15.,23.0491683351188));
#29460=CARTESIAN_POINT('',(96.2254158324406,15.,23.0491683351188));
#29461=CARTESIAN_POINT('',(95.6258960932749,495.,23.0491683351188));
#29462=CARTESIAN_POINT('',(96.9508316648812,495.,23.0491683351188));
#29463=CARTESIAN_POINT('',(95.6258960932749,0.,23.0491683351188));
#29464=CARTESIAN_POINT('Origin',(95.6258960932749,0.,23.0491683351188));
#29465=CARTESIAN_POINT('',(99.25,15.,19.3877250397624));
#29466=CARTESIAN_POINT('',(96.2269045529402,15.,22.4419676444844));
#29467=CARTESIAN_POINT('',(99.25,495.,19.3877250397624));
#29468=CARTESIAN_POINT('',(95.6258960932749,495.,23.0491683351188));
#29469=CARTESIAN_POINT('',(99.25,0.,19.3877250397624));
#29470=CARTESIAN_POINT('Origin',(99.25,0.,19.3877250397624));
#29471=CARTESIAN_POINT('',(99.25,15.,9.05613748011882));
#29472=CARTESIAN_POINT('',(99.25,495.,20.75));
#29473=CARTESIAN_POINT('Origin',(99.936778624571,0.,29.0217448304843));
#29474=CARTESIAN_POINT('',(99.936778624571,15.,29.0217448304843));
#29475=CARTESIAN_POINT('',(99.936778624571,15.,30.));
#29476=CARTESIAN_POINT('',(99.936778624571,15.,25.7608724152421));
#29477=CARTESIAN_POINT('',(99.936778624571,495.,29.0217448304843));
#29478=CARTESIAN_POINT('',(99.936778624571,0.,29.0217448304843));
#29479=CARTESIAN_POINT('',(99.936778624571,495.,30.));
#29480=CARTESIAN_POINT('',(99.936778624571,495.,29.0217448304843));
#29481=CARTESIAN_POINT('',(99.936778624571,0.,30.));
#29482=CARTESIAN_POINT('Origin',(100.797592784069,0.,29.0217448304843));
#29483=CARTESIAN_POINT('',(100.797592784069,15.,29.0217448304843));
#29484=CARTESIAN_POINT('',(99.1487963920345,15.,29.0217448304843));
#29485=CARTESIAN_POINT('',(100.797592784069,495.,29.0217448304843));
#29486=CARTESIAN_POINT('',(100.797592784069,0.,29.0217448304843));
#29487=CARTESIAN_POINT('',(100.797592784069,495.,29.0217448304843));
#29488=CARTESIAN_POINT('Origin',(100.797592784069,0.,28.0434896609685));
#29489=CARTESIAN_POINT('',(100.797592784069,15.,28.0434896609685));
#29490=CARTESIAN_POINT('',(100.797592784069,15.,25.2717448304843));
#29491=CARTESIAN_POINT('',(100.797592784069,495.,28.0434896609685));
#29492=CARTESIAN_POINT('',(100.797592784069,0.,28.0434896609685));
#29493=CARTESIAN_POINT('',(100.797592784069,495.,28.0434896609685));
#29494=CARTESIAN_POINT('Origin',(96.9508316648812,0.,28.0434896609685));
#29495=CARTESIAN_POINT('',(96.9508316648812,15.,28.0434896609685));
#29496=CARTESIAN_POINT('',(97.2254158324406,15.,28.0434896609685));
#29497=CARTESIAN_POINT('',(96.9508316648812,495.,28.0434896609685));
#29498=CARTESIAN_POINT('',(96.9508316648812,0.,28.0434896609685));
#29499=CARTESIAN_POINT('',(96.9508316648812,495.,28.0434896609685));
#29500=CARTESIAN_POINT('Origin',(96.9508316648812,0.,24.5536170636906));
#29501=CARTESIAN_POINT('',(96.9508316648812,15.,24.5536170636906));
#29502=CARTESIAN_POINT('',(96.9508316648812,15.,23.5268085318453));
#29503=CARTESIAN_POINT('',(96.9508316648812,495.,24.5536170636906));
#29504=CARTESIAN_POINT('',(96.9508316648812,0.,24.5536170636906));
#29505=CARTESIAN_POINT('',(96.9508316648812,495.,23.0491683351188));
#29506=CARTESIAN_POINT('Origin',(100.715659452243,0.,20.75));
#29507=CARTESIAN_POINT('',(100.715659452243,15.,20.75));
#29508=CARTESIAN_POINT('',(99.4825076947727,15.,21.9958570037598));
#29509=CARTESIAN_POINT('',(100.715659452243,495.,20.75));
#29510=CARTESIAN_POINT('',(100.715659452243,0.,20.75));
#29511=CARTESIAN_POINT('',(96.9508316648812,495.,24.5536170636906));
#29512=CARTESIAN_POINT('Origin',(115.049168335119,0.,28.0434896609685));
#29513=CARTESIAN_POINT('',(115.049168335119,15.,28.0434896609685));
#29514=CARTESIAN_POINT('',(115.049168335119,15.,23.0491683351188));
#29515=CARTESIAN_POINT('',(115.049168335119,15.,25.2717448304843));
#29516=CARTESIAN_POINT('',(115.049168335119,495.,23.0491683351188));
#29517=CARTESIAN_POINT('',(115.049168335119,0.,23.0491683351188));
#29518=CARTESIAN_POINT('',(115.049168335119,495.,28.0434896609685));
#29519=CARTESIAN_POINT('',(115.049168335119,495.,23.0491683351188));
#29520=CARTESIAN_POINT('',(115.049168335119,0.,28.0434896609685));
#29521=CARTESIAN_POINT('Origin',(115.049168335119,0.,23.0491683351188));
#29522=CARTESIAN_POINT('',(114.374103906725,15.,23.0491683351188));
#29523=CARTESIAN_POINT('',(113.774584167559,15.,23.0491683351188));
#29524=CARTESIAN_POINT('',(114.374103906725,495.,23.0491683351188));
#29525=CARTESIAN_POINT('',(114.374103906725,0.,23.0491683351188));
#29526=CARTESIAN_POINT('',(113.049168335119,495.,23.0491683351188));
#29527=CARTESIAN_POINT('Origin',(114.374103906725,0.,23.0491683351188));
#29528=CARTESIAN_POINT('',(110.75,15.,19.3877250397624));
#29529=CARTESIAN_POINT('',(113.77309544706,15.,22.4419676444844));
#29530=CARTESIAN_POINT('',(110.75,495.,19.3877250397624));
#29531=CARTESIAN_POINT('',(110.75,0.,19.3877250397624));
#29532=CARTESIAN_POINT('',(114.374103906725,495.,23.0491683351188));
#29533=CARTESIAN_POINT('Origin',(110.75,0.,19.3877250397624));
#29534=CARTESIAN_POINT('',(110.75,15.,9.05613748011882));
#29535=CARTESIAN_POINT('',(110.75,495.,20.75));
#29536=CARTESIAN_POINT('Origin',(105.,0.,15.));
#29537=CARTESIAN_POINT('',(101.75,495.,15.));
#29538=CARTESIAN_POINT('Origin',(105.,495.,15.));
#29539=CARTESIAN_POINT('',(101.75,15.,15.));
#29540=CARTESIAN_POINT('',(101.75,0.,15.));
#29541=CARTESIAN_POINT('Origin',(105.,15.,15.));
#29542=CARTESIAN_POINT('Origin',(105.,0.,20.75));
#29543=CARTESIAN_POINT('',(109.284340547757,15.,20.75));
#29544=CARTESIAN_POINT('',(108.75,15.,20.75));
#29545=CARTESIAN_POINT('',(109.284340547757,495.,20.75));
#29546=CARTESIAN_POINT('',(109.284340547757,0.,20.75));
#29547=CARTESIAN_POINT('',(110.75,495.,20.75));
#29548=CARTESIAN_POINT('Origin',(110.063221375429,0.,29.0217448304843));
#29549=CARTESIAN_POINT('',(110.063221375429,15.,29.0217448304843));
#29550=CARTESIAN_POINT('',(110.063221375429,15.,30.));
#29551=CARTESIAN_POINT('',(110.063221375429,15.,25.7608724152421));
#29552=CARTESIAN_POINT('',(110.063221375429,495.,30.));
#29553=CARTESIAN_POINT('',(110.063221375429,0.,30.));
#29554=CARTESIAN_POINT('',(110.063221375429,495.,29.0217448304843));
#29555=CARTESIAN_POINT('',(110.063221375429,495.,29.0217448304843));
#29556=CARTESIAN_POINT('',(110.063221375429,0.,29.0217448304843));
#29557=CARTESIAN_POINT('Origin',(109.202407215931,0.,29.0217448304843));
#29558=CARTESIAN_POINT('',(109.202407215931,15.,29.0217448304843));
#29559=CARTESIAN_POINT('',(110.851203607966,15.,29.0217448304843));
#29560=CARTESIAN_POINT('',(109.202407215931,495.,29.0217448304843));
#29561=CARTESIAN_POINT('',(109.202407215931,495.,29.0217448304843));
#29562=CARTESIAN_POINT('',(109.202407215931,0.,29.0217448304843));
#29563=CARTESIAN_POINT('Origin',(109.202407215931,0.,28.0434896609685));
#29564=CARTESIAN_POINT('',(109.202407215931,15.,28.0434896609685));
#29565=CARTESIAN_POINT('',(109.202407215931,15.,25.2717448304843));
#29566=CARTESIAN_POINT('',(109.202407215931,495.,28.0434896609685));
#29567=CARTESIAN_POINT('',(109.202407215931,495.,28.0434896609685));
#29568=CARTESIAN_POINT('',(109.202407215931,0.,28.0434896609685));
#29569=CARTESIAN_POINT('Origin',(113.049168335119,0.,28.0434896609685));
#29570=CARTESIAN_POINT('',(113.049168335119,15.,28.0434896609685));
#29571=CARTESIAN_POINT('',(112.774584167559,15.,28.0434896609685));
#29572=CARTESIAN_POINT('',(113.049168335119,495.,28.0434896609685));
#29573=CARTESIAN_POINT('',(113.049168335119,495.,28.0434896609685));
#29574=CARTESIAN_POINT('',(113.049168335119,0.,28.0434896609685));
#29575=CARTESIAN_POINT('Origin',(113.049168335119,0.,24.5536170636906));
#29576=CARTESIAN_POINT('',(113.049168335119,15.,24.5536170636906));
#29577=CARTESIAN_POINT('',(113.049168335119,15.,23.5268085318453));
#29578=CARTESIAN_POINT('',(113.049168335119,495.,24.5536170636906));
#29579=CARTESIAN_POINT('',(113.049168335119,495.,23.0491683351188));
#29580=CARTESIAN_POINT('',(113.049168335119,0.,24.5536170636906));
#29581=CARTESIAN_POINT('Origin',(109.284340547757,0.,20.75));
#29582=CARTESIAN_POINT('',(110.517492305227,15.,21.9958570037598));
#29583=CARTESIAN_POINT('',(113.049168335119,495.,24.5536170636906));
#29584=CARTESIAN_POINT('Origin',(148.100393916659,0.,24.8185447775707));
#29585=CARTESIAN_POINT('',(148.100393916659,15.,24.8185447775707));
#29586=CARTESIAN_POINT('',(145.213316286378,15.,24.8185447775707));
#29587=CARTESIAN_POINT('',(141.550196958329,15.,24.8185447775707));
#29588=CARTESIAN_POINT('',(148.100393916659,495.,24.8185447775707));
#29589=CARTESIAN_POINT('',(148.100393916659,0.,24.8185447775707));
#29590=CARTESIAN_POINT('',(145.213316286378,495.,24.8185447775707));
#29591=CARTESIAN_POINT('',(148.100393916659,495.,24.8185447775707));
#29592=CARTESIAN_POINT('',(145.213316286378,0.,24.8185447775707));
#29593=CARTESIAN_POINT('Origin',(145.213316286378,0.,25.3185447775707));
#29594=CARTESIAN_POINT('',(144.713316286378,15.,25.3185447775707));
#29595=CARTESIAN_POINT('Origin',(145.213316286378,15.,25.3185447775707));
#29596=CARTESIAN_POINT('',(144.713316286378,495.,25.3185447775707));
#29597=CARTESIAN_POINT('Origin',(145.213316286378,495.,25.3185447775707));
#29598=CARTESIAN_POINT('',(144.713316286378,0.,25.3185447775707));
#29599=CARTESIAN_POINT('Origin',(144.713316286378,0.,25.3185447775707));
#29600=CARTESIAN_POINT('',(144.713316286378,15.,28.1876354028612));
#29601=CARTESIAN_POINT('',(144.713316286378,15.,23.9092723887854));
#29602=CARTESIAN_POINT('',(144.713316286378,495.,28.1876354028612));
#29603=CARTESIAN_POINT('',(144.713316286378,495.,25.3185447775707));
#29604=CARTESIAN_POINT('',(144.713316286378,0.,28.1876354028612));
#29605=CARTESIAN_POINT('Origin',(145.213316286378,0.,28.1876354028611));
#29606=CARTESIAN_POINT('',(145.213316286378,15.,28.6876354028611));
#29607=CARTESIAN_POINT('Origin',(145.213316286378,15.,28.1876354028611));
#29608=CARTESIAN_POINT('',(145.213316286378,495.,28.6876354028611));
#29609=CARTESIAN_POINT('Origin',(145.213316286378,495.,28.1876354028611));
#29610=CARTESIAN_POINT('',(145.213316286378,0.,28.6876354028611));
#29611=CARTESIAN_POINT('Origin',(130.715659452243,0.,20.75));
#29612=CARTESIAN_POINT('',(130.715659452243,15.,20.75));
#29613=CARTESIAN_POINT('',(126.950831664881,15.,24.5536170636906));
#29614=CARTESIAN_POINT('',(131.338288955863,15.,20.1209555023271));
#29615=CARTESIAN_POINT('',(130.715659452243,495.,20.75));
#29616=CARTESIAN_POINT('',(130.715659452243,0.,20.75));
#29617=CARTESIAN_POINT('',(126.950831664881,495.,24.5536170636906));
#29618=CARTESIAN_POINT('',(126.950831664881,495.,24.5536170636906));
#29619=CARTESIAN_POINT('',(126.950831664881,0.,24.5536170636906));
#29620=CARTESIAN_POINT('Origin',(126.950831664881,0.,24.5536170636906));
#29621=CARTESIAN_POINT('',(126.950831664881,15.,28.0434896609686));
#29622=CARTESIAN_POINT('',(126.950831664881,15.,23.5268085318453));
#29623=CARTESIAN_POINT('',(126.950831664881,495.,28.0434896609686));
#29624=CARTESIAN_POINT('',(126.950831664881,495.,23.0491683351188));
#29625=CARTESIAN_POINT('',(126.950831664881,0.,28.0434896609686));
#29626=CARTESIAN_POINT('Origin',(126.950831664881,0.,28.0434896609686));
#29627=CARTESIAN_POINT('',(130.797592784069,15.,28.0434896609686));
#29628=CARTESIAN_POINT('',(130.975415832441,15.,28.0434896609686));
#29629=CARTESIAN_POINT('',(130.797592784069,495.,28.0434896609686));
#29630=CARTESIAN_POINT('',(126.950831664881,495.,28.0434896609686));
#29631=CARTESIAN_POINT('',(130.797592784069,0.,28.0434896609686));
#29632=CARTESIAN_POINT('Origin',(130.797592784069,0.,28.0434896609686));
#29633=CARTESIAN_POINT('',(130.797592784069,15.,29.0217448304843));
#29634=CARTESIAN_POINT('',(130.797592784069,15.,25.2717448304843));
#29635=CARTESIAN_POINT('',(130.797592784069,495.,29.0217448304843));
#29636=CARTESIAN_POINT('',(130.797592784069,495.,28.0434896609686));
#29637=CARTESIAN_POINT('',(130.797592784069,0.,29.0217448304843));
#29638=CARTESIAN_POINT('Origin',(130.797592784069,0.,29.0217448304843));
#29639=CARTESIAN_POINT('',(129.936778624571,15.,29.0217448304843));
#29640=CARTESIAN_POINT('',(132.898796392034,15.,29.0217448304843));
#29641=CARTESIAN_POINT('',(129.936778624571,495.,29.0217448304843));
#29642=CARTESIAN_POINT('',(130.797592784069,495.,29.0217448304843));
#29643=CARTESIAN_POINT('',(129.936778624571,0.,29.0217448304843));
#29644=CARTESIAN_POINT('Origin',(129.936778624571,0.,29.0217448304843));
#29645=CARTESIAN_POINT('',(129.936778624571,15.,30.));
#29646=CARTESIAN_POINT('',(129.936778624571,15.,25.7608724152422));
#29647=CARTESIAN_POINT('',(129.936778624571,495.,30.));
#29648=CARTESIAN_POINT('',(129.936778624571,495.,29.0217448304843));
#29649=CARTESIAN_POINT('',(129.936778624571,0.,30.));
#29650=CARTESIAN_POINT('Origin',(129.936778624571,0.,30.));
#29651=CARTESIAN_POINT('',(111.281610687714,15.,30.));
#29652=CARTESIAN_POINT('',(135.,495.,30.));
#29653=CARTESIAN_POINT('Origin',(120.,0.,28.0434896609686));
#29654=CARTESIAN_POINT('',(124.950831664881,15.,28.0434896609686));
#29655=CARTESIAN_POINT('',(127.5,15.,28.0434896609686));
#29656=CARTESIAN_POINT('',(124.950831664881,495.,28.0434896609686));
#29657=CARTESIAN_POINT('',(113.049168335119,495.,28.0434896609685));
#29658=CARTESIAN_POINT('',(124.950831664881,0.,28.0434896609686));
#29659=CARTESIAN_POINT('Origin',(124.950831664881,0.,28.0434896609686));
#29660=CARTESIAN_POINT('',(124.950831664881,15.,23.0491683351188));
#29661=CARTESIAN_POINT('',(124.950831664881,15.,25.2717448304843));
#29662=CARTESIAN_POINT('',(124.950831664881,495.,23.0491683351188));
#29663=CARTESIAN_POINT('',(124.950831664881,495.,23.0491683351188));
#29664=CARTESIAN_POINT('',(124.950831664881,0.,23.0491683351188));
#29665=CARTESIAN_POINT('Origin',(124.950831664881,0.,23.0491683351188));
#29666=CARTESIAN_POINT('',(125.625896093275,15.,23.0491683351188));
#29667=CARTESIAN_POINT('',(129.975415832441,15.,23.0491683351188));
#29668=CARTESIAN_POINT('',(125.625896093275,495.,23.0491683351188));
#29669=CARTESIAN_POINT('',(126.950831664881,495.,23.0491683351188));
#29670=CARTESIAN_POINT('',(125.625896093275,0.,23.0491683351188));
#29671=CARTESIAN_POINT('Origin',(125.625896093275,0.,23.0491683351188));
#29672=CARTESIAN_POINT('',(129.25,15.,19.3877250397624));
#29673=CARTESIAN_POINT('',(128.082685814031,15.,20.5670661430517));
#29674=CARTESIAN_POINT('',(129.25,495.,19.3877250397624));
#29675=CARTESIAN_POINT('',(125.625896093275,495.,23.0491683351188));
#29676=CARTESIAN_POINT('',(129.25,0.,19.3877250397624));
#29677=CARTESIAN_POINT('Origin',(148.100393916659,0.,25.3185447775707));
#29678=CARTESIAN_POINT('',(148.600393916659,15.,25.3185447775707));
#29679=CARTESIAN_POINT('Origin',(148.100393916659,15.,25.3185447775707));
#29680=CARTESIAN_POINT('',(148.600393916659,495.,25.3185447775707));
#29681=CARTESIAN_POINT('',(148.600393916659,0.,25.3185447775707));
#29682=CARTESIAN_POINT('Origin',(148.100393916659,495.,25.3185447775707));
#29683=CARTESIAN_POINT('Origin',(148.600393916659,0.,28.1876354028612));
#29684=CARTESIAN_POINT('',(148.600393916659,15.,28.1876354028612));
#29685=CARTESIAN_POINT('',(148.600393916659,15.,25.3438177014306));
#29686=CARTESIAN_POINT('',(148.600393916659,495.,28.1876354028612));
#29687=CARTESIAN_POINT('',(148.600393916659,0.,28.1876354028612));
#29688=CARTESIAN_POINT('',(148.600393916659,495.,28.1876354028612));
#29689=CARTESIAN_POINT('Origin',(148.100393916659,0.,28.1876354028611));
#29690=CARTESIAN_POINT('',(148.100393916659,15.,28.6876354028611));
#29691=CARTESIAN_POINT('Origin',(148.100393916659,15.,28.1876354028611));
#29692=CARTESIAN_POINT('',(148.100393916659,495.,28.6876354028611));
#29693=CARTESIAN_POINT('',(148.100393916659,0.,28.6876354028611));
#29694=CARTESIAN_POINT('Origin',(148.100393916659,495.,28.1876354028611));
#29695=CARTESIAN_POINT('Origin',(145.213316286378,0.,28.6876354028611));
#29696=CARTESIAN_POINT('',(140.106658143189,15.,28.6876354028611));
#29697=CARTESIAN_POINT('',(145.213316286378,495.,28.6876354028611));
#29698=CARTESIAN_POINT('Origin',(139.284340547757,0.,20.75));
#29699=CARTESIAN_POINT('',(139.284340547757,15.,20.75));
#29700=CARTESIAN_POINT('',(137.142170273878,15.,20.75));
#29701=CARTESIAN_POINT('',(139.284340547757,495.,20.75));
#29702=CARTESIAN_POINT('',(139.284340547757,0.,20.75));
#29703=CARTESIAN_POINT('',(140.75,495.,20.75));
#29704=CARTESIAN_POINT('Origin',(143.049168335119,0.,24.5536170636906));
#29705=CARTESIAN_POINT('',(143.049168335119,15.,24.5536170636906));
#29706=CARTESIAN_POINT('',(140.544124937818,15.,22.0227640341724));
#29707=CARTESIAN_POINT('',(143.049168335119,495.,24.5536170636906));
#29708=CARTESIAN_POINT('',(143.049168335119,0.,24.5536170636906));
#29709=CARTESIAN_POINT('',(143.049168335119,495.,24.5536170636906));
#29710=CARTESIAN_POINT('Origin',(143.049168335119,0.,28.0434896609686));
#29711=CARTESIAN_POINT('',(143.049168335119,15.,28.0434896609686));
#29712=CARTESIAN_POINT('',(143.049168335119,15.,25.2717448304843));
#29713=CARTESIAN_POINT('',(143.049168335119,495.,28.0434896609686));
#29714=CARTESIAN_POINT('',(143.049168335119,0.,28.0434896609686));
#29715=CARTESIAN_POINT('',(143.049168335119,495.,23.0491683351188));
#29716=CARTESIAN_POINT('Origin',(139.202407215931,0.,28.0434896609686));
#29717=CARTESIAN_POINT('',(139.202407215931,15.,28.0434896609686));
#29718=CARTESIAN_POINT('',(137.101203607966,15.,28.0434896609686));
#29719=CARTESIAN_POINT('',(139.202407215931,495.,28.0434896609686));
#29720=CARTESIAN_POINT('',(139.202407215931,0.,28.0434896609686));
#29721=CARTESIAN_POINT('',(140.063221375429,495.,28.0434896609686));
#29722=CARTESIAN_POINT('Origin',(139.202407215931,0.,29.0217448304843));
#29723=CARTESIAN_POINT('',(139.202407215931,15.,29.0217448304843));
#29724=CARTESIAN_POINT('',(139.202407215931,15.,25.7608724152422));
#29725=CARTESIAN_POINT('',(139.202407215931,495.,29.0217448304843));
#29726=CARTESIAN_POINT('',(139.202407215931,0.,29.0217448304843));
#29727=CARTESIAN_POINT('',(139.202407215931,495.,28.0434896609686));
#29728=CARTESIAN_POINT('Origin',(140.063221375429,0.,29.0217448304843));
#29729=CARTESIAN_POINT('',(140.063221375429,15.,29.0217448304843));
#29730=CARTESIAN_POINT('',(137.531610687714,15.,29.0217448304843));
#29731=CARTESIAN_POINT('',(140.063221375429,495.,29.0217448304843));
#29732=CARTESIAN_POINT('',(140.063221375429,0.,29.0217448304843));
#29733=CARTESIAN_POINT('',(139.202407215931,495.,29.0217448304843));
#29734=CARTESIAN_POINT('Origin',(140.063221375429,0.,30.));
#29735=CARTESIAN_POINT('',(140.063221375429,15.,30.));
#29736=CARTESIAN_POINT('',(140.063221375429,15.,26.25));
#29737=CARTESIAN_POINT('',(140.063221375429,495.,30.));
#29738=CARTESIAN_POINT('',(140.063221375429,0.,30.));
#29739=CARTESIAN_POINT('',(140.063221375429,495.,29.0217448304843));
#29740=CARTESIAN_POINT('Origin',(148.,0.,30.));
#29741=CARTESIAN_POINT('',(148.,15.,30.));
#29742=CARTESIAN_POINT('',(141.5,15.,30.));
#29743=CARTESIAN_POINT('',(148.,495.,30.));
#29744=CARTESIAN_POINT('',(148.,0.,30.));
#29745=CARTESIAN_POINT('',(135.,495.,30.));
#29746=CARTESIAN_POINT('Origin',(148.,0.,28.));
#29747=CARTESIAN_POINT('',(150.,15.,28.));
#29748=CARTESIAN_POINT('Origin',(148.,15.,28.));
#29749=CARTESIAN_POINT('',(150.,495.,28.));
#29750=CARTESIAN_POINT('',(150.,0.,28.));
#29751=CARTESIAN_POINT('Origin',(148.,495.,28.));
#29752=CARTESIAN_POINT('Origin',(150.,0.,20.063221375429));
#29753=CARTESIAN_POINT('',(150.,15.,20.063221375429));
#29754=CARTESIAN_POINT('',(150.,15.,21.2816106877145));
#29755=CARTESIAN_POINT('',(150.,495.,20.063221375429));
#29756=CARTESIAN_POINT('',(150.,0.,20.063221375429));
#29757=CARTESIAN_POINT('',(150.,495.,20.063221375429));
#29758=CARTESIAN_POINT('Origin',(149.021744830484,0.,20.063221375429));
#29759=CARTESIAN_POINT('',(149.021744830484,15.,20.063221375429));
#29760=CARTESIAN_POINT('',(142.010872415242,15.,20.063221375429));
#29761=CARTESIAN_POINT('',(149.021744830484,495.,20.063221375429));
#29762=CARTESIAN_POINT('',(149.021744830484,0.,20.063221375429));
#29763=CARTESIAN_POINT('',(149.021744830484,495.,20.063221375429));
#29764=CARTESIAN_POINT('Origin',(149.021744830484,0.,19.2024072159311));
#29765=CARTESIAN_POINT('',(149.021744830484,15.,19.2024072159311));
#29766=CARTESIAN_POINT('',(149.021744830484,15.,20.8512036079656));
#29767=CARTESIAN_POINT('',(149.021744830484,495.,19.2024072159311));
#29768=CARTESIAN_POINT('',(149.021744830484,0.,19.2024072159311));
#29769=CARTESIAN_POINT('',(149.021744830484,495.,19.2024072159311));
#29770=CARTESIAN_POINT('Origin',(148.043489660969,0.,19.2024072159311));
#29771=CARTESIAN_POINT('',(148.043489660969,15.,19.2024072159311));
#29772=CARTESIAN_POINT('',(141.521744830484,15.,19.2024072159311));
#29773=CARTESIAN_POINT('',(148.043489660969,495.,19.2024072159311));
#29774=CARTESIAN_POINT('',(148.043489660969,0.,19.2024072159311));
#29775=CARTESIAN_POINT('',(148.043489660969,495.,19.2024072159311));
#29776=CARTESIAN_POINT('Origin',(148.043489660969,0.,23.0491683351188));
#29777=CARTESIAN_POINT('',(148.043489660969,15.,23.0491683351188));
#29778=CARTESIAN_POINT('',(148.043489660969,15.,22.7745841675594));
#29779=CARTESIAN_POINT('',(148.043489660969,495.,23.0491683351188));
#29780=CARTESIAN_POINT('',(148.043489660969,0.,23.0491683351188));
#29781=CARTESIAN_POINT('',(148.043489660969,495.,23.0491683351188));
#29782=CARTESIAN_POINT('Origin',(144.374103906725,0.,23.0491683351188));
#29783=CARTESIAN_POINT('',(144.374103906725,15.,23.0491683351188));
#29784=CARTESIAN_POINT('',(139.687051953363,15.,23.0491683351188));
#29785=CARTESIAN_POINT('',(144.374103906725,495.,23.0491683351188));
#29786=CARTESIAN_POINT('',(144.374103906725,0.,23.0491683351188));
#29787=CARTESIAN_POINT('',(148.043489660969,495.,23.0491683351188));
#29788=CARTESIAN_POINT('Origin',(140.75,0.,19.3877250397624));
#29789=CARTESIAN_POINT('',(140.75,15.,19.3877250397624));
#29790=CARTESIAN_POINT('',(140.105262232607,15.,18.7363444953735));
#29791=CARTESIAN_POINT('',(140.75,495.,19.3877250397624));
#29792=CARTESIAN_POINT('',(140.75,0.,19.3877250397624));
#29793=CARTESIAN_POINT('',(144.374103906725,495.,23.0491683351188));
#29794=CARTESIAN_POINT('Origin',(148.100393916659,0.,5.18145522242934));
#29795=CARTESIAN_POINT('',(148.100393916659,15.,5.18145522242934));
#29796=CARTESIAN_POINT('',(145.213316286378,15.,5.18145522242934));
#29797=CARTESIAN_POINT('',(141.550196958329,15.,5.18145522242934));
#29798=CARTESIAN_POINT('',(145.213316286378,495.,5.18145522242934));
#29799=CARTESIAN_POINT('',(145.213316286378,0.,5.18145522242934));
#29800=CARTESIAN_POINT('',(148.100393916659,495.,5.18145522242934));
#29801=CARTESIAN_POINT('',(148.100393916659,495.,5.18145522242934));
#29802=CARTESIAN_POINT('',(148.100393916659,0.,5.18145522242934));
#29803=CARTESIAN_POINT('Origin',(145.213316286378,0.,4.68145522242934));
#29804=CARTESIAN_POINT('',(144.713316286378,15.,4.68145522242934));
#29805=CARTESIAN_POINT('Origin',(145.213316286378,15.,4.68145522242934));
#29806=CARTESIAN_POINT('',(144.713316286378,495.,4.68145522242934));
#29807=CARTESIAN_POINT('',(144.713316286378,0.,4.68145522242934));
#29808=CARTESIAN_POINT('Origin',(145.213316286378,495.,4.68145522242934));
#29809=CARTESIAN_POINT('Origin',(144.713316286378,0.,4.68145522242934));
#29810=CARTESIAN_POINT('',(144.713316286378,15.,1.81236459713888));
#29811=CARTESIAN_POINT('',(144.713316286378,15.,6.09072761121468));
#29812=CARTESIAN_POINT('',(144.713316286378,495.,1.81236459713888));
#29813=CARTESIAN_POINT('',(144.713316286378,0.,1.81236459713888));
#29814=CARTESIAN_POINT('',(144.713316286378,495.,4.68145522242934));
#29815=CARTESIAN_POINT('Origin',(145.213316286378,0.,1.81236459713889));
#29816=CARTESIAN_POINT('',(145.213316286378,15.,1.3123645971389));
#29817=CARTESIAN_POINT('Origin',(145.213316286378,15.,1.81236459713889));
#29818=CARTESIAN_POINT('',(145.213316286378,495.,1.3123645971389));
#29819=CARTESIAN_POINT('',(145.213316286378,0.,1.3123645971389));
#29820=CARTESIAN_POINT('Origin',(145.213316286378,495.,1.81236459713889));
#29821=CARTESIAN_POINT('Origin',(130.715659452243,0.,9.25000000000001));
#29822=CARTESIAN_POINT('',(130.715659452243,15.,9.25000000000001));
#29823=CARTESIAN_POINT('',(126.950831664881,15.,5.44638293630938));
#29824=CARTESIAN_POINT('',(131.338288955863,15.,9.8790444976729));
#29825=CARTESIAN_POINT('',(126.950831664881,495.,5.44638293630938));
#29826=CARTESIAN_POINT('',(126.950831664881,0.,5.44638293630938));
#29827=CARTESIAN_POINT('',(130.715659452243,495.,9.25000000000001));
#29828=CARTESIAN_POINT('',(126.950831664881,495.,5.44638293630938));
#29829=CARTESIAN_POINT('',(130.715659452243,0.,9.25000000000001));
#29830=CARTESIAN_POINT('Origin',(126.950831664881,0.,5.44638293630938));
#29831=CARTESIAN_POINT('',(126.950831664881,15.,1.95651033903147));
#29832=CARTESIAN_POINT('',(126.950831664881,15.,6.4731914681547));
#29833=CARTESIAN_POINT('',(126.950831664881,495.,1.95651033903147));
#29834=CARTESIAN_POINT('',(126.950831664881,0.,1.95651033903147));
#29835=CARTESIAN_POINT('',(126.950831664881,495.,6.95083166488122));
#29836=CARTESIAN_POINT('Origin',(126.950831664881,0.,1.95651033903147));
#29837=CARTESIAN_POINT('',(130.797592784069,15.,1.95651033903147));
#29838=CARTESIAN_POINT('',(130.975415832441,15.,1.95651033903147));
#29839=CARTESIAN_POINT('',(130.797592784069,495.,1.95651033903147));
#29840=CARTESIAN_POINT('',(130.797592784069,0.,1.95651033903147));
#29841=CARTESIAN_POINT('',(126.950831664881,495.,1.95651033903147));
#29842=CARTESIAN_POINT('Origin',(130.797592784069,0.,1.95651033903147));
#29843=CARTESIAN_POINT('',(130.797592784069,15.,0.978255169515743));
#29844=CARTESIAN_POINT('',(130.797592784069,15.,4.72825516951574));
#29845=CARTESIAN_POINT('',(130.797592784069,495.,0.978255169515743));
#29846=CARTESIAN_POINT('',(130.797592784069,0.,0.978255169515743));
#29847=CARTESIAN_POINT('',(130.797592784069,495.,1.95651033903147));
#29848=CARTESIAN_POINT('Origin',(130.797592784069,0.,0.978255169515743));
#29849=CARTESIAN_POINT('',(129.936778624571,15.,0.978255169515743));
#29850=CARTESIAN_POINT('',(132.898796392034,15.,0.978255169515747));
#29851=CARTESIAN_POINT('',(129.936778624571,495.,0.978255169515743));
#29852=CARTESIAN_POINT('',(129.936778624571,0.,0.978255169515743));
#29853=CARTESIAN_POINT('',(130.797592784069,495.,0.978255169515743));
#29854=CARTESIAN_POINT('Origin',(129.936778624571,0.,0.978255169515743));
#29855=CARTESIAN_POINT('',(129.936778624571,15.,1.33226762955019E-14));
#29856=CARTESIAN_POINT('',(129.936778624571,15.,4.23912758475788));
#29857=CARTESIAN_POINT('',(129.936778624571,495.,1.33226762955019E-14));
#29858=CARTESIAN_POINT('',(129.936778624571,0.,1.33226762955019E-14));
#29859=CARTESIAN_POINT('',(129.936778624571,495.,0.978255169515743));
#29860=CARTESIAN_POINT('Origin',(129.936778624571,0.,1.33226762955019E-14));
#29861=CARTESIAN_POINT('',(111.281610687714,15.,0.));
#29862=CARTESIAN_POINT('',(135.,495.,1.77635683940025E-14));
#29863=CARTESIAN_POINT('Origin',(120.,0.,1.95651033903147));
#29864=CARTESIAN_POINT('',(124.950831664881,15.,1.95651033903147));
#29865=CARTESIAN_POINT('',(127.5,15.,1.95651033903147));
#29866=CARTESIAN_POINT('',(124.950831664881,495.,1.95651033903147));
#29867=CARTESIAN_POINT('',(124.950831664881,0.,1.95651033903147));
#29868=CARTESIAN_POINT('',(113.049168335119,495.,1.95651033903146));
#29869=CARTESIAN_POINT('Origin',(124.950831664881,0.,1.95651033903147));
#29870=CARTESIAN_POINT('',(124.950831664881,15.,6.95083166488122));
#29871=CARTESIAN_POINT('',(124.950831664881,15.,4.72825516951574));
#29872=CARTESIAN_POINT('',(124.950831664881,495.,6.95083166488122));
#29873=CARTESIAN_POINT('',(124.950831664881,0.,6.95083166488122));
#29874=CARTESIAN_POINT('',(124.950831664881,495.,6.95083166488122));
#29875=CARTESIAN_POINT('Origin',(124.950831664881,0.,6.95083166488122));
#29876=CARTESIAN_POINT('',(125.625896093275,15.,6.95083166488122));
#29877=CARTESIAN_POINT('',(129.975415832441,15.,6.95083166488122));
#29878=CARTESIAN_POINT('',(125.625896093275,495.,6.95083166488122));
#29879=CARTESIAN_POINT('',(125.625896093275,0.,6.95083166488122));
#29880=CARTESIAN_POINT('',(126.950831664881,495.,6.95083166488122));
#29881=CARTESIAN_POINT('Origin',(125.625896093275,0.,6.95083166488122));
#29882=CARTESIAN_POINT('',(129.25,15.,10.6122749602377));
#29883=CARTESIAN_POINT('',(128.082685814031,15.,9.43293385694832));
#29884=CARTESIAN_POINT('',(129.25,495.,10.6122749602377));
#29885=CARTESIAN_POINT('',(129.25,0.,10.6122749602377));
#29886=CARTESIAN_POINT('',(125.625896093275,495.,6.95083166488122));
#29887=CARTESIAN_POINT('Origin',(129.25,0.,10.6122749602377));
#29888=CARTESIAN_POINT('',(129.25,15.,20.9438625198812));
#29889=CARTESIAN_POINT('',(129.25,495.,9.25000000000001));
#29890=CARTESIAN_POINT('Origin',(135.,0.,15.));
#29891=CARTESIAN_POINT('',(138.25,495.,15.));
#29892=CARTESIAN_POINT('Origin',(135.,495.,15.));
#29893=CARTESIAN_POINT('',(138.25,15.,15.));
#29894=CARTESIAN_POINT('',(138.25,0.,15.));
#29895=CARTESIAN_POINT('Origin',(135.,15.,15.));
#29896=CARTESIAN_POINT('Origin',(140.75,0.,15.));
#29897=CARTESIAN_POINT('',(140.75,15.,10.6122749602377));
#29898=CARTESIAN_POINT('',(140.75,15.,11.25));
#29899=CARTESIAN_POINT('',(140.75,495.,10.6122749602377));
#29900=CARTESIAN_POINT('',(140.75,0.,10.6122749602377));
#29901=CARTESIAN_POINT('',(140.75,495.,9.25000000000002));
#29902=CARTESIAN_POINT('Origin',(148.100393916659,0.,4.68145522242934));
#29903=CARTESIAN_POINT('',(148.600393916659,15.,4.68145522242934));
#29904=CARTESIAN_POINT('Origin',(148.100393916659,15.,4.68145522242934));
#29905=CARTESIAN_POINT('',(148.600393916659,495.,4.68145522242934));
#29906=CARTESIAN_POINT('Origin',(148.100393916659,495.,4.68145522242934));
#29907=CARTESIAN_POINT('',(148.600393916659,0.,4.68145522242934));
#29908=CARTESIAN_POINT('Origin',(148.600393916659,0.,1.81236459713888));
#29909=CARTESIAN_POINT('',(148.600393916659,15.,1.81236459713888));
#29910=CARTESIAN_POINT('',(148.600393916659,15.,4.65618229856945));
#29911=CARTESIAN_POINT('',(148.600393916659,495.,1.81236459713888));
#29912=CARTESIAN_POINT('',(148.600393916659,495.,1.81236459713888));
#29913=CARTESIAN_POINT('',(148.600393916659,0.,1.81236459713888));
#29914=CARTESIAN_POINT('Origin',(148.100393916659,0.,1.81236459713889));
#29915=CARTESIAN_POINT('',(148.100393916659,15.,1.3123645971389));
#29916=CARTESIAN_POINT('Origin',(148.100393916659,15.,1.81236459713889));
#29917=CARTESIAN_POINT('',(148.100393916659,495.,1.3123645971389));
#29918=CARTESIAN_POINT('Origin',(148.100393916659,495.,1.81236459713889));
#29919=CARTESIAN_POINT('',(148.100393916659,0.,1.3123645971389));
#29920=CARTESIAN_POINT('Origin',(145.213316286378,0.,1.3123645971389));
#29921=CARTESIAN_POINT('',(140.106658143189,15.,1.3123645971389));
#29922=CARTESIAN_POINT('',(145.213316286378,495.,1.3123645971389));
#29923=CARTESIAN_POINT('Origin',(139.284340547757,0.,9.25000000000002));
#29924=CARTESIAN_POINT('',(139.284340547757,15.,9.25000000000002));
#29925=CARTESIAN_POINT('',(137.142170273878,15.,9.25000000000002));
#29926=CARTESIAN_POINT('',(139.284340547757,495.,9.25000000000002));
#29927=CARTESIAN_POINT('',(140.75,495.,9.25000000000002));
#29928=CARTESIAN_POINT('',(139.284340547757,0.,9.25000000000002));
#29929=CARTESIAN_POINT('Origin',(143.049168335119,0.,5.44638293630939));
#29930=CARTESIAN_POINT('',(143.049168335119,15.,5.44638293630939));
#29931=CARTESIAN_POINT('',(140.544124937818,15.,7.9772359658276));
#29932=CARTESIAN_POINT('',(143.049168335119,495.,5.44638293630939));
#29933=CARTESIAN_POINT('',(143.049168335119,495.,5.44638293630939));
#29934=CARTESIAN_POINT('',(143.049168335119,0.,5.44638293630939));
#29935=CARTESIAN_POINT('Origin',(143.049168335119,0.,1.95651033903148));
#29936=CARTESIAN_POINT('',(143.049168335119,15.,1.95651033903148));
#29937=CARTESIAN_POINT('',(143.049168335119,15.,4.72825516951575));
#29938=CARTESIAN_POINT('',(143.049168335119,495.,1.95651033903148));
#29939=CARTESIAN_POINT('',(143.049168335119,495.,6.95083166488122));
#29940=CARTESIAN_POINT('',(143.049168335119,0.,1.95651033903148));
#29941=CARTESIAN_POINT('Origin',(139.202407215931,0.,1.95651033903148));
#29942=CARTESIAN_POINT('',(139.202407215931,15.,1.95651033903148));
#29943=CARTESIAN_POINT('',(137.101203607966,15.,1.95651033903148));
#29944=CARTESIAN_POINT('',(139.202407215931,495.,1.95651033903148));
#29945=CARTESIAN_POINT('',(140.063221375429,495.,1.95651033903148));
#29946=CARTESIAN_POINT('',(139.202407215931,0.,1.95651033903148));
#29947=CARTESIAN_POINT('Origin',(139.202407215931,0.,0.978255169515747));
#29948=CARTESIAN_POINT('',(139.202407215931,15.,0.978255169515747));
#29949=CARTESIAN_POINT('',(139.202407215931,15.,4.23912758475788));
#29950=CARTESIAN_POINT('',(139.202407215931,495.,0.978255169515747));
#29951=CARTESIAN_POINT('',(139.202407215931,495.,1.95651033903148));
#29952=CARTESIAN_POINT('',(139.202407215931,0.,0.978255169515747));
#29953=CARTESIAN_POINT('Origin',(140.063221375429,0.,0.978255169515747));
#29954=CARTESIAN_POINT('',(140.063221375429,15.,0.978255169515747));
#29955=CARTESIAN_POINT('',(137.531610687715,15.,0.978255169515747));
#29956=CARTESIAN_POINT('',(140.063221375429,495.,0.978255169515747));
#29957=CARTESIAN_POINT('',(139.202407215931,495.,0.978255169515747));
#29958=CARTESIAN_POINT('',(140.063221375429,0.,0.978255169515747));
#29959=CARTESIAN_POINT('Origin',(140.063221375429,0.,1.77635683940025E-14));
#29960=CARTESIAN_POINT('',(140.063221375429,15.,1.77635683940025E-14));
#29961=CARTESIAN_POINT('',(140.063221375429,15.,3.75000000000002));
#29962=CARTESIAN_POINT('',(140.063221375429,495.,1.77635683940025E-14));
#29963=CARTESIAN_POINT('',(140.063221375429,495.,0.978255169515747));
#29964=CARTESIAN_POINT('',(140.063221375429,0.,1.77635683940025E-14));
#29965=CARTESIAN_POINT('Origin',(148.,0.,1.77635683940025E-14));
#29966=CARTESIAN_POINT('',(148.,15.,1.77635683940025E-14));
#29967=CARTESIAN_POINT('',(141.5,15.,1.77635683940025E-14));
#29968=CARTESIAN_POINT('',(148.,495.,1.77635683940025E-14));
#29969=CARTESIAN_POINT('',(135.,495.,1.77635683940025E-14));
#29970=CARTESIAN_POINT('',(148.,0.,1.77635683940025E-14));
#29971=CARTESIAN_POINT('Origin',(148.,0.,2.00000000000002));
#29972=CARTESIAN_POINT('',(150.,15.,2.00000000000002));
#29973=CARTESIAN_POINT('Origin',(148.,15.,2.00000000000002));
#29974=CARTESIAN_POINT('',(150.,495.,2.00000000000002));
#29975=CARTESIAN_POINT('Origin',(148.,495.,2.00000000000002));
#29976=CARTESIAN_POINT('',(150.,0.,2.00000000000002));
#29977=CARTESIAN_POINT('Origin',(150.,0.,9.93677862457105));
#29978=CARTESIAN_POINT('',(150.,15.,9.93677862457105));
#29979=CARTESIAN_POINT('',(150.,15.,8.71838931228553));
#29980=CARTESIAN_POINT('',(150.,495.,9.93677862457105));
#29981=CARTESIAN_POINT('',(150.,495.,9.93677862457105));
#29982=CARTESIAN_POINT('',(150.,0.,9.93677862457105));
#29983=CARTESIAN_POINT('Origin',(149.021744830484,0.,9.93677862457105));
#29984=CARTESIAN_POINT('',(149.021744830484,15.,9.93677862457105));
#29985=CARTESIAN_POINT('',(142.010872415242,15.,9.93677862457105));
#29986=CARTESIAN_POINT('',(149.021744830484,495.,9.93677862457105));
#29987=CARTESIAN_POINT('',(149.021744830484,495.,9.93677862457105));
#29988=CARTESIAN_POINT('',(149.021744830484,0.,9.93677862457105));
#29989=CARTESIAN_POINT('Origin',(149.021744830484,0.,10.7975927840689));
#29990=CARTESIAN_POINT('',(149.021744830484,15.,10.7975927840689));
#29991=CARTESIAN_POINT('',(149.021744830484,15.,9.14879639203446));
#29992=CARTESIAN_POINT('',(149.021744830484,495.,10.7975927840689));
#29993=CARTESIAN_POINT('',(149.021744830484,495.,10.7975927840689));
#29994=CARTESIAN_POINT('',(149.021744830484,0.,10.7975927840689));
#29995=CARTESIAN_POINT('Origin',(148.043489660969,0.,10.7975927840689));
#29996=CARTESIAN_POINT('',(148.043489660969,15.,10.7975927840689));
#29997=CARTESIAN_POINT('',(141.521744830484,15.,10.7975927840689));
#29998=CARTESIAN_POINT('',(148.043489660969,495.,10.7975927840689));
#29999=CARTESIAN_POINT('',(148.043489660969,495.,10.7975927840689));
#30000=CARTESIAN_POINT('',(148.043489660969,0.,10.7975927840689));
#30001=CARTESIAN_POINT('Origin',(148.043489660969,0.,6.95083166488122));
#30002=CARTESIAN_POINT('',(148.043489660969,15.,6.95083166488122));
#30003=CARTESIAN_POINT('',(148.043489660969,15.,7.22541583244062));
#30004=CARTESIAN_POINT('',(148.043489660969,495.,6.95083166488122));
#30005=CARTESIAN_POINT('',(148.043489660969,495.,6.95083166488122));
#30006=CARTESIAN_POINT('',(148.043489660969,0.,6.95083166488122));
#30007=CARTESIAN_POINT('Origin',(144.374103906725,0.,6.95083166488122));
#30008=CARTESIAN_POINT('',(144.374103906725,15.,6.95083166488122));
#30009=CARTESIAN_POINT('',(139.687051953363,15.,6.95083166488122));
#30010=CARTESIAN_POINT('',(144.374103906725,495.,6.95083166488122));
#30011=CARTESIAN_POINT('',(148.043489660969,495.,6.95083166488122));
#30012=CARTESIAN_POINT('',(144.374103906725,0.,6.95083166488122));
#30013=CARTESIAN_POINT('Origin',(140.75,0.,10.6122749602377));
#30014=CARTESIAN_POINT('',(140.105262232607,15.,11.2636555046265));
#30015=CARTESIAN_POINT('',(144.374103906725,495.,6.95083166488122));
#30016=CARTESIAN_POINT('Origin',(64.9508316648812,0.,1.95651033903146));
#30017=CARTESIAN_POINT('',(64.9508316648812,15.,1.95651033903146));
#30018=CARTESIAN_POINT('',(64.9508316648812,15.,6.95083166488121));
#30019=CARTESIAN_POINT('',(64.9508316648812,15.,4.72825516951573));
#30020=CARTESIAN_POINT('',(64.9508316648812,495.,6.95083166488121));
#30021=CARTESIAN_POINT('',(64.9508316648812,0.,6.95083166488121));
#30022=CARTESIAN_POINT('',(64.9508316648812,495.,1.95651033903146));
#30023=CARTESIAN_POINT('',(64.9508316648812,495.,6.95083166488121));
#30024=CARTESIAN_POINT('',(64.9508316648812,0.,1.95651033903146));
#30025=CARTESIAN_POINT('Origin',(64.9508316648812,0.,6.95083166488121));
#30026=CARTESIAN_POINT('',(65.6258960932749,15.,6.95083166488121));
#30027=CARTESIAN_POINT('',(66.2254158324406,15.,6.95083166488121));
#30028=CARTESIAN_POINT('',(65.6258960932749,495.,6.95083166488121));
#30029=CARTESIAN_POINT('',(65.6258960932749,0.,6.95083166488121));
#30030=CARTESIAN_POINT('',(66.9508316648812,495.,6.95083166488121));
#30031=CARTESIAN_POINT('Origin',(65.6258960932749,0.,6.95083166488121));
#30032=CARTESIAN_POINT('',(69.25,15.,10.6122749602376));
#30033=CARTESIAN_POINT('',(66.2269045529402,15.,7.55803235551558));
#30034=CARTESIAN_POINT('',(69.25,495.,10.6122749602376));
#30035=CARTESIAN_POINT('',(69.25,0.,10.6122749602376));
#30036=CARTESIAN_POINT('',(65.6258960932749,495.,6.95083166488121));
#30037=CARTESIAN_POINT('Origin',(69.936778624571,0.,0.978255169515729));
#30038=CARTESIAN_POINT('',(69.936778624571,15.,0.978255169515729));
#30039=CARTESIAN_POINT('',(69.936778624571,15.,0.));
#30040=CARTESIAN_POINT('',(69.936778624571,15.,4.23912758475787));
#30041=CARTESIAN_POINT('',(69.936778624571,495.,0.));
#30042=CARTESIAN_POINT('',(69.936778624571,0.,0.));
#30043=CARTESIAN_POINT('',(69.936778624571,495.,0.978255169515729));
#30044=CARTESIAN_POINT('',(69.936778624571,495.,0.978255169515729));
#30045=CARTESIAN_POINT('',(69.936778624571,0.,0.978255169515729));
#30046=CARTESIAN_POINT('Origin',(70.7975927840689,0.,0.978255169515729));
#30047=CARTESIAN_POINT('',(70.7975927840689,15.,0.978255169515729));
#30048=CARTESIAN_POINT('',(69.1487963920345,15.,0.978255169515729));
#30049=CARTESIAN_POINT('',(70.7975927840689,495.,0.978255169515729));
#30050=CARTESIAN_POINT('',(70.7975927840689,495.,0.978255169515729));
#30051=CARTESIAN_POINT('',(70.7975927840689,0.,0.978255169515729));
#30052=CARTESIAN_POINT('Origin',(70.7975927840689,0.,1.95651033903146));
#30053=CARTESIAN_POINT('',(70.7975927840689,15.,1.95651033903146));
#30054=CARTESIAN_POINT('',(70.7975927840689,15.,4.72825516951573));
#30055=CARTESIAN_POINT('',(70.7975927840689,495.,1.95651033903146));
#30056=CARTESIAN_POINT('',(70.7975927840689,495.,1.95651033903146));
#30057=CARTESIAN_POINT('',(70.7975927840689,0.,1.95651033903146));
#30058=CARTESIAN_POINT('Origin',(66.9508316648812,0.,1.95651033903146));
#30059=CARTESIAN_POINT('',(66.9508316648812,15.,1.95651033903146));
#30060=CARTESIAN_POINT('',(67.2254158324406,15.,1.95651033903146));
#30061=CARTESIAN_POINT('',(66.9508316648812,495.,1.95651033903146));
#30062=CARTESIAN_POINT('',(66.9508316648812,495.,1.95651033903146));
#30063=CARTESIAN_POINT('',(66.9508316648812,0.,1.95651033903146));
#30064=CARTESIAN_POINT('Origin',(66.9508316648812,0.,5.44638293630937));
#30065=CARTESIAN_POINT('',(66.9508316648812,15.,5.44638293630937));
#30066=CARTESIAN_POINT('',(66.9508316648812,15.,6.47319146815469));
#30067=CARTESIAN_POINT('',(66.9508316648812,495.,5.44638293630937));
#30068=CARTESIAN_POINT('',(66.9508316648812,495.,6.95083166488121));
#30069=CARTESIAN_POINT('',(66.9508316648812,0.,5.44638293630937));
#30070=CARTESIAN_POINT('Origin',(70.715659452243,0.,9.25));
#30071=CARTESIAN_POINT('',(70.715659452243,15.,9.25));
#30072=CARTESIAN_POINT('',(69.4825076947727,15.,8.00414299624016));
#30073=CARTESIAN_POINT('',(70.715659452243,495.,9.25));
#30074=CARTESIAN_POINT('',(66.9508316648812,495.,5.44638293630937));
#30075=CARTESIAN_POINT('',(70.715659452243,0.,9.25));
#30076=CARTESIAN_POINT('Origin',(90.,0.,1.95651033903146));
#30077=CARTESIAN_POINT('',(85.0491683351188,15.,1.95651033903146));
#30078=CARTESIAN_POINT('',(86.25,15.,1.95651033903146));
#30079=CARTESIAN_POINT('',(85.0491683351188,495.,1.95651033903146));
#30080=CARTESIAN_POINT('',(83.0491683351188,495.,1.95651033903146));
#30081=CARTESIAN_POINT('',(85.0491683351188,0.,1.95651033903146));
#30082=CARTESIAN_POINT('Origin',(85.0491683351188,0.,1.95651033903146));
#30083=CARTESIAN_POINT('',(85.0491683351188,15.,6.95083166488121));
#30084=CARTESIAN_POINT('',(85.0491683351188,15.,4.72825516951573));
#30085=CARTESIAN_POINT('',(85.0491683351188,495.,6.95083166488121));
#30086=CARTESIAN_POINT('',(85.0491683351188,495.,6.95083166488121));
#30087=CARTESIAN_POINT('',(85.0491683351188,0.,6.95083166488121));
#30088=CARTESIAN_POINT('Origin',(85.0491683351188,0.,6.95083166488121));
#30089=CARTESIAN_POINT('',(84.3741039067251,15.,6.95083166488121));
#30090=CARTESIAN_POINT('',(83.7745841675594,15.,6.95083166488121));
#30091=CARTESIAN_POINT('',(84.3741039067251,495.,6.95083166488121));
#30092=CARTESIAN_POINT('',(83.0491683351188,495.,6.95083166488121));
#30093=CARTESIAN_POINT('',(84.3741039067251,0.,6.95083166488121));
#30094=CARTESIAN_POINT('Origin',(84.3741039067251,0.,6.95083166488121));
#30095=CARTESIAN_POINT('',(80.75,15.,10.6122749602376));
#30096=CARTESIAN_POINT('',(83.7730954470598,15.,7.55803235551558));
#30097=CARTESIAN_POINT('',(80.75,495.,10.6122749602376));
#30098=CARTESIAN_POINT('',(84.3741039067251,495.,6.95083166488121));
#30099=CARTESIAN_POINT('',(80.75,0.,10.6122749602376));
#30100=CARTESIAN_POINT('Origin',(75.,0.,9.25));
#30101=CARTESIAN_POINT('',(79.284340547757,15.,9.25));
#30102=CARTESIAN_POINT('',(78.75,15.,9.25));
#30103=CARTESIAN_POINT('',(79.284340547757,495.,9.25));
#30104=CARTESIAN_POINT('',(80.75,495.,9.25));
#30105=CARTESIAN_POINT('',(79.284340547757,0.,9.25));
#30106=CARTESIAN_POINT('Origin',(80.063221375429,0.,0.));
#30107=CARTESIAN_POINT('',(80.063221375429,15.,0.));
#30108=CARTESIAN_POINT('',(98.7183893122855,15.,0.));
#30109=CARTESIAN_POINT('',(80.063221375429,495.,0.));
#30110=CARTESIAN_POINT('',(80.063221375429,0.,0.));
#30111=CARTESIAN_POINT('',(75.,495.,0.));
#30112=CARTESIAN_POINT('Origin',(80.063221375429,0.,0.978255169515729));
#30113=CARTESIAN_POINT('',(80.063221375429,15.,0.978255169515729));
#30114=CARTESIAN_POINT('',(80.063221375429,15.,4.23912758475787));
#30115=CARTESIAN_POINT('',(80.063221375429,495.,0.978255169515729));
#30116=CARTESIAN_POINT('',(80.063221375429,0.,0.978255169515729));
#30117=CARTESIAN_POINT('',(80.063221375429,495.,0.978255169515729));
#30118=CARTESIAN_POINT('Origin',(79.2024072159311,0.,0.978255169515729));
#30119=CARTESIAN_POINT('',(79.2024072159311,15.,0.978255169515729));
#30120=CARTESIAN_POINT('',(80.8512036079655,15.,0.978255169515729));
#30121=CARTESIAN_POINT('',(79.2024072159311,495.,0.978255169515729));
#30122=CARTESIAN_POINT('',(79.2024072159311,0.,0.978255169515729));
#30123=CARTESIAN_POINT('',(79.2024072159311,495.,0.978255169515729));
#30124=CARTESIAN_POINT('Origin',(79.2024072159311,0.,1.95651033903146));
#30125=CARTESIAN_POINT('',(79.2024072159311,15.,1.95651033903146));
#30126=CARTESIAN_POINT('',(79.2024072159311,15.,4.72825516951573));
#30127=CARTESIAN_POINT('',(79.2024072159311,495.,1.95651033903146));
#30128=CARTESIAN_POINT('',(79.2024072159311,0.,1.95651033903146));
#30129=CARTESIAN_POINT('',(79.2024072159311,495.,1.95651033903146));
#30130=CARTESIAN_POINT('Origin',(83.0491683351188,0.,1.95651033903146));
#30131=CARTESIAN_POINT('',(83.0491683351188,15.,1.95651033903146));
#30132=CARTESIAN_POINT('',(82.7745841675594,15.,1.95651033903146));
#30133=CARTESIAN_POINT('',(83.0491683351188,495.,1.95651033903146));
#30134=CARTESIAN_POINT('',(83.0491683351188,0.,1.95651033903146));
#30135=CARTESIAN_POINT('',(83.0491683351188,495.,1.95651033903146));
#30136=CARTESIAN_POINT('Origin',(83.0491683351188,0.,5.44638293630937));
#30137=CARTESIAN_POINT('',(83.0491683351188,15.,5.44638293630937));
#30138=CARTESIAN_POINT('',(83.0491683351188,15.,6.47319146815469));
#30139=CARTESIAN_POINT('',(83.0491683351188,495.,5.44638293630937));
#30140=CARTESIAN_POINT('',(83.0491683351188,0.,5.44638293630937));
#30141=CARTESIAN_POINT('',(83.0491683351188,495.,6.95083166488121));
#30142=CARTESIAN_POINT('Origin',(79.284340547757,0.,9.25));
#30143=CARTESIAN_POINT('',(80.5174923052273,15.,8.00414299624016));
#30144=CARTESIAN_POINT('',(83.0491683351188,495.,5.44638293630937));
#30145=CARTESIAN_POINT('Origin',(64.9508316648812,0.,28.0434896609685));
#30146=CARTESIAN_POINT('',(64.9508316648812,15.,28.0434896609685));
#30147=CARTESIAN_POINT('',(64.9508316648812,15.,23.0491683351188));
#30148=CARTESIAN_POINT('',(64.9508316648812,15.,25.2717448304843));
#30149=CARTESIAN_POINT('',(64.9508316648812,495.,28.0434896609685));
#30150=CARTESIAN_POINT('',(64.9508316648812,0.,28.0434896609685));
#30151=CARTESIAN_POINT('',(64.9508316648812,495.,23.0491683351188));
#30152=CARTESIAN_POINT('',(64.9508316648812,495.,23.0491683351188));
#30153=CARTESIAN_POINT('',(64.9508316648812,0.,23.0491683351188));
#30154=CARTESIAN_POINT('Origin',(64.9508316648812,0.,23.0491683351188));
#30155=CARTESIAN_POINT('',(65.6258960932749,15.,23.0491683351188));
#30156=CARTESIAN_POINT('',(66.2254158324406,15.,23.0491683351188));
#30157=CARTESIAN_POINT('',(65.6258960932749,495.,23.0491683351188));
#30158=CARTESIAN_POINT('',(66.9508316648812,495.,23.0491683351188));
#30159=CARTESIAN_POINT('',(65.6258960932749,0.,23.0491683351188));
#30160=CARTESIAN_POINT('Origin',(65.6258960932749,0.,23.0491683351188));
#30161=CARTESIAN_POINT('',(69.25,15.,19.3877250397624));
#30162=CARTESIAN_POINT('',(66.2269045529402,15.,22.4419676444844));
#30163=CARTESIAN_POINT('',(69.25,495.,19.3877250397624));
#30164=CARTESIAN_POINT('',(65.6258960932749,495.,23.0491683351188));
#30165=CARTESIAN_POINT('',(69.25,0.,19.3877250397624));
#30166=CARTESIAN_POINT('Origin',(69.25,0.,19.3877250397624));
#30167=CARTESIAN_POINT('',(69.25,15.,9.05613748011882));
#30168=CARTESIAN_POINT('',(69.25,495.,20.75));
#30169=CARTESIAN_POINT('Origin',(69.936778624571,0.,29.0217448304843));
#30170=CARTESIAN_POINT('',(69.936778624571,15.,29.0217448304843));
#30171=CARTESIAN_POINT('',(69.936778624571,15.,30.));
#30172=CARTESIAN_POINT('',(69.936778624571,15.,25.7608724152421));
#30173=CARTESIAN_POINT('',(69.936778624571,495.,29.0217448304843));
#30174=CARTESIAN_POINT('',(69.936778624571,0.,29.0217448304843));
#30175=CARTESIAN_POINT('',(69.936778624571,495.,30.));
#30176=CARTESIAN_POINT('',(69.936778624571,495.,29.0217448304843));
#30177=CARTESIAN_POINT('',(69.936778624571,0.,30.));
#30178=CARTESIAN_POINT('Origin',(70.7975927840689,0.,29.0217448304843));
#30179=CARTESIAN_POINT('',(70.7975927840689,15.,29.0217448304843));
#30180=CARTESIAN_POINT('',(69.1487963920345,15.,29.0217448304843));
#30181=CARTESIAN_POINT('',(70.7975927840689,495.,29.0217448304843));
#30182=CARTESIAN_POINT('',(70.7975927840689,0.,29.0217448304843));
#30183=CARTESIAN_POINT('',(70.7975927840689,495.,29.0217448304843));
#30184=CARTESIAN_POINT('Origin',(70.7975927840689,0.,28.0434896609685));
#30185=CARTESIAN_POINT('',(70.7975927840689,15.,28.0434896609685));
#30186=CARTESIAN_POINT('',(70.7975927840689,15.,25.2717448304843));
#30187=CARTESIAN_POINT('',(70.7975927840689,495.,28.0434896609685));
#30188=CARTESIAN_POINT('',(70.7975927840689,0.,28.0434896609685));
#30189=CARTESIAN_POINT('',(70.7975927840689,495.,28.0434896609685));
#30190=CARTESIAN_POINT('Origin',(66.9508316648812,0.,28.0434896609685));
#30191=CARTESIAN_POINT('',(66.9508316648812,15.,28.0434896609685));
#30192=CARTESIAN_POINT('',(67.2254158324406,15.,28.0434896609685));
#30193=CARTESIAN_POINT('',(66.9508316648812,495.,28.0434896609685));
#30194=CARTESIAN_POINT('',(66.9508316648812,0.,28.0434896609685));
#30195=CARTESIAN_POINT('',(66.9508316648812,495.,28.0434896609685));
#30196=CARTESIAN_POINT('Origin',(66.9508316648812,0.,24.5536170636906));
#30197=CARTESIAN_POINT('',(66.9508316648812,15.,24.5536170636906));
#30198=CARTESIAN_POINT('',(66.9508316648812,15.,23.5268085318453));
#30199=CARTESIAN_POINT('',(66.9508316648812,495.,24.5536170636906));
#30200=CARTESIAN_POINT('',(66.9508316648812,0.,24.5536170636906));
#30201=CARTESIAN_POINT('',(66.9508316648812,495.,23.0491683351188));
#30202=CARTESIAN_POINT('Origin',(70.715659452243,0.,20.75));
#30203=CARTESIAN_POINT('',(70.715659452243,15.,20.75));
#30204=CARTESIAN_POINT('',(69.4825076947727,15.,21.9958570037598));
#30205=CARTESIAN_POINT('',(70.715659452243,495.,20.75));
#30206=CARTESIAN_POINT('',(70.715659452243,0.,20.75));
#30207=CARTESIAN_POINT('',(66.9508316648812,495.,24.5536170636906));
#30208=CARTESIAN_POINT('Origin',(90.,0.,28.0434896609685));
#30209=CARTESIAN_POINT('',(85.0491683351188,15.,28.0434896609685));
#30210=CARTESIAN_POINT('',(86.25,15.,28.0434896609685));
#30211=CARTESIAN_POINT('',(85.0491683351188,495.,28.0434896609685));
#30212=CARTESIAN_POINT('',(85.0491683351188,0.,28.0434896609685));
#30213=CARTESIAN_POINT('',(96.9508316648812,495.,28.0434896609685));
#30214=CARTESIAN_POINT('Origin',(85.0491683351188,0.,28.0434896609685));
#30215=CARTESIAN_POINT('',(85.0491683351188,15.,23.0491683351188));
#30216=CARTESIAN_POINT('',(85.0491683351188,15.,25.2717448304843));
#30217=CARTESIAN_POINT('',(85.0491683351188,495.,23.0491683351188));
#30218=CARTESIAN_POINT('',(85.0491683351188,0.,23.0491683351188));
#30219=CARTESIAN_POINT('',(85.0491683351188,495.,23.0491683351188));
#30220=CARTESIAN_POINT('Origin',(85.0491683351188,0.,23.0491683351188));
#30221=CARTESIAN_POINT('',(84.3741039067251,15.,23.0491683351188));
#30222=CARTESIAN_POINT('',(83.7745841675594,15.,23.0491683351188));
#30223=CARTESIAN_POINT('',(84.3741039067251,495.,23.0491683351188));
#30224=CARTESIAN_POINT('',(84.3741039067251,0.,23.0491683351188));
#30225=CARTESIAN_POINT('',(83.0491683351188,495.,23.0491683351188));
#30226=CARTESIAN_POINT('Origin',(84.3741039067251,0.,23.0491683351188));
#30227=CARTESIAN_POINT('',(80.75,15.,19.3877250397624));
#30228=CARTESIAN_POINT('',(83.7730954470598,15.,22.4419676444844));
#30229=CARTESIAN_POINT('',(80.75,495.,19.3877250397624));
#30230=CARTESIAN_POINT('',(80.75,0.,19.3877250397624));
#30231=CARTESIAN_POINT('',(84.3741039067251,495.,23.0491683351188));
#30232=CARTESIAN_POINT('Origin',(80.75,0.,19.3877250397624));
#30233=CARTESIAN_POINT('',(80.75,15.,9.05613748011882));
#30234=CARTESIAN_POINT('',(80.75,495.,20.75));
#30235=CARTESIAN_POINT('Origin',(75.,0.,15.));
#30236=CARTESIAN_POINT('',(71.75,495.,15.));
#30237=CARTESIAN_POINT('Origin',(75.,495.,15.));
#30238=CARTESIAN_POINT('',(71.75,15.,15.));
#30239=CARTESIAN_POINT('',(71.75,0.,15.));
#30240=CARTESIAN_POINT('Origin',(75.,15.,15.));
#30241=CARTESIAN_POINT('Origin',(75.,0.,20.75));
#30242=CARTESIAN_POINT('',(79.284340547757,15.,20.75));
#30243=CARTESIAN_POINT('',(78.75,15.,20.75));
#30244=CARTESIAN_POINT('',(79.284340547757,495.,20.75));
#30245=CARTESIAN_POINT('',(79.284340547757,0.,20.75));
#30246=CARTESIAN_POINT('',(80.75,495.,20.75));
#30247=CARTESIAN_POINT('Origin',(80.063221375429,0.,30.));
#30248=CARTESIAN_POINT('',(80.063221375429,15.,30.));
#30249=CARTESIAN_POINT('',(98.7183893122855,15.,30.));
#30250=CARTESIAN_POINT('',(80.063221375429,495.,30.));
#30251=CARTESIAN_POINT('',(75.,495.,30.));
#30252=CARTESIAN_POINT('',(80.063221375429,0.,30.));
#30253=CARTESIAN_POINT('Origin',(80.063221375429,0.,29.0217448304843));
#30254=CARTESIAN_POINT('',(80.063221375429,15.,29.0217448304843));
#30255=CARTESIAN_POINT('',(80.063221375429,15.,25.7608724152421));
#30256=CARTESIAN_POINT('',(80.063221375429,495.,29.0217448304843));
#30257=CARTESIAN_POINT('',(80.063221375429,495.,29.0217448304843));
#30258=CARTESIAN_POINT('',(80.063221375429,0.,29.0217448304843));
#30259=CARTESIAN_POINT('Origin',(79.2024072159311,0.,29.0217448304843));
#30260=CARTESIAN_POINT('',(79.2024072159311,15.,29.0217448304843));
#30261=CARTESIAN_POINT('',(80.8512036079655,15.,29.0217448304843));
#30262=CARTESIAN_POINT('',(79.2024072159311,495.,29.0217448304843));
#30263=CARTESIAN_POINT('',(79.2024072159311,495.,29.0217448304843));
#30264=CARTESIAN_POINT('',(79.2024072159311,0.,29.0217448304843));
#30265=CARTESIAN_POINT('Origin',(79.2024072159311,0.,28.0434896609685));
#30266=CARTESIAN_POINT('',(79.2024072159311,15.,28.0434896609685));
#30267=CARTESIAN_POINT('',(79.2024072159311,15.,25.2717448304843));
#30268=CARTESIAN_POINT('',(79.2024072159311,495.,28.0434896609685));
#30269=CARTESIAN_POINT('',(79.2024072159311,495.,28.0434896609685));
#30270=CARTESIAN_POINT('',(79.2024072159311,0.,28.0434896609685));
#30271=CARTESIAN_POINT('Origin',(83.0491683351188,0.,28.0434896609685));
#30272=CARTESIAN_POINT('',(83.0491683351188,15.,28.0434896609685));
#30273=CARTESIAN_POINT('',(82.7745841675594,15.,28.0434896609685));
#30274=CARTESIAN_POINT('',(83.0491683351188,495.,28.0434896609685));
#30275=CARTESIAN_POINT('',(83.0491683351188,495.,28.0434896609685));
#30276=CARTESIAN_POINT('',(83.0491683351188,0.,28.0434896609685));
#30277=CARTESIAN_POINT('Origin',(83.0491683351188,0.,24.5536170636906));
#30278=CARTESIAN_POINT('',(83.0491683351188,15.,24.5536170636906));
#30279=CARTESIAN_POINT('',(83.0491683351188,15.,23.5268085318453));
#30280=CARTESIAN_POINT('',(83.0491683351188,495.,24.5536170636906));
#30281=CARTESIAN_POINT('',(83.0491683351188,495.,23.0491683351188));
#30282=CARTESIAN_POINT('',(83.0491683351188,0.,24.5536170636906));
#30283=CARTESIAN_POINT('Origin',(79.284340547757,0.,20.75));
#30284=CARTESIAN_POINT('',(80.5174923052273,15.,21.9958570037598));
#30285=CARTESIAN_POINT('',(83.0491683351188,495.,24.5536170636906));
#30286=CARTESIAN_POINT('Origin',(34.9508316648812,0.,1.95651033903146));
#30287=CARTESIAN_POINT('',(34.9508316648812,15.,1.95651033903146));
#30288=CARTESIAN_POINT('',(34.9508316648812,15.,6.95083166488121));
#30289=CARTESIAN_POINT('',(34.9508316648812,15.,4.72825516951573));
#30290=CARTESIAN_POINT('',(34.9508316648812,495.,6.95083166488121));
#30291=CARTESIAN_POINT('',(34.9508316648812,0.,6.95083166488121));
#30292=CARTESIAN_POINT('',(34.9508316648812,495.,1.95651033903146));
#30293=CARTESIAN_POINT('',(34.9508316648812,495.,6.95083166488121));
#30294=CARTESIAN_POINT('',(34.9508316648812,0.,1.95651033903146));
#30295=CARTESIAN_POINT('Origin',(34.9508316648812,0.,6.95083166488121));
#30296=CARTESIAN_POINT('',(35.6258960932749,15.,6.95083166488121));
#30297=CARTESIAN_POINT('',(36.2254158324406,15.,6.95083166488121));
#30298=CARTESIAN_POINT('',(35.6258960932749,495.,6.95083166488121));
#30299=CARTESIAN_POINT('',(35.6258960932749,0.,6.95083166488121));
#30300=CARTESIAN_POINT('',(36.9508316648812,495.,6.95083166488121));
#30301=CARTESIAN_POINT('Origin',(35.6258960932749,0.,6.95083166488121));
#30302=CARTESIAN_POINT('',(39.25,15.,10.6122749602376));
#30303=CARTESIAN_POINT('',(36.2269045529402,15.,7.55803235551558));
#30304=CARTESIAN_POINT('',(39.25,495.,10.6122749602376));
#30305=CARTESIAN_POINT('',(39.25,0.,10.6122749602376));
#30306=CARTESIAN_POINT('',(35.6258960932749,495.,6.95083166488121));
#30307=CARTESIAN_POINT('Origin',(39.936778624571,0.,0.978255169515729));
#30308=CARTESIAN_POINT('',(39.936778624571,15.,0.978255169515729));
#30309=CARTESIAN_POINT('',(39.936778624571,15.,0.));
#30310=CARTESIAN_POINT('',(39.936778624571,15.,4.23912758475787));
#30311=CARTESIAN_POINT('',(39.936778624571,495.,0.));
#30312=CARTESIAN_POINT('',(39.936778624571,0.,0.));
#30313=CARTESIAN_POINT('',(39.936778624571,495.,0.978255169515729));
#30314=CARTESIAN_POINT('',(39.936778624571,495.,0.978255169515729));
#30315=CARTESIAN_POINT('',(39.936778624571,0.,0.978255169515729));
#30316=CARTESIAN_POINT('Origin',(40.7975927840689,0.,0.978255169515729));
#30317=CARTESIAN_POINT('',(40.7975927840689,15.,0.978255169515729));
#30318=CARTESIAN_POINT('',(39.1487963920345,15.,0.978255169515729));
#30319=CARTESIAN_POINT('',(40.7975927840689,495.,0.978255169515729));
#30320=CARTESIAN_POINT('',(40.7975927840689,495.,0.978255169515729));
#30321=CARTESIAN_POINT('',(40.7975927840689,0.,0.978255169515729));
#30322=CARTESIAN_POINT('Origin',(40.7975927840689,0.,1.95651033903146));
#30323=CARTESIAN_POINT('',(40.7975927840689,15.,1.95651033903146));
#30324=CARTESIAN_POINT('',(40.7975927840689,15.,4.72825516951573));
#30325=CARTESIAN_POINT('',(40.7975927840689,495.,1.95651033903146));
#30326=CARTESIAN_POINT('',(40.7975927840689,495.,1.95651033903146));
#30327=CARTESIAN_POINT('',(40.7975927840689,0.,1.95651033903146));
#30328=CARTESIAN_POINT('Origin',(36.9508316648812,0.,1.95651033903146));
#30329=CARTESIAN_POINT('',(36.9508316648812,15.,1.95651033903146));
#30330=CARTESIAN_POINT('',(37.2254158324406,15.,1.95651033903146));
#30331=CARTESIAN_POINT('',(36.9508316648812,495.,1.95651033903146));
#30332=CARTESIAN_POINT('',(36.9508316648812,495.,1.95651033903146));
#30333=CARTESIAN_POINT('',(36.9508316648812,0.,1.95651033903146));
#30334=CARTESIAN_POINT('Origin',(36.9508316648812,0.,5.44638293630937));
#30335=CARTESIAN_POINT('',(36.9508316648812,15.,5.44638293630937));
#30336=CARTESIAN_POINT('',(36.9508316648812,15.,6.47319146815469));
#30337=CARTESIAN_POINT('',(36.9508316648812,495.,5.44638293630937));
#30338=CARTESIAN_POINT('',(36.9508316648812,495.,6.95083166488121));
#30339=CARTESIAN_POINT('',(36.9508316648812,0.,5.44638293630937));
#30340=CARTESIAN_POINT('Origin',(40.715659452243,0.,9.25));
#30341=CARTESIAN_POINT('',(40.715659452243,15.,9.25));
#30342=CARTESIAN_POINT('',(39.4825076947727,15.,8.00414299624016));
#30343=CARTESIAN_POINT('',(40.715659452243,495.,9.25));
#30344=CARTESIAN_POINT('',(36.9508316648812,495.,5.44638293630937));
#30345=CARTESIAN_POINT('',(40.715659452243,0.,9.25));
#30346=CARTESIAN_POINT('Origin',(60.,0.,1.95651033903146));
#30347=CARTESIAN_POINT('',(55.0491683351188,15.,1.95651033903146));
#30348=CARTESIAN_POINT('',(56.25,15.,1.95651033903146));
#30349=CARTESIAN_POINT('',(55.0491683351188,495.,1.95651033903146));
#30350=CARTESIAN_POINT('',(53.0491683351188,495.,1.95651033903146));
#30351=CARTESIAN_POINT('',(55.0491683351188,0.,1.95651033903146));
#30352=CARTESIAN_POINT('Origin',(55.0491683351188,0.,1.95651033903146));
#30353=CARTESIAN_POINT('',(55.0491683351188,15.,6.95083166488121));
#30354=CARTESIAN_POINT('',(55.0491683351188,15.,4.72825516951573));
#30355=CARTESIAN_POINT('',(55.0491683351188,495.,6.95083166488121));
#30356=CARTESIAN_POINT('',(55.0491683351188,495.,6.95083166488121));
#30357=CARTESIAN_POINT('',(55.0491683351188,0.,6.95083166488121));
#30358=CARTESIAN_POINT('Origin',(55.0491683351188,0.,6.95083166488121));
#30359=CARTESIAN_POINT('',(54.3741039067251,15.,6.95083166488121));
#30360=CARTESIAN_POINT('',(53.7745841675594,15.,6.95083166488121));
#30361=CARTESIAN_POINT('',(54.3741039067251,495.,6.95083166488121));
#30362=CARTESIAN_POINT('',(53.0491683351188,495.,6.95083166488121));
#30363=CARTESIAN_POINT('',(54.3741039067251,0.,6.95083166488121));
#30364=CARTESIAN_POINT('Origin',(54.3741039067251,0.,6.95083166488121));
#30365=CARTESIAN_POINT('',(50.75,15.,10.6122749602376));
#30366=CARTESIAN_POINT('',(53.7730954470598,15.,7.55803235551558));
#30367=CARTESIAN_POINT('',(50.75,495.,10.6122749602376));
#30368=CARTESIAN_POINT('',(54.3741039067251,495.,6.95083166488121));
#30369=CARTESIAN_POINT('',(50.75,0.,10.6122749602376));
#30370=CARTESIAN_POINT('Origin',(45.,0.,9.25));
#30371=CARTESIAN_POINT('',(49.284340547757,15.,9.25));
#30372=CARTESIAN_POINT('',(48.75,15.,9.25));
#30373=CARTESIAN_POINT('',(49.284340547757,495.,9.25));
#30374=CARTESIAN_POINT('',(50.75,495.,9.25));
#30375=CARTESIAN_POINT('',(49.284340547757,0.,9.25));
#30376=CARTESIAN_POINT('Origin',(50.063221375429,0.,0.));
#30377=CARTESIAN_POINT('',(50.063221375429,15.,0.));
#30378=CARTESIAN_POINT('',(68.7183893122855,15.,0.));
#30379=CARTESIAN_POINT('',(50.063221375429,495.,0.));
#30380=CARTESIAN_POINT('',(50.063221375429,0.,0.));
#30381=CARTESIAN_POINT('',(45.,495.,0.));
#30382=CARTESIAN_POINT('Origin',(50.063221375429,0.,0.978255169515729));
#30383=CARTESIAN_POINT('',(50.063221375429,15.,0.978255169515729));
#30384=CARTESIAN_POINT('',(50.063221375429,15.,4.23912758475787));
#30385=CARTESIAN_POINT('',(50.063221375429,495.,0.978255169515729));
#30386=CARTESIAN_POINT('',(50.063221375429,0.,0.978255169515729));
#30387=CARTESIAN_POINT('',(50.063221375429,495.,0.978255169515729));
#30388=CARTESIAN_POINT('Origin',(49.2024072159311,0.,0.978255169515729));
#30389=CARTESIAN_POINT('',(49.2024072159311,15.,0.978255169515729));
#30390=CARTESIAN_POINT('',(50.8512036079655,15.,0.978255169515729));
#30391=CARTESIAN_POINT('',(49.2024072159311,495.,0.978255169515729));
#30392=CARTESIAN_POINT('',(49.2024072159311,0.,0.978255169515729));
#30393=CARTESIAN_POINT('',(49.2024072159311,495.,0.978255169515729));
#30394=CARTESIAN_POINT('Origin',(49.2024072159311,0.,1.95651033903146));
#30395=CARTESIAN_POINT('',(49.2024072159311,15.,1.95651033903146));
#30396=CARTESIAN_POINT('',(49.2024072159311,15.,4.72825516951573));
#30397=CARTESIAN_POINT('',(49.2024072159311,495.,1.95651033903146));
#30398=CARTESIAN_POINT('',(49.2024072159311,0.,1.95651033903146));
#30399=CARTESIAN_POINT('',(49.2024072159311,495.,1.95651033903146));
#30400=CARTESIAN_POINT('Origin',(53.0491683351188,0.,1.95651033903146));
#30401=CARTESIAN_POINT('',(53.0491683351188,15.,1.95651033903146));
#30402=CARTESIAN_POINT('',(52.7745841675594,15.,1.95651033903146));
#30403=CARTESIAN_POINT('',(53.0491683351188,495.,1.95651033903146));
#30404=CARTESIAN_POINT('',(53.0491683351188,0.,1.95651033903146));
#30405=CARTESIAN_POINT('',(53.0491683351188,495.,1.95651033903146));
#30406=CARTESIAN_POINT('Origin',(53.0491683351188,0.,5.44638293630937));
#30407=CARTESIAN_POINT('',(53.0491683351188,15.,5.44638293630937));
#30408=CARTESIAN_POINT('',(53.0491683351188,15.,6.47319146815469));
#30409=CARTESIAN_POINT('',(53.0491683351188,495.,5.44638293630937));
#30410=CARTESIAN_POINT('',(53.0491683351188,0.,5.44638293630937));
#30411=CARTESIAN_POINT('',(53.0491683351188,495.,6.95083166488121));
#30412=CARTESIAN_POINT('Origin',(49.284340547757,0.,9.25));
#30413=CARTESIAN_POINT('',(50.5174923052273,15.,8.00414299624016));
#30414=CARTESIAN_POINT('',(53.0491683351188,495.,5.44638293630937));
#30415=CARTESIAN_POINT('Origin',(34.9508316648812,0.,28.0434896609685));
#30416=CARTESIAN_POINT('',(34.9508316648812,15.,28.0434896609685));
#30417=CARTESIAN_POINT('',(34.9508316648812,15.,23.0491683351188));
#30418=CARTESIAN_POINT('',(34.9508316648812,15.,25.2717448304843));
#30419=CARTESIAN_POINT('',(34.9508316648812,495.,28.0434896609685));
#30420=CARTESIAN_POINT('',(34.9508316648812,0.,28.0434896609685));
#30421=CARTESIAN_POINT('',(34.9508316648812,495.,23.0491683351188));
#30422=CARTESIAN_POINT('',(34.9508316648812,495.,23.0491683351188));
#30423=CARTESIAN_POINT('',(34.9508316648812,0.,23.0491683351188));
#30424=CARTESIAN_POINT('Origin',(34.9508316648812,0.,23.0491683351188));
#30425=CARTESIAN_POINT('',(35.6258960932749,15.,23.0491683351188));
#30426=CARTESIAN_POINT('',(36.2254158324406,15.,23.0491683351188));
#30427=CARTESIAN_POINT('',(35.6258960932749,495.,23.0491683351188));
#30428=CARTESIAN_POINT('',(36.9508316648812,495.,23.0491683351188));
#30429=CARTESIAN_POINT('',(35.6258960932749,0.,23.0491683351188));
#30430=CARTESIAN_POINT('Origin',(35.6258960932749,0.,23.0491683351188));
#30431=CARTESIAN_POINT('',(39.25,15.,19.3877250397624));
#30432=CARTESIAN_POINT('',(36.2269045529402,15.,22.4419676444844));
#30433=CARTESIAN_POINT('',(39.25,495.,19.3877250397624));
#30434=CARTESIAN_POINT('',(35.6258960932749,495.,23.0491683351188));
#30435=CARTESIAN_POINT('',(39.25,0.,19.3877250397624));
#30436=CARTESIAN_POINT('Origin',(39.25,0.,19.3877250397624));
#30437=CARTESIAN_POINT('',(39.25,15.,9.05613748011882));
#30438=CARTESIAN_POINT('',(39.25,495.,20.75));
#30439=CARTESIAN_POINT('Origin',(39.936778624571,0.,29.0217448304843));
#30440=CARTESIAN_POINT('',(39.936778624571,15.,29.0217448304843));
#30441=CARTESIAN_POINT('',(39.936778624571,15.,30.));
#30442=CARTESIAN_POINT('',(39.936778624571,15.,25.7608724152421));
#30443=CARTESIAN_POINT('',(39.936778624571,495.,29.0217448304843));
#30444=CARTESIAN_POINT('',(39.936778624571,0.,29.0217448304843));
#30445=CARTESIAN_POINT('',(39.936778624571,495.,30.));
#30446=CARTESIAN_POINT('',(39.936778624571,495.,29.0217448304843));
#30447=CARTESIAN_POINT('',(39.936778624571,0.,30.));
#30448=CARTESIAN_POINT('Origin',(40.7975927840689,0.,29.0217448304843));
#30449=CARTESIAN_POINT('',(40.7975927840689,15.,29.0217448304843));
#30450=CARTESIAN_POINT('',(39.1487963920345,15.,29.0217448304843));
#30451=CARTESIAN_POINT('',(40.7975927840689,495.,29.0217448304843));
#30452=CARTESIAN_POINT('',(40.7975927840689,0.,29.0217448304843));
#30453=CARTESIAN_POINT('',(40.7975927840689,495.,29.0217448304843));
#30454=CARTESIAN_POINT('Origin',(40.7975927840689,0.,28.0434896609685));
#30455=CARTESIAN_POINT('',(40.7975927840689,15.,28.0434896609685));
#30456=CARTESIAN_POINT('',(40.7975927840689,15.,25.2717448304843));
#30457=CARTESIAN_POINT('',(40.7975927840689,495.,28.0434896609685));
#30458=CARTESIAN_POINT('',(40.7975927840689,0.,28.0434896609685));
#30459=CARTESIAN_POINT('',(40.7975927840689,495.,28.0434896609685));
#30460=CARTESIAN_POINT('Origin',(36.9508316648812,0.,28.0434896609685));
#30461=CARTESIAN_POINT('',(36.9508316648812,15.,28.0434896609685));
#30462=CARTESIAN_POINT('',(37.2254158324406,15.,28.0434896609685));
#30463=CARTESIAN_POINT('',(36.9508316648812,495.,28.0434896609685));
#30464=CARTESIAN_POINT('',(36.9508316648812,0.,28.0434896609685));
#30465=CARTESIAN_POINT('',(36.9508316648812,495.,28.0434896609685));
#30466=CARTESIAN_POINT('Origin',(36.9508316648812,0.,24.5536170636906));
#30467=CARTESIAN_POINT('',(36.9508316648812,15.,24.5536170636906));
#30468=CARTESIAN_POINT('',(36.9508316648812,15.,23.5268085318453));
#30469=CARTESIAN_POINT('',(36.9508316648812,495.,24.5536170636906));
#30470=CARTESIAN_POINT('',(36.9508316648812,0.,24.5536170636906));
#30471=CARTESIAN_POINT('',(36.9508316648812,495.,23.0491683351188));
#30472=CARTESIAN_POINT('Origin',(40.715659452243,0.,20.75));
#30473=CARTESIAN_POINT('',(40.715659452243,15.,20.75));
#30474=CARTESIAN_POINT('',(39.4825076947727,15.,21.9958570037598));
#30475=CARTESIAN_POINT('',(40.715659452243,495.,20.75));
#30476=CARTESIAN_POINT('',(40.715659452243,0.,20.75));
#30477=CARTESIAN_POINT('',(36.9508316648812,495.,24.5536170636906));
#30478=CARTESIAN_POINT('Origin',(60.,0.,28.0434896609685));
#30479=CARTESIAN_POINT('',(55.0491683351188,15.,28.0434896609685));
#30480=CARTESIAN_POINT('',(56.25,15.,28.0434896609685));
#30481=CARTESIAN_POINT('',(55.0491683351188,495.,28.0434896609685));
#30482=CARTESIAN_POINT('',(55.0491683351188,0.,28.0434896609685));
#30483=CARTESIAN_POINT('',(66.9508316648812,495.,28.0434896609685));
#30484=CARTESIAN_POINT('Origin',(55.0491683351188,0.,28.0434896609685));
#30485=CARTESIAN_POINT('',(55.0491683351188,15.,23.0491683351188));
#30486=CARTESIAN_POINT('',(55.0491683351188,15.,25.2717448304843));
#30487=CARTESIAN_POINT('',(55.0491683351188,495.,23.0491683351188));
#30488=CARTESIAN_POINT('',(55.0491683351188,0.,23.0491683351188));
#30489=CARTESIAN_POINT('',(55.0491683351188,495.,23.0491683351188));
#30490=CARTESIAN_POINT('Origin',(55.0491683351188,0.,23.0491683351188));
#30491=CARTESIAN_POINT('',(54.3741039067251,15.,23.0491683351188));
#30492=CARTESIAN_POINT('',(53.7745841675594,15.,23.0491683351188));
#30493=CARTESIAN_POINT('',(54.3741039067251,495.,23.0491683351188));
#30494=CARTESIAN_POINT('',(54.3741039067251,0.,23.0491683351188));
#30495=CARTESIAN_POINT('',(53.0491683351188,495.,23.0491683351188));
#30496=CARTESIAN_POINT('Origin',(54.3741039067251,0.,23.0491683351188));
#30497=CARTESIAN_POINT('',(50.75,15.,19.3877250397624));
#30498=CARTESIAN_POINT('',(53.7730954470598,15.,22.4419676444844));
#30499=CARTESIAN_POINT('',(50.75,495.,19.3877250397624));
#30500=CARTESIAN_POINT('',(50.75,0.,19.3877250397624));
#30501=CARTESIAN_POINT('',(54.3741039067251,495.,23.0491683351188));
#30502=CARTESIAN_POINT('Origin',(50.75,0.,19.3877250397624));
#30503=CARTESIAN_POINT('',(50.75,15.,9.05613748011882));
#30504=CARTESIAN_POINT('',(50.75,495.,20.75));
#30505=CARTESIAN_POINT('Origin',(45.,0.,15.));
#30506=CARTESIAN_POINT('',(41.75,495.,15.));
#30507=CARTESIAN_POINT('Origin',(45.,495.,15.));
#30508=CARTESIAN_POINT('',(41.75,15.,15.));
#30509=CARTESIAN_POINT('',(41.75,0.,15.));
#30510=CARTESIAN_POINT('Origin',(45.,15.,15.));
#30511=CARTESIAN_POINT('Origin',(45.,0.,20.75));
#30512=CARTESIAN_POINT('',(49.284340547757,15.,20.75));
#30513=CARTESIAN_POINT('',(48.75,15.,20.75));
#30514=CARTESIAN_POINT('',(49.284340547757,495.,20.75));
#30515=CARTESIAN_POINT('',(49.284340547757,0.,20.75));
#30516=CARTESIAN_POINT('',(50.75,495.,20.75));
#30517=CARTESIAN_POINT('Origin',(50.063221375429,0.,30.));
#30518=CARTESIAN_POINT('',(50.063221375429,15.,30.));
#30519=CARTESIAN_POINT('',(68.7183893122855,15.,30.));
#30520=CARTESIAN_POINT('',(50.063221375429,495.,30.));
#30521=CARTESIAN_POINT('',(45.,495.,30.));
#30522=CARTESIAN_POINT('',(50.063221375429,0.,30.));
#30523=CARTESIAN_POINT('Origin',(50.063221375429,0.,29.0217448304843));
#30524=CARTESIAN_POINT('',(50.063221375429,15.,29.0217448304843));
#30525=CARTESIAN_POINT('',(50.063221375429,15.,25.7608724152421));
#30526=CARTESIAN_POINT('',(50.063221375429,495.,29.0217448304843));
#30527=CARTESIAN_POINT('',(50.063221375429,495.,29.0217448304843));
#30528=CARTESIAN_POINT('',(50.063221375429,0.,29.0217448304843));
#30529=CARTESIAN_POINT('Origin',(49.2024072159311,0.,29.0217448304843));
#30530=CARTESIAN_POINT('',(49.2024072159311,15.,29.0217448304843));
#30531=CARTESIAN_POINT('',(50.8512036079655,15.,29.0217448304843));
#30532=CARTESIAN_POINT('',(49.2024072159311,495.,29.0217448304843));
#30533=CARTESIAN_POINT('',(49.2024072159311,495.,29.0217448304843));
#30534=CARTESIAN_POINT('',(49.2024072159311,0.,29.0217448304843));
#30535=CARTESIAN_POINT('Origin',(49.2024072159311,0.,28.0434896609685));
#30536=CARTESIAN_POINT('',(49.2024072159311,15.,28.0434896609685));
#30537=CARTESIAN_POINT('',(49.2024072159311,15.,25.2717448304843));
#30538=CARTESIAN_POINT('',(49.2024072159311,495.,28.0434896609685));
#30539=CARTESIAN_POINT('',(49.2024072159311,495.,28.0434896609685));
#30540=CARTESIAN_POINT('',(49.2024072159311,0.,28.0434896609685));
#30541=CARTESIAN_POINT('Origin',(53.0491683351188,0.,28.0434896609685));
#30542=CARTESIAN_POINT('',(53.0491683351188,15.,28.0434896609685));
#30543=CARTESIAN_POINT('',(52.7745841675594,15.,28.0434896609685));
#30544=CARTESIAN_POINT('',(53.0491683351188,495.,28.0434896609685));
#30545=CARTESIAN_POINT('',(53.0491683351188,495.,28.0434896609685));
#30546=CARTESIAN_POINT('',(53.0491683351188,0.,28.0434896609685));
#30547=CARTESIAN_POINT('Origin',(53.0491683351188,0.,24.5536170636906));
#30548=CARTESIAN_POINT('',(53.0491683351188,15.,24.5536170636906));
#30549=CARTESIAN_POINT('',(53.0491683351188,15.,23.5268085318453));
#30550=CARTESIAN_POINT('',(53.0491683351188,495.,24.5536170636906));
#30551=CARTESIAN_POINT('',(53.0491683351188,495.,23.0491683351188));
#30552=CARTESIAN_POINT('',(53.0491683351188,0.,24.5536170636906));
#30553=CARTESIAN_POINT('Origin',(49.284340547757,0.,20.75));
#30554=CARTESIAN_POINT('',(50.5174923052273,15.,21.9958570037598));
#30555=CARTESIAN_POINT('',(53.0491683351188,495.,24.5536170636906));
#30556=CARTESIAN_POINT('Origin',(1.89960608334138,0.,5.18145522242933));
#30557=CARTESIAN_POINT('',(1.89960608334138,15.,5.18145522242933));
#30558=CARTESIAN_POINT('',(4.78668371362235,15.,5.18145522242933));
#30559=CARTESIAN_POINT('',(8.44980304167069,15.,5.18145522242933));
#30560=CARTESIAN_POINT('',(1.89960608334138,495.,5.18145522242933));
#30561=CARTESIAN_POINT('',(1.89960608334138,0.,5.18145522242933));
#30562=CARTESIAN_POINT('',(4.78668371362235,495.,5.18145522242933));
#30563=CARTESIAN_POINT('',(1.89960608334138,495.,5.18145522242933));
#30564=CARTESIAN_POINT('',(4.78668371362235,0.,5.18145522242933));
#30565=CARTESIAN_POINT('Origin',(4.78668371362236,0.,4.68145522242933));
#30566=CARTESIAN_POINT('',(5.28668371362236,15.,4.68145522242933));
#30567=CARTESIAN_POINT('Origin',(4.78668371362236,15.,4.68145522242933));
#30568=CARTESIAN_POINT('',(5.28668371362236,495.,4.68145522242933));
#30569=CARTESIAN_POINT('Origin',(4.78668371362236,495.,4.68145522242933));
#30570=CARTESIAN_POINT('',(5.28668371362236,0.,4.68145522242933));
#30571=CARTESIAN_POINT('Origin',(5.28668371362236,0.,4.68145522242933));
#30572=CARTESIAN_POINT('',(5.28668371362235,15.,1.81236459713887));
#30573=CARTESIAN_POINT('',(5.28668371362236,15.,6.09072761121467));
#30574=CARTESIAN_POINT('',(5.28668371362235,495.,1.81236459713887));
#30575=CARTESIAN_POINT('',(5.28668371362236,495.,4.68145522242933));
#30576=CARTESIAN_POINT('',(5.28668371362235,0.,1.81236459713887));
#30577=CARTESIAN_POINT('Origin',(4.78668371362235,0.,1.81236459713888));
#30578=CARTESIAN_POINT('',(4.78668371362235,15.,1.31236459713888));
#30579=CARTESIAN_POINT('Origin',(4.78668371362235,15.,1.81236459713888));
#30580=CARTESIAN_POINT('',(4.78668371362235,495.,1.31236459713888));
#30581=CARTESIAN_POINT('Origin',(4.78668371362235,495.,1.81236459713888));
#30582=CARTESIAN_POINT('',(4.78668371362235,0.,1.31236459713888));
#30583=CARTESIAN_POINT('Origin',(19.284340547757,0.,9.25));
#30584=CARTESIAN_POINT('',(19.284340547757,15.,9.25));
#30585=CARTESIAN_POINT('',(23.0491683351188,15.,5.44638293630937));
#30586=CARTESIAN_POINT('',(18.661711044137,15.,9.87904449767289));
#30587=CARTESIAN_POINT('',(19.284340547757,495.,9.25));
#30588=CARTESIAN_POINT('',(19.284340547757,0.,9.25));
#30589=CARTESIAN_POINT('',(23.0491683351188,495.,5.44638293630937));
#30590=CARTESIAN_POINT('',(23.0491683351188,495.,5.44638293630937));
#30591=CARTESIAN_POINT('',(23.0491683351188,0.,5.44638293630937));
#30592=CARTESIAN_POINT('Origin',(23.0491683351188,0.,5.44638293630937));
#30593=CARTESIAN_POINT('',(23.0491683351188,15.,1.95651033903146));
#30594=CARTESIAN_POINT('',(23.0491683351188,15.,6.47319146815469));
#30595=CARTESIAN_POINT('',(23.0491683351188,495.,1.95651033903146));
#30596=CARTESIAN_POINT('',(23.0491683351188,495.,6.95083166488121));
#30597=CARTESIAN_POINT('',(23.0491683351188,0.,1.95651033903146));
#30598=CARTESIAN_POINT('Origin',(23.0491683351188,0.,1.95651033903146));
#30599=CARTESIAN_POINT('',(19.2024072159311,15.,1.95651033903146));
#30600=CARTESIAN_POINT('',(19.0245841675594,15.,1.95651033903146));
#30601=CARTESIAN_POINT('',(19.2024072159311,495.,1.95651033903146));
#30602=CARTESIAN_POINT('',(23.0491683351188,495.,1.95651033903146));
#30603=CARTESIAN_POINT('',(19.2024072159311,0.,1.95651033903146));
#30604=CARTESIAN_POINT('Origin',(19.2024072159311,0.,1.95651033903146));
#30605=CARTESIAN_POINT('',(19.2024072159311,15.,0.978255169515729));
#30606=CARTESIAN_POINT('',(19.2024072159311,15.,4.72825516951573));
#30607=CARTESIAN_POINT('',(19.2024072159311,495.,0.978255169515729));
#30608=CARTESIAN_POINT('',(19.2024072159311,495.,1.95651033903146));
#30609=CARTESIAN_POINT('',(19.2024072159311,0.,0.978255169515729));
#30610=CARTESIAN_POINT('Origin',(19.2024072159311,0.,0.978255169515729));
#30611=CARTESIAN_POINT('',(20.063221375429,15.,0.978255169515729));
#30612=CARTESIAN_POINT('',(17.1012036079655,15.,0.978255169515729));
#30613=CARTESIAN_POINT('',(20.063221375429,495.,0.978255169515729));
#30614=CARTESIAN_POINT('',(19.2024072159311,495.,0.978255169515729));
#30615=CARTESIAN_POINT('',(20.063221375429,0.,0.978255169515729));
#30616=CARTESIAN_POINT('Origin',(20.063221375429,0.,0.978255169515729));
#30617=CARTESIAN_POINT('',(20.063221375429,15.,0.));
#30618=CARTESIAN_POINT('',(20.063221375429,15.,4.23912758475787));
#30619=CARTESIAN_POINT('',(20.063221375429,495.,0.));
#30620=CARTESIAN_POINT('',(20.063221375429,495.,0.978255169515729));
#30621=CARTESIAN_POINT('',(20.063221375429,0.,0.));
#30622=CARTESIAN_POINT('Origin',(20.063221375429,0.,0.));
#30623=CARTESIAN_POINT('',(38.7183893122855,15.,0.));
#30624=CARTESIAN_POINT('',(15.,495.,0.));
#30625=CARTESIAN_POINT('Origin',(30.,0.,1.95651033903146));
#30626=CARTESIAN_POINT('',(25.0491683351188,15.,1.95651033903146));
#30627=CARTESIAN_POINT('',(22.5,15.,1.95651033903146));
#30628=CARTESIAN_POINT('',(25.0491683351188,495.,1.95651033903146));
#30629=CARTESIAN_POINT('',(36.9508316648812,495.,1.95651033903146));
#30630=CARTESIAN_POINT('',(25.0491683351188,0.,1.95651033903146));
#30631=CARTESIAN_POINT('Origin',(25.0491683351188,0.,1.95651033903146));
#30632=CARTESIAN_POINT('',(25.0491683351188,15.,6.95083166488121));
#30633=CARTESIAN_POINT('',(25.0491683351188,15.,4.72825516951573));
#30634=CARTESIAN_POINT('',(25.0491683351188,495.,6.95083166488121));
#30635=CARTESIAN_POINT('',(25.0491683351188,495.,6.95083166488121));
#30636=CARTESIAN_POINT('',(25.0491683351188,0.,6.95083166488121));
#30637=CARTESIAN_POINT('Origin',(25.0491683351188,0.,6.95083166488121));
#30638=CARTESIAN_POINT('',(24.3741039067251,15.,6.95083166488121));
#30639=CARTESIAN_POINT('',(20.0245841675594,15.,6.95083166488121));
#30640=CARTESIAN_POINT('',(24.3741039067251,495.,6.95083166488121));
#30641=CARTESIAN_POINT('',(23.0491683351188,495.,6.95083166488121));
#30642=CARTESIAN_POINT('',(24.3741039067251,0.,6.95083166488121));
#30643=CARTESIAN_POINT('Origin',(24.3741039067251,0.,6.95083166488121));
#30644=CARTESIAN_POINT('',(20.75,15.,10.6122749602376));
#30645=CARTESIAN_POINT('',(21.9173141859695,15.,9.43293385694831));
#30646=CARTESIAN_POINT('',(20.75,495.,10.6122749602376));
#30647=CARTESIAN_POINT('',(24.3741039067251,495.,6.95083166488121));
#30648=CARTESIAN_POINT('',(20.75,0.,10.6122749602376));
#30649=CARTESIAN_POINT('Origin',(1.89960608334138,0.,4.68145522242933));
#30650=CARTESIAN_POINT('',(1.39960608334138,15.,4.68145522242933));
#30651=CARTESIAN_POINT('Origin',(1.89960608334138,15.,4.68145522242933));
#30652=CARTESIAN_POINT('',(1.39960608334138,495.,4.68145522242933));
#30653=CARTESIAN_POINT('',(1.39960608334138,0.,4.68145522242933));
#30654=CARTESIAN_POINT('Origin',(1.89960608334138,495.,4.68145522242933));
#30655=CARTESIAN_POINT('Origin',(1.39960608334138,0.,1.81236459713887));
#30656=CARTESIAN_POINT('',(1.39960608334138,15.,1.81236459713887));
#30657=CARTESIAN_POINT('',(1.39960608334138,15.,4.65618229856943));
#30658=CARTESIAN_POINT('',(1.39960608334138,495.,1.81236459713887));
#30659=CARTESIAN_POINT('',(1.39960608334138,0.,1.81236459713887));
#30660=CARTESIAN_POINT('',(1.39960608334138,495.,1.81236459713887));
#30661=CARTESIAN_POINT('Origin',(1.89960608334138,0.,1.81236459713888));
#30662=CARTESIAN_POINT('',(1.89960608334138,15.,1.31236459713888));
#30663=CARTESIAN_POINT('Origin',(1.89960608334138,15.,1.81236459713888));
#30664=CARTESIAN_POINT('',(1.89960608334138,495.,1.31236459713888));
#30665=CARTESIAN_POINT('',(1.89960608334138,0.,1.31236459713888));
#30666=CARTESIAN_POINT('Origin',(1.89960608334138,495.,1.81236459713888));
#30667=CARTESIAN_POINT('Origin',(4.78668371362235,0.,1.31236459713888));
#30668=CARTESIAN_POINT('',(9.89334185681118,15.,1.31236459713888));
#30669=CARTESIAN_POINT('',(4.78668371362235,495.,1.31236459713888));
#30670=CARTESIAN_POINT('Origin',(10.715659452243,0.,9.25));
#30671=CARTESIAN_POINT('',(10.715659452243,15.,9.25));
#30672=CARTESIAN_POINT('',(12.8578297261215,15.,9.25));
#30673=CARTESIAN_POINT('',(10.715659452243,495.,9.25));
#30674=CARTESIAN_POINT('',(10.715659452243,0.,9.25));
#30675=CARTESIAN_POINT('',(9.25,495.,9.25));
#30676=CARTESIAN_POINT('Origin',(6.9508316648812,0.,5.44638293630937));
#30677=CARTESIAN_POINT('',(6.9508316648812,15.,5.44638293630937));
#30678=CARTESIAN_POINT('',(9.45587506218205,15.,7.97723596582758));
#30679=CARTESIAN_POINT('',(6.9508316648812,495.,5.44638293630937));
#30680=CARTESIAN_POINT('',(6.9508316648812,0.,5.44638293630937));
#30681=CARTESIAN_POINT('',(6.9508316648812,495.,5.44638293630937));
#30682=CARTESIAN_POINT('Origin',(6.9508316648812,0.,1.95651033903146));
#30683=CARTESIAN_POINT('',(6.9508316648812,15.,1.95651033903146));
#30684=CARTESIAN_POINT('',(6.9508316648812,15.,4.72825516951573));
#30685=CARTESIAN_POINT('',(6.9508316648812,495.,1.95651033903146));
#30686=CARTESIAN_POINT('',(6.9508316648812,0.,1.95651033903146));
#30687=CARTESIAN_POINT('',(6.9508316648812,495.,6.95083166488121));
#30688=CARTESIAN_POINT('Origin',(10.7975927840689,0.,1.95651033903146));
#30689=CARTESIAN_POINT('',(10.7975927840689,15.,1.95651033903146));
#30690=CARTESIAN_POINT('',(12.8987963920345,15.,1.95651033903146));
#30691=CARTESIAN_POINT('',(10.7975927840689,495.,1.95651033903146));
#30692=CARTESIAN_POINT('',(10.7975927840689,0.,1.95651033903146));
#30693=CARTESIAN_POINT('',(9.93677862457103,495.,1.95651033903146));
#30694=CARTESIAN_POINT('Origin',(10.7975927840689,0.,0.978255169515729));
#30695=CARTESIAN_POINT('',(10.7975927840689,15.,0.978255169515729));
#30696=CARTESIAN_POINT('',(10.7975927840689,15.,4.23912758475787));
#30697=CARTESIAN_POINT('',(10.7975927840689,495.,0.978255169515729));
#30698=CARTESIAN_POINT('',(10.7975927840689,0.,0.978255169515729));
#30699=CARTESIAN_POINT('',(10.7975927840689,495.,1.95651033903146));
#30700=CARTESIAN_POINT('Origin',(9.93677862457103,0.,0.978255169515729));
#30701=CARTESIAN_POINT('',(9.93677862457103,15.,0.978255169515729));
#30702=CARTESIAN_POINT('',(12.4683893122855,15.,0.978255169515729));
#30703=CARTESIAN_POINT('',(9.93677862457103,495.,0.978255169515729));
#30704=CARTESIAN_POINT('',(9.93677862457103,0.,0.978255169515729));
#30705=CARTESIAN_POINT('',(10.7975927840689,495.,0.978255169515729));
#30706=CARTESIAN_POINT('Origin',(9.93677862457103,0.,0.));
#30707=CARTESIAN_POINT('',(9.93677862457103,15.,0.));
#30708=CARTESIAN_POINT('',(9.93677862457103,15.,3.75));
#30709=CARTESIAN_POINT('',(9.93677862457103,495.,0.));
#30710=CARTESIAN_POINT('',(9.93677862457103,0.,0.));
#30711=CARTESIAN_POINT('',(9.93677862457103,495.,0.978255169515729));
#30712=CARTESIAN_POINT('Origin',(2.,0.,0.));
#30713=CARTESIAN_POINT('',(2.,15.,0.));
#30714=CARTESIAN_POINT('',(8.5,15.,0.));
#30715=CARTESIAN_POINT('',(2.,495.,0.));
#30716=CARTESIAN_POINT('',(2.,0.,0.));
#30717=CARTESIAN_POINT('',(15.,495.,0.));
#30718=CARTESIAN_POINT('Origin',(2.,0.,2.));
#30719=CARTESIAN_POINT('',(2.22044604925031E-15,15.,2.));
#30720=CARTESIAN_POINT('Origin',(2.,15.,2.));
#30721=CARTESIAN_POINT('',(2.22044604925031E-15,495.,2.));
#30722=CARTESIAN_POINT('',(2.4980018054066E-15,0.,2.));
#30723=CARTESIAN_POINT('Origin',(2.,495.,2.));
#30724=CARTESIAN_POINT('Origin',(-2.22044604925031E-15,0.,9.93677862457103));
#30725=CARTESIAN_POINT('',(-2.22044604925031E-15,15.,9.93677862457103));
#30726=CARTESIAN_POINT('',(-2.22044604925031E-15,15.,8.71838931228551));
#30727=CARTESIAN_POINT('',(-2.22044604925031E-15,495.,9.93677862457103));
#30728=CARTESIAN_POINT('',(-2.22044604925031E-15,0.,9.93677862457103));
#30729=CARTESIAN_POINT('',(-2.22044604925031E-15,495.,9.93677862457103));
#30730=CARTESIAN_POINT('Origin',(0.978255169515727,0.,9.93677862457103));
#30731=CARTESIAN_POINT('',(0.978255169515727,15.,9.93677862457103));
#30732=CARTESIAN_POINT('',(7.98912758475786,15.,9.93677862457103));
#30733=CARTESIAN_POINT('',(0.978255169515727,495.,9.93677862457103));
#30734=CARTESIAN_POINT('',(0.978255169515727,0.,9.93677862457103));
#30735=CARTESIAN_POINT('',(0.978255169515727,495.,9.93677862457103));
#30736=CARTESIAN_POINT('Origin',(0.978255169515725,0.,10.7975927840689));
#30737=CARTESIAN_POINT('',(0.978255169515725,15.,10.7975927840689));
#30738=CARTESIAN_POINT('',(0.978255169515729,15.,9.14879639203444));
#30739=CARTESIAN_POINT('',(0.978255169515725,495.,10.7975927840689));
#30740=CARTESIAN_POINT('',(0.978255169515725,0.,10.7975927840689));
#30741=CARTESIAN_POINT('',(0.978255169515725,495.,10.7975927840689));
#30742=CARTESIAN_POINT('Origin',(1.95651033903146,0.,10.7975927840689));
#30743=CARTESIAN_POINT('',(1.95651033903146,15.,10.7975927840689));
#30744=CARTESIAN_POINT('',(8.47825516951573,15.,10.7975927840689));
#30745=CARTESIAN_POINT('',(1.95651033903146,495.,10.7975927840689));
#30746=CARTESIAN_POINT('',(1.95651033903146,0.,10.7975927840689));
#30747=CARTESIAN_POINT('',(1.95651033903146,495.,10.7975927840689));
#30748=CARTESIAN_POINT('Origin',(1.95651033903146,0.,6.95083166488121));
#30749=CARTESIAN_POINT('',(1.95651033903146,15.,6.95083166488121));
#30750=CARTESIAN_POINT('',(1.95651033903146,15.,7.2254158324406));
#30751=CARTESIAN_POINT('',(1.95651033903146,495.,6.95083166488121));
#30752=CARTESIAN_POINT('',(1.95651033903146,0.,6.95083166488121));
#30753=CARTESIAN_POINT('',(1.95651033903146,495.,6.95083166488121));
#30754=CARTESIAN_POINT('Origin',(5.62589609327486,0.,6.95083166488121));
#30755=CARTESIAN_POINT('',(5.62589609327486,15.,6.95083166488121));
#30756=CARTESIAN_POINT('',(10.3129480466374,15.,6.95083166488121));
#30757=CARTESIAN_POINT('',(5.62589609327486,495.,6.95083166488121));
#30758=CARTESIAN_POINT('',(5.62589609327486,0.,6.95083166488121));
#30759=CARTESIAN_POINT('',(1.95651033903146,495.,6.95083166488121));
#30760=CARTESIAN_POINT('Origin',(9.25,0.,10.6122749602376));
#30761=CARTESIAN_POINT('',(9.25,15.,10.6122749602376));
#30762=CARTESIAN_POINT('',(9.89473776739309,15.,11.2636555046265));
#30763=CARTESIAN_POINT('',(9.25,495.,10.6122749602376));
#30764=CARTESIAN_POINT('',(9.25,0.,10.6122749602376));
#30765=CARTESIAN_POINT('',(5.62589609327486,495.,6.95083166488121));
#30766=CARTESIAN_POINT('Origin',(15.,15.,22.5));
#30767=CARTESIAN_POINT('',(20.063221375429,15.,30.));
#30768=CARTESIAN_POINT('',(38.7183893122855,15.,30.));
#30769=CARTESIAN_POINT('',(20.063221375429,15.,29.0217448304843));
#30770=CARTESIAN_POINT('',(20.063221375429,15.,25.7608724152421));
#30771=CARTESIAN_POINT('',(19.2024072159311,15.,29.0217448304843));
#30772=CARTESIAN_POINT('',(17.1012036079655,15.,29.0217448304843));
#30773=CARTESIAN_POINT('',(19.2024072159311,15.,28.0434896609685));
#30774=CARTESIAN_POINT('',(19.2024072159311,15.,25.2717448304843));
#30775=CARTESIAN_POINT('',(23.0491683351188,15.,28.0434896609685));
#30776=CARTESIAN_POINT('',(19.0245841675594,15.,28.0434896609685));
#30777=CARTESIAN_POINT('',(23.0491683351188,15.,24.5536170636906));
#30778=CARTESIAN_POINT('',(23.0491683351188,15.,23.5268085318453));
#30779=CARTESIAN_POINT('',(19.284340547757,15.,20.75));
#30780=CARTESIAN_POINT('',(18.661711044137,15.,20.1209555023271));
#30781=CARTESIAN_POINT('',(10.715659452243,15.,20.75));
#30782=CARTESIAN_POINT('',(12.8578297261215,15.,20.75));
#30783=CARTESIAN_POINT('',(6.9508316648812,15.,24.5536170636906));
#30784=CARTESIAN_POINT('',(9.45587506218205,15.,22.0227640341724));
#30785=CARTESIAN_POINT('',(6.9508316648812,15.,28.0434896609685));
#30786=CARTESIAN_POINT('',(6.9508316648812,15.,25.2717448304843));
#30787=CARTESIAN_POINT('',(10.7975927840689,15.,28.0434896609685));
#30788=CARTESIAN_POINT('',(12.8987963920345,15.,28.0434896609685));
#30789=CARTESIAN_POINT('',(10.7975927840689,15.,29.0217448304843));
#30790=CARTESIAN_POINT('',(10.7975927840689,15.,25.7608724152421));
#30791=CARTESIAN_POINT('',(9.93677862457103,15.,29.0217448304843));
#30792=CARTESIAN_POINT('',(12.4683893122855,15.,29.0217448304843));
#30793=CARTESIAN_POINT('',(9.93677862457103,15.,30.));
#30794=CARTESIAN_POINT('',(9.93677862457103,15.,26.25));
#30795=CARTESIAN_POINT('',(2.,15.,30.));
#30796=CARTESIAN_POINT('',(8.5,15.,30.));
#30797=CARTESIAN_POINT('',(2.22044604925031E-15,15.,28.));
#30798=CARTESIAN_POINT('Origin',(2.,15.,28.));
#30799=CARTESIAN_POINT('',(-2.22044604925031E-15,15.,20.063221375429));
#30800=CARTESIAN_POINT('',(-2.22044604925031E-15,15.,21.2816106877145));
#30801=CARTESIAN_POINT('',(0.978255169515727,15.,20.063221375429));
#30802=CARTESIAN_POINT('',(7.98912758475786,15.,20.063221375429));
#30803=CARTESIAN_POINT('',(0.978255169515725,15.,19.2024072159311));
#30804=CARTESIAN_POINT('',(0.978255169515729,15.,20.8512036079656));
#30805=CARTESIAN_POINT('',(1.95651033903146,15.,19.2024072159311));
#30806=CARTESIAN_POINT('',(8.47825516951573,15.,19.2024072159311));
#30807=CARTESIAN_POINT('',(1.95651033903146,15.,23.0491683351188));
#30808=CARTESIAN_POINT('',(1.95651033903146,15.,22.7745841675594));
#30809=CARTESIAN_POINT('',(5.62589609327486,15.,23.0491683351188));
#30810=CARTESIAN_POINT('',(10.3129480466374,15.,23.0491683351188));
#30811=CARTESIAN_POINT('',(9.25,15.,19.3877250397624));
#30812=CARTESIAN_POINT('',(9.89473776739309,15.,18.7363444953735));
#30813=CARTESIAN_POINT('',(9.25,15.,18.75));
#30814=CARTESIAN_POINT('',(20.75,15.,19.3877250397624));
#30815=CARTESIAN_POINT('',(20.75,15.,9.05613748011882));
#30816=CARTESIAN_POINT('',(24.3741039067251,15.,23.0491683351188));
#30817=CARTESIAN_POINT('',(21.9173141859695,15.,20.5670661430517));
#30818=CARTESIAN_POINT('',(25.0491683351188,15.,23.0491683351188));
#30819=CARTESIAN_POINT('',(20.0245841675594,15.,23.0491683351188));
#30820=CARTESIAN_POINT('',(25.0491683351188,15.,28.0434896609685));
#30821=CARTESIAN_POINT('',(25.0491683351188,15.,25.2717448304843));
#30822=CARTESIAN_POINT('',(22.5,15.,28.0434896609685));
#30823=CARTESIAN_POINT('',(5.28668371362235,15.,28.1876354028611));
#30824=CARTESIAN_POINT('',(4.78668371362235,15.,28.6876354028611));
#30825=CARTESIAN_POINT('Origin',(4.78668371362235,15.,28.1876354028611));
#30826=CARTESIAN_POINT('',(5.28668371362236,15.,25.3185447775707));
#30827=CARTESIAN_POINT('',(5.28668371362236,15.,23.9092723887853));
#30828=CARTESIAN_POINT('',(4.78668371362235,15.,24.8185447775707));
#30829=CARTESIAN_POINT('Origin',(4.78668371362236,15.,25.3185447775707));
#30830=CARTESIAN_POINT('',(1.89960608334138,15.,24.8185447775707));
#30831=CARTESIAN_POINT('',(8.44980304167069,15.,24.8185447775707));
#30832=CARTESIAN_POINT('',(1.39960608334138,15.,25.3185447775707));
#30833=CARTESIAN_POINT('Origin',(1.89960608334138,15.,25.3185447775707));
#30834=CARTESIAN_POINT('',(1.39960608334138,15.,28.1876354028611));
#30835=CARTESIAN_POINT('',(1.39960608334138,15.,25.3438177014306));
#30836=CARTESIAN_POINT('',(1.89960608334138,15.,28.6876354028611));
#30837=CARTESIAN_POINT('Origin',(1.89960608334138,15.,28.1876354028611));
#30838=CARTESIAN_POINT('',(9.89334185681118,15.,28.6876354028611));
#30839=CARTESIAN_POINT('',(11.75,15.,15.));
#30840=CARTESIAN_POINT('Origin',(15.,15.,15.));
#30841=CARTESIAN_POINT('Origin',(1.89960608334138,0.,24.8185447775707));
#30842=CARTESIAN_POINT('',(4.78668371362235,495.,24.8185447775707));
#30843=CARTESIAN_POINT('',(4.78668371362235,0.,24.8185447775707));
#30844=CARTESIAN_POINT('',(1.89960608334138,495.,24.8185447775707));
#30845=CARTESIAN_POINT('',(1.89960608334138,495.,24.8185447775707));
#30846=CARTESIAN_POINT('',(1.89960608334138,0.,24.8185447775707));
#30847=CARTESIAN_POINT('Origin',(4.78668371362236,0.,25.3185447775707));
#30848=CARTESIAN_POINT('',(5.28668371362236,495.,25.3185447775707));
#30849=CARTESIAN_POINT('',(5.28668371362236,0.,25.3185447775707));
#30850=CARTESIAN_POINT('Origin',(4.78668371362236,495.,25.3185447775707));
#30851=CARTESIAN_POINT('Origin',(5.28668371362236,0.,25.3185447775707));
#30852=CARTESIAN_POINT('',(5.28668371362235,495.,28.1876354028611));
#30853=CARTESIAN_POINT('',(5.28668371362235,0.,28.1876354028611));
#30854=CARTESIAN_POINT('',(5.28668371362236,495.,25.3185447775707));
#30855=CARTESIAN_POINT('Origin',(4.78668371362235,0.,28.1876354028611));
#30856=CARTESIAN_POINT('',(4.78668371362235,495.,28.6876354028611));
#30857=CARTESIAN_POINT('',(4.78668371362235,0.,28.6876354028611));
#30858=CARTESIAN_POINT('Origin',(4.78668371362235,495.,28.1876354028611));
#30859=CARTESIAN_POINT('Origin',(19.284340547757,0.,20.75));
#30860=CARTESIAN_POINT('',(23.0491683351188,495.,24.5536170636906));
#30861=CARTESIAN_POINT('',(23.0491683351188,0.,24.5536170636906));
#30862=CARTESIAN_POINT('',(19.284340547757,495.,20.75));
#30863=CARTESIAN_POINT('',(23.0491683351188,495.,24.5536170636906));
#30864=CARTESIAN_POINT('',(19.284340547757,0.,20.75));
#30865=CARTESIAN_POINT('Origin',(23.0491683351188,0.,24.5536170636906));
#30866=CARTESIAN_POINT('',(23.0491683351188,495.,28.0434896609685));
#30867=CARTESIAN_POINT('',(23.0491683351188,0.,28.0434896609685));
#30868=CARTESIAN_POINT('',(23.0491683351188,495.,23.0491683351188));
#30869=CARTESIAN_POINT('Origin',(23.0491683351188,0.,28.0434896609685));
#30870=CARTESIAN_POINT('',(19.2024072159311,495.,28.0434896609685));
#30871=CARTESIAN_POINT('',(19.2024072159311,0.,28.0434896609685));
#30872=CARTESIAN_POINT('',(23.0491683351188,495.,28.0434896609685));
#30873=CARTESIAN_POINT('Origin',(19.2024072159311,0.,28.0434896609685));
#30874=CARTESIAN_POINT('',(19.2024072159311,495.,29.0217448304843));
#30875=CARTESIAN_POINT('',(19.2024072159311,0.,29.0217448304843));
#30876=CARTESIAN_POINT('',(19.2024072159311,495.,28.0434896609685));
#30877=CARTESIAN_POINT('Origin',(19.2024072159311,0.,29.0217448304843));
#30878=CARTESIAN_POINT('',(20.063221375429,495.,29.0217448304843));
#30879=CARTESIAN_POINT('',(20.063221375429,0.,29.0217448304843));
#30880=CARTESIAN_POINT('',(19.2024072159311,495.,29.0217448304843));
#30881=CARTESIAN_POINT('Origin',(20.063221375429,0.,29.0217448304843));
#30882=CARTESIAN_POINT('',(20.063221375429,495.,30.));
#30883=CARTESIAN_POINT('',(20.063221375429,0.,30.));
#30884=CARTESIAN_POINT('',(20.063221375429,495.,29.0217448304843));
#30885=CARTESIAN_POINT('Origin',(20.063221375429,0.,30.));
#30886=CARTESIAN_POINT('',(15.,495.,30.));
#30887=CARTESIAN_POINT('Origin',(30.,0.,28.0434896609685));
#30888=CARTESIAN_POINT('',(25.0491683351188,495.,28.0434896609685));
#30889=CARTESIAN_POINT('',(25.0491683351188,0.,28.0434896609685));
#30890=CARTESIAN_POINT('',(36.9508316648812,495.,28.0434896609685));
#30891=CARTESIAN_POINT('Origin',(25.0491683351188,0.,28.0434896609685));
#30892=CARTESIAN_POINT('',(25.0491683351188,495.,23.0491683351188));
#30893=CARTESIAN_POINT('',(25.0491683351188,0.,23.0491683351188));
#30894=CARTESIAN_POINT('',(25.0491683351188,495.,23.0491683351188));
#30895=CARTESIAN_POINT('Origin',(25.0491683351188,0.,23.0491683351188));
#30896=CARTESIAN_POINT('',(24.3741039067251,495.,23.0491683351188));
#30897=CARTESIAN_POINT('',(24.3741039067251,0.,23.0491683351188));
#30898=CARTESIAN_POINT('',(23.0491683351188,495.,23.0491683351188));
#30899=CARTESIAN_POINT('Origin',(24.3741039067251,0.,23.0491683351188));
#30900=CARTESIAN_POINT('',(20.75,495.,19.3877250397624));
#30901=CARTESIAN_POINT('',(20.75,0.,19.3877250397624));
#30902=CARTESIAN_POINT('',(24.3741039067251,495.,23.0491683351188));
#30903=CARTESIAN_POINT('Origin',(20.75,0.,19.3877250397624));
#30904=CARTESIAN_POINT('',(20.75,495.,20.75));
#30905=CARTESIAN_POINT('Origin',(15.,0.,15.));
#30906=CARTESIAN_POINT('',(11.75,495.,15.));
#30907=CARTESIAN_POINT('Origin',(15.,495.,15.));
#30908=CARTESIAN_POINT('',(11.75,0.,15.));
#30909=CARTESIAN_POINT('Origin',(9.25,0.,15.));
#30910=CARTESIAN_POINT('',(9.25,495.,19.3877250397624));
#30911=CARTESIAN_POINT('',(9.25,0.,19.3877250397624));
#30912=CARTESIAN_POINT('',(9.25,495.,20.75));
#30913=CARTESIAN_POINT('Origin',(1.89960608334138,0.,25.3185447775707));
#30914=CARTESIAN_POINT('',(1.39960608334138,495.,25.3185447775707));
#30915=CARTESIAN_POINT('Origin',(1.89960608334138,495.,25.3185447775707));
#30916=CARTESIAN_POINT('',(1.39960608334138,0.,25.3185447775707));
#30917=CARTESIAN_POINT('Origin',(1.39960608334138,0.,28.1876354028611));
#30918=CARTESIAN_POINT('',(1.39960608334138,495.,28.1876354028611));
#30919=CARTESIAN_POINT('',(1.39960608334138,495.,28.1876354028611));
#30920=CARTESIAN_POINT('',(1.39960608334138,0.,28.1876354028611));
#30921=CARTESIAN_POINT('Origin',(1.89960608334138,0.,28.1876354028611));
#30922=CARTESIAN_POINT('',(1.89960608334138,495.,28.6876354028611));
#30923=CARTESIAN_POINT('Origin',(1.89960608334138,495.,28.1876354028611));
#30924=CARTESIAN_POINT('',(1.89960608334138,0.,28.6876354028611));
#30925=CARTESIAN_POINT('Origin',(4.78668371362235,0.,28.6876354028611));
#30926=CARTESIAN_POINT('',(4.78668371362235,495.,28.6876354028611));
#30927=CARTESIAN_POINT('Origin',(10.715659452243,0.,20.75));
#30928=CARTESIAN_POINT('',(10.715659452243,495.,20.75));
#30929=CARTESIAN_POINT('',(9.25,495.,20.75));
#30930=CARTESIAN_POINT('',(10.715659452243,0.,20.75));
#30931=CARTESIAN_POINT('Origin',(6.9508316648812,0.,24.5536170636906));
#30932=CARTESIAN_POINT('',(6.9508316648812,495.,24.5536170636906));
#30933=CARTESIAN_POINT('',(6.9508316648812,495.,24.5536170636906));
#30934=CARTESIAN_POINT('',(6.9508316648812,0.,24.5536170636906));
#30935=CARTESIAN_POINT('Origin',(6.9508316648812,0.,28.0434896609685));
#30936=CARTESIAN_POINT('',(6.9508316648812,495.,28.0434896609685));
#30937=CARTESIAN_POINT('',(6.9508316648812,495.,23.0491683351188));
#30938=CARTESIAN_POINT('',(6.9508316648812,0.,28.0434896609685));
#30939=CARTESIAN_POINT('Origin',(10.7975927840689,0.,28.0434896609685));
#30940=CARTESIAN_POINT('',(10.7975927840689,495.,28.0434896609685));
#30941=CARTESIAN_POINT('',(9.93677862457103,495.,28.0434896609685));
#30942=CARTESIAN_POINT('',(10.7975927840689,0.,28.0434896609685));
#30943=CARTESIAN_POINT('Origin',(10.7975927840689,0.,29.0217448304843));
#30944=CARTESIAN_POINT('',(10.7975927840689,495.,29.0217448304843));
#30945=CARTESIAN_POINT('',(10.7975927840689,495.,28.0434896609685));
#30946=CARTESIAN_POINT('',(10.7975927840689,0.,29.0217448304843));
#30947=CARTESIAN_POINT('Origin',(9.93677862457103,0.,29.0217448304843));
#30948=CARTESIAN_POINT('',(9.93677862457103,495.,29.0217448304843));
#30949=CARTESIAN_POINT('',(10.7975927840689,495.,29.0217448304843));
#30950=CARTESIAN_POINT('',(9.93677862457103,0.,29.0217448304843));
#30951=CARTESIAN_POINT('Origin',(9.93677862457103,0.,30.));
#30952=CARTESIAN_POINT('',(9.93677862457103,495.,30.));
#30953=CARTESIAN_POINT('',(9.93677862457103,495.,29.0217448304843));
#30954=CARTESIAN_POINT('',(9.93677862457103,0.,30.));
#30955=CARTESIAN_POINT('Origin',(2.,0.,30.));
#30956=CARTESIAN_POINT('',(2.,495.,30.));
#30957=CARTESIAN_POINT('',(15.,495.,30.));
#30958=CARTESIAN_POINT('',(2.,0.,30.));
#30959=CARTESIAN_POINT('Origin',(2.,0.,28.));
#30960=CARTESIAN_POINT('',(2.22044604925031E-15,495.,28.));
#30961=CARTESIAN_POINT('Origin',(2.,495.,28.));
#30962=CARTESIAN_POINT('',(2.4980018054066E-15,0.,28.));
#30963=CARTESIAN_POINT('Origin',(-2.22044604925031E-15,0.,20.063221375429));
#30964=CARTESIAN_POINT('',(-2.22044604925031E-15,495.,20.063221375429));
#30965=CARTESIAN_POINT('',(-2.22044604925031E-15,495.,20.063221375429));
#30966=CARTESIAN_POINT('',(-2.22044604925031E-15,0.,20.063221375429));
#30967=CARTESIAN_POINT('Origin',(0.978255169515727,0.,20.063221375429));
#30968=CARTESIAN_POINT('',(0.978255169515727,495.,20.063221375429));
#30969=CARTESIAN_POINT('',(0.978255169515727,495.,20.063221375429));
#30970=CARTESIAN_POINT('',(0.978255169515727,0.,20.063221375429));
#30971=CARTESIAN_POINT('Origin',(0.978255169515725,0.,19.2024072159311));
#30972=CARTESIAN_POINT('',(0.978255169515725,495.,19.2024072159311));
#30973=CARTESIAN_POINT('',(0.978255169515725,495.,19.2024072159311));
#30974=CARTESIAN_POINT('',(0.978255169515725,0.,19.2024072159311));
#30975=CARTESIAN_POINT('Origin',(1.95651033903146,0.,19.2024072159311));
#30976=CARTESIAN_POINT('',(1.95651033903146,495.,19.2024072159311));
#30977=CARTESIAN_POINT('',(1.95651033903146,495.,19.2024072159311));
#30978=CARTESIAN_POINT('',(1.95651033903146,0.,19.2024072159311));
#30979=CARTESIAN_POINT('Origin',(1.95651033903146,0.,23.0491683351188));
#30980=CARTESIAN_POINT('',(1.95651033903146,495.,23.0491683351188));
#30981=CARTESIAN_POINT('',(1.95651033903146,495.,23.0491683351188));
#30982=CARTESIAN_POINT('',(1.95651033903146,0.,23.0491683351188));
#30983=CARTESIAN_POINT('Origin',(5.62589609327486,0.,23.0491683351188));
#30984=CARTESIAN_POINT('',(5.62589609327486,495.,23.0491683351188));
#30985=CARTESIAN_POINT('',(1.95651033903146,495.,23.0491683351188));
#30986=CARTESIAN_POINT('',(5.62589609327486,0.,23.0491683351188));
#30987=CARTESIAN_POINT('Origin',(9.25,0.,19.3877250397624));
#30988=CARTESIAN_POINT('',(5.62589609327486,495.,23.0491683351188));
#30989=CARTESIAN_POINT('Origin',(15.,495.,22.5));
#30990=CARTESIAN_POINT('',(0.,0.,0.));
#30991=CARTESIAN_POINT('Origin',(74.9879498948689,255.,53.0228109606356));
#30992=CARTESIAN_POINT('',(82.9065970110875,414.278332223638,53.0282292646567));
#30993=CARTESIAN_POINT('',(82.9129498948689,415.721667776361,53.0228109606487));
#30994=CARTESIAN_POINT('',(82.9129498948689,255.,53.0228109606356));
#30995=CARTESIAN_POINT('',(67.8083803398704,416.,49.6673071229179));
#30996=CARTESIAN_POINT('Ctrl Pts',(82.9129498948689,414.278332223638,53.0228109606355));
#30997=CARTESIAN_POINT('Ctrl Pts',(82.9129498948689,414.455428795637,50.8182135007257));
#30998=CARTESIAN_POINT('Ctrl Pts',(81.9432795991106,414.632525367635,48.6308565362894));
#30999=CARTESIAN_POINT('Ctrl Pts',(80.3096882702542,414.809621939634,47.1504412801785));
#31000=CARTESIAN_POINT('Ctrl Pts',(78.6760969413978,414.986718511633,45.6700260240676));
#31001=CARTESIAN_POINT('Ctrl Pts',(76.4041347530445,415.163815083631,44.9197069006031));
#31002=CARTESIAN_POINT('Ctrl Pts',(74.210180011222,415.34091165563,45.136068983869));
#31003=CARTESIAN_POINT('Ctrl Pts',(72.0162252693994,415.518008227629,45.3524310671349));
#31004=CARTESIAN_POINT('Ctrl Pts',(69.934592507698,415.695104799628,46.5320903475013));
#31005=CARTESIAN_POINT('Ctrl Pts',(68.6216467656608,415.872201371626,48.3030853894784));
#31006=CARTESIAN_POINT('Ctrl Pts',(68.3058253599202,415.914800914418,48.7290878706236));
#31007=CARTESIAN_POINT('Ctrl Pts',(68.0329145681891,415.957400457209,49.1868847518951));
#31008=CARTESIAN_POINT('Ctrl Pts',(67.8083803398704,416.,49.6673071229179));
#31009=CARTESIAN_POINT('',(82.1675194498639,416.,49.6673071229103));
#31010=CARTESIAN_POINT('Origin',(74.9879498948689,416.,53.0228109606356));
#31011=CARTESIAN_POINT('Ctrl Pts',(82.1675194498639,416.000000000001,49.6673071229103));
#31012=CARTESIAN_POINT('Ctrl Pts',(82.6565318269656,415.907222592121,50.7136174668838));
#31013=CARTESIAN_POINT('Ctrl Pts',(82.9065122305317,415.814445184241,51.86425892299));
#31014=CARTESIAN_POINT('Ctrl Pts',(82.9078731907355,415.721667776361,53.0191031778888));
#31015=CARTESIAN_POINT('Origin',(74.9879498948689,255.,53.0228109606356));
#31016=CARTESIAN_POINT('',(82.9241352897681,410.278332223638,53.0251703538597));
#31017=CARTESIAN_POINT('',(82.9129145441845,411.721667776361,53.0231512301084));
#31018=CARTESIAN_POINT('',(82.9129498948689,255.,53.0228109606356));
#31019=CARTESIAN_POINT('Ctrl Pts',(82.9241352897681,410.278332223638,53.0251703538597));
#31020=CARTESIAN_POINT('Ctrl Pts',(82.9144087418507,410.479926090632,50.5264531396333));
#31021=CARTESIAN_POINT('Ctrl Pts',(81.6392328200664,410.681519957625,48.0190747435334));
#31022=CARTESIAN_POINT('Ctrl Pts',(79.6067374458105,410.883113824619,46.5659622102762));
#31023=CARTESIAN_POINT('Ctrl Pts',(77.4677531876784,411.095269834171,45.0367164991663));
#31024=CARTESIAN_POINT('Ctrl Pts',(74.4900138615837,411.307425843724,44.6751033274731));
#31025=CARTESIAN_POINT('Ctrl Pts',(72.0493789123074,411.519581853276,45.6477657875292));
#31026=CARTESIAN_POINT('Ctrl Pts',(69.6087439630311,411.731737862829,46.6204282475853));
#31027=CARTESIAN_POINT('Ctrl Pts',(67.7052133905732,411.94389387238,48.9273663393907));
#31028=CARTESIAN_POINT('Ctrl Pts',(67.1985039826836,412.156049881933,51.5089701657794));
#31029=CARTESIAN_POINT('Ctrl Pts',(66.9451492787388,412.262127886709,52.7997720789737));
#31030=CARTESIAN_POINT('Ctrl Pts',(67.040999865936,412.368205891486,54.1592404258139));
#31031=CARTESIAN_POINT('Ctrl Pts',(67.4422155137494,412.474283896262,55.4216291114888));
#31032=CARTESIAN_POINT('Ctrl Pts',(67.8434311615628,412.580361901038,56.6840177971637));
#31033=CARTESIAN_POINT('Ctrl Pts',(68.5500118699923,412.686439905814,57.8493268216733));
#31034=CARTESIAN_POINT('Ctrl Pts',(69.5022941704941,412.79251791059,58.7568510247251));
#31035=CARTESIAN_POINT('Ctrl Pts',(71.4068587714976,413.004673920142,60.5718994308287));
#31036=CARTESIAN_POINT('Ctrl Pts',(74.29422974079,413.216829929695,61.3558085511009));
#31037=CARTESIAN_POINT('Ctrl Pts',(76.8480876043277,413.428985939247,60.7407007216353));
#31038=CARTESIAN_POINT('Ctrl Pts',(79.4019454678654,413.6411419488,60.1255928921697));
#31039=CARTESIAN_POINT('Ctrl Pts',(81.6222902256485,413.853297958352,58.1114681129663));
#31040=CARTESIAN_POINT('Ctrl Pts',(82.4863699092025,414.065453967904,55.6275433329795));
#31041=CARTESIAN_POINT('Ctrl Pts',(82.7753770039315,414.136413386482,54.7967497177));
#31042=CARTESIAN_POINT('Ctrl Pts',(82.9126601982892,414.20737280506,53.913400086736));
#31043=CARTESIAN_POINT('Ctrl Pts',(82.9065970110875,414.278332223638,53.0282292646567));
#31044=CARTESIAN_POINT('Ctrl Pts',(82.9129498948689,415.721667776361,53.0228109606488));
#31045=CARTESIAN_POINT('Ctrl Pts',(82.9129498948652,415.544571204362,55.2274084205585));
#31046=CARTESIAN_POINT('Ctrl Pts',(81.9432795991034,415.367474632363,57.4147653849931));
#31047=CARTESIAN_POINT('Ctrl Pts',(80.3096882702446,415.190378060364,58.8951806411014));
#31048=CARTESIAN_POINT('Ctrl Pts',(78.6760969413858,415.013281488366,60.3755958972096));
#31049=CARTESIAN_POINT('Ctrl Pts',(76.4041347530313,414.836184916367,61.1259150206704));
#31050=CARTESIAN_POINT('Ctrl Pts',(74.2101800112091,414.659088344368,60.9095529374009));
#31051=CARTESIAN_POINT('Ctrl Pts',(72.016225269387,414.481991772369,60.6931908541314));
#31052=CARTESIAN_POINT('Ctrl Pts',(69.9345925076874,414.304895200371,59.5135315737616));
#31053=CARTESIAN_POINT('Ctrl Pts',(68.6216467656532,414.127798628372,57.7425365317824));
#31054=CARTESIAN_POINT('Ctrl Pts',(67.3087010236189,413.950702056373,55.9715414898033));
#31055=CARTESIAN_POINT('Ctrl Pts',(66.784977419823,413.773605484375,53.6369099216174));
#31056=CARTESIAN_POINT('Ctrl Pts',(67.215612605763,413.596508912376,51.4747805783839));
#31057=CARTESIAN_POINT('Ctrl Pts',(67.6462477917031,413.419412340377,49.3126512351505));
#31058=CARTESIAN_POINT('Ctrl Pts',(69.0245064208055,413.242315768378,47.3568408855388));
#31059=CARTESIAN_POINT('Ctrl Pts',(70.9158061804571,413.06521919638,46.224041177125));
#31060=CARTESIAN_POINT('Ctrl Pts',(72.8071059401087,412.888122624381,45.0912414687111));
#31061=CARTESIAN_POINT('Ctrl Pts',(75.1818659698228,412.711026052382,44.7991699473061));
#31062=CARTESIAN_POINT('Ctrl Pts',(77.2912945088783,412.533929480384,45.4399204438792));
#31063=CARTESIAN_POINT('Ctrl Pts',(79.4007230479338,412.356832908385,46.0806709404523));
#31064=CARTESIAN_POINT('Ctrl Pts',(81.2118275942158,412.179736336386,47.6442218014031));
#31065=CARTESIAN_POINT('Ctrl Pts',(82.1535440633151,412.002639764387,49.6375657386272));
#31066=CARTESIAN_POINT('Ctrl Pts',(82.6515697929947,411.908982435045,50.6917435101895));
#31067=CARTESIAN_POINT('Ctrl Pts',(82.9129498948708,411.815325105703,51.8569119935511));
#31068=CARTESIAN_POINT('Ctrl Pts',(82.9129498948689,411.721667776361,53.0228109606486));
#31069=CARTESIAN_POINT('Origin',(74.9879498948689,255.,53.0228109606356));
#31070=CARTESIAN_POINT('',(82.9129987951795,406.278332223638,53.022353166431));
#31071=CARTESIAN_POINT('',(82.9231891863576,407.721667776361,53.0235399778202));
#31072=CARTESIAN_POINT('',(82.9129498948689,255.,53.0228109606356));
#31073=CARTESIAN_POINT('Ctrl Pts',(82.9136411619662,406.278332223638,53.0163394665249));
#31074=CARTESIAN_POINT('Ctrl Pts',(82.9194890840726,406.328167357099,52.3962321856271));
#31075=CARTESIAN_POINT('Ctrl Pts',(82.8528804541948,406.37800249056,51.7772617381742));
#31076=CARTESIAN_POINT('Ctrl Pts',(82.7090801244942,406.427837624021,51.1765844418892));
#31077=CARTESIAN_POINT('Ctrl Pts',(82.0968994799793,406.639993633573,48.6194066165628));
#31078=CARTESIAN_POINT('Ctrl Pts',(80.0857435909802,406.852149643125,46.3937626956099));
#31079=CARTESIAN_POINT('Ctrl Pts',(77.605322558894,407.064305652678,45.5277522795078));
#31080=CARTESIAN_POINT('Ctrl Pts',(75.1249015268078,407.27646166223,44.6617418634056));
#31081=CARTESIAN_POINT('Ctrl Pts',(72.1752153516344,407.488617671782,45.1553649521542));
#31082=CARTESIAN_POINT('Ctrl Pts',(70.0996427799517,407.700773681334,46.7721254255252));
#31083=CARTESIAN_POINT('Ctrl Pts',(69.0618564941103,407.806851686111,47.5805056622108));
#31084=CARTESIAN_POINT('Ctrl Pts',(68.2425986091416,407.912929690887,48.6696702450519));
#31085=CARTESIAN_POINT('Ctrl Pts',(67.7178205322322,408.019007695663,49.8858983521605));
#31086=CARTESIAN_POINT('Ctrl Pts',(67.1930424553228,408.125085700439,51.102126459269));
#31087=CARTESIAN_POINT('Ctrl Pts',(66.9627441864726,408.231163705215,52.4454180906449));
#31088=CARTESIAN_POINT('Ctrl Pts',(67.0866534420349,408.337241709991,53.7550467932846));
#31089=CARTESIAN_POINT('Ctrl Pts',(67.3344719531597,408.549397719544,56.3743041985641));
#31090=CARTESIAN_POINT('Ctrl Pts',(68.9991205619347,408.761553729096,58.8589098888989));
#31091=CARTESIAN_POINT('Ctrl Pts',(71.3309510746786,408.973709738649,60.0692889110528));
#31092=CARTESIAN_POINT('Ctrl Pts',(73.6627815874224,409.185865748201,61.2796679332067));
#31093=CARTESIAN_POINT('Ctrl Pts',(76.6617940041351,409.398021757753,61.2158202871798));
#31094=CARTESIAN_POINT('Ctrl Pts',(78.9421958230637,409.610177767305,59.906728427714));
#31095=CARTESIAN_POINT('Ctrl Pts',(81.2225976419923,409.822333776857,58.5976365682483));
#31096=CARTESIAN_POINT('Ctrl Pts',(82.7843888631369,410.03448978641,56.0433004953437));
#31097=CARTESIAN_POINT('Ctrl Pts',(82.9151698786245,410.246645795963,53.4176933336282));
#31098=CARTESIAN_POINT('Ctrl Pts',(82.9216807841248,410.257207938521,53.2869780302849));
#31099=CARTESIAN_POINT('Ctrl Pts',(82.9246448944859,410.26777008108,53.156086079738));
#31100=CARTESIAN_POINT('Ctrl Pts',(82.9241352897681,410.278332223638,53.0251703538597));
#31101=CARTESIAN_POINT('Ctrl Pts',(82.9124186818494,411.721667776361,53.0279241726423));
#31102=CARTESIAN_POINT('Ctrl Pts',(82.9169360649469,411.662686450708,53.7626941830692));
#31103=CARTESIAN_POINT('Ctrl Pts',(82.8207774927491,411.603705125055,54.4960880068349));
#31104=CARTESIAN_POINT('Ctrl Pts',(82.6188780515908,411.544723799402,55.1990731318781));
#31105=CARTESIAN_POINT('Ctrl Pts',(81.8926451415501,411.33256778985,57.7277127860879));
#31106=CARTESIAN_POINT('Ctrl Pts',(79.7982912841655,411.120411780297,59.8629115870814));
#31107=CARTESIAN_POINT('Ctrl Pts',(77.2832349439534,410.908255770745,60.622689727324));
#31108=CARTESIAN_POINT('Ctrl Pts',(74.7681786037414,410.696099761193,61.3824678675665));
#31109=CARTESIAN_POINT('Ctrl Pts',(71.8324197807018,410.48394375164,60.7668253470583));
#31110=CARTESIAN_POINT('Ctrl Pts',(69.8324586031125,410.271787742088,59.0597807109634));
#31111=CARTESIAN_POINT('Ctrl Pts',(67.8324974255232,410.059631732536,57.3527360748685));
#31112=CARTESIAN_POINT('Ctrl Pts',(66.7683338933842,409.847475722983,54.554289323187));
#31113=CARTESIAN_POINT('Ctrl Pts',(67.1237968814133,409.635319713431,51.9495700089795));
#31114=CARTESIAN_POINT('Ctrl Pts',(67.4792598694425,409.423163703879,49.3448506947721));
#31115=CARTESIAN_POINT('Ctrl Pts',(69.2543493776398,409.211007694326,46.9338588180387));
#31116=CARTESIAN_POINT('Ctrl Pts',(71.638613990893,408.998851684774,45.8251495656732));
#31117=CARTESIAN_POINT('Ctrl Pts',(74.0228786041463,408.786695675222,44.7164403133077));
#31118=CARTESIAN_POINT('Ctrl Pts',(77.0163183224555,408.574539665669,44.9100136853101));
#31119=CARTESIAN_POINT('Ctrl Pts',(79.2357603254525,408.362383656117,46.3159041905652));
#31120=CARTESIAN_POINT('Ctrl Pts',(81.4552023284494,408.150227646565,47.7217946958203));
#31121=CARTESIAN_POINT('Ctrl Pts',(82.9006466161341,407.938071637013,50.3400023343282));
#31122=CARTESIAN_POINT('Ctrl Pts',(82.9229329658515,407.72591562746,52.970862780681));
#31123=CARTESIAN_POINT('Ctrl Pts',(82.9230817071722,407.724499677094,52.9884214056813));
#31124=CARTESIAN_POINT('Ctrl Pts',(82.9231670559047,407.723083726727,53.0059805942834));
#31125=CARTESIAN_POINT('Ctrl Pts',(82.9231891863576,407.721667776361,53.0235399778202));
#31126=CARTESIAN_POINT('Origin',(74.9879498948689,255.,53.0228109606356));
#31127=CARTESIAN_POINT('',(82.9129498948689,402.278332223638,53.0228109606356));
#31128=CARTESIAN_POINT('',(82.9110727027003,403.721667776361,53.0200287533551));
#31129=CARTESIAN_POINT('',(82.9129498948689,255.,53.0228109606356));
#31130=CARTESIAN_POINT('Ctrl Pts',(82.9129498948689,402.278332223638,53.0228109606358));
#31131=CARTESIAN_POINT('Ctrl Pts',(82.912949894869,402.455428795637,50.8182135007261));
#31132=CARTESIAN_POINT('Ctrl Pts',(81.9432795991109,402.632525367635,48.6308565362898));
#31133=CARTESIAN_POINT('Ctrl Pts',(80.3096882702546,402.809621939634,47.1504412801789));
#31134=CARTESIAN_POINT('Ctrl Pts',(78.6760969413983,402.986718511633,45.6700260240679));
#31135=CARTESIAN_POINT('Ctrl Pts',(76.4041347530452,403.163815083631,44.9197069006032));
#31136=CARTESIAN_POINT('Ctrl Pts',(74.2101800112226,403.34091165563,45.1360689838689));
#31137=CARTESIAN_POINT('Ctrl Pts',(72.0162252694001,403.518008227629,45.3524310671347));
#31138=CARTESIAN_POINT('Ctrl Pts',(69.9345925076986,403.695104799628,46.5320903475009));
#31139=CARTESIAN_POINT('Ctrl Pts',(68.6216467656613,403.872201371626,48.3030853894777));
#31140=CARTESIAN_POINT('Ctrl Pts',(67.308701023624,404.049297943625,50.0740804314546));
#31141=CARTESIAN_POINT('Ctrl Pts',(66.784977419824,404.226394515624,52.4087119996396));
#31142=CARTESIAN_POINT('Ctrl Pts',(67.2156126057604,404.403491087622,54.5708413428738));
#31143=CARTESIAN_POINT('Ctrl Pts',(67.6462477916967,404.580587659621,56.7329706861079));
#31144=CARTESIAN_POINT('Ctrl Pts',(69.0245064207957,404.75768423162,58.6887810357219));
#31145=CARTESIAN_POINT('Ctrl Pts',(70.9158061804453,404.934780803619,59.8215807441391));
#31146=CARTESIAN_POINT('Ctrl Pts',(72.8071059400949,405.111877375617,60.9543804525562));
#31147=CARTESIAN_POINT('Ctrl Pts',(75.1818659698084,405.288973947616,61.2464519739654));
#31148=CARTESIAN_POINT('Ctrl Pts',(77.2912945088651,405.466070519615,60.605701477396));
#31149=CARTESIAN_POINT('Ctrl Pts',(79.4007230479217,405.643167091614,59.9649509808265));
#31150=CARTESIAN_POINT('Ctrl Pts',(81.2118275942064,405.820263663612,58.4014001198789));
#31151=CARTESIAN_POINT('Ctrl Pts',(82.1535440633091,405.997360235611,56.4080561826565));
#31152=CARTESIAN_POINT('Ctrl Pts',(82.6515697929907,406.091017564953,55.3538784110949));
#31153=CARTESIAN_POINT('Ctrl Pts',(82.9129498948689,406.184674894295,54.1887099277337));
#31154=CARTESIAN_POINT('Ctrl Pts',(82.9129498948689,406.278332223638,53.022810960636));
#31155=CARTESIAN_POINT('Ctrl Pts',(82.9231891863576,407.721667776361,53.0235399778202));
#31156=CARTESIAN_POINT('Ctrl Pts',(82.9248249913466,407.617005721951,54.3214676443345));
#31157=CARTESIAN_POINT('Ctrl Pts',(82.5810585782997,407.512343667541,55.6204603650967));
#31158=CARTESIAN_POINT('Ctrl Pts',(81.9622851139255,407.407681613132,56.7716307635747));
#31159=CARTESIAN_POINT('Ctrl Pts',(81.3351403967737,407.301603608356,57.9383750981546));
#31160=CARTESIAN_POINT('Ctrl Pts',(80.4254972721032,407.19552560358,58.9532703421768));
#31161=CARTESIAN_POINT('Ctrl Pts',(79.3222099604759,407.089447598803,59.6696753185319));
#31162=CARTESIAN_POINT('Ctrl Pts',(77.1156353372214,406.877291589251,61.1024852712423));
#31163=CARTESIAN_POINT('Ctrl Pts',(74.1344839661398,406.665135579699,61.3413341532847));
#31164=CARTESIAN_POINT('Ctrl Pts',(71.7374668755085,406.452979570146,60.2658009811163));
#31165=CARTESIAN_POINT('Ctrl Pts',(69.3404497848772,406.240823560594,59.1902678089478));
#31166=CARTESIAN_POINT('Ctrl Pts',(67.5275669746961,406.028667551042,56.8003525825685));
#31167=CARTESIAN_POINT('Ctrl Pts',(67.1369370180655,405.81651154149,54.2000964780969));
#31168=CARTESIAN_POINT('Ctrl Pts',(66.7463070614349,405.604355531937,51.5998403736252));
#31169=CARTESIAN_POINT('Ctrl Pts',(67.7779299583547,405.392199522385,48.7892433910612));
#31170=CARTESIAN_POINT('Ctrl Pts',(69.7543007334193,405.180043512832,47.05577978859));
#31171=CARTESIAN_POINT('Ctrl Pts',(71.7306715084839,404.96788750328,45.3223161861188));
#31172=CARTESIAN_POINT('Ctrl Pts',(74.6517901616933,404.755731493728,44.6659859637404));
#31173=CARTESIAN_POINT('Ctrl Pts',(77.1789100392733,404.543575484176,45.3923390707145));
#31174=CARTESIAN_POINT('Ctrl Pts',(79.7060299168532,404.331419474623,46.1186921776886));
#31175=CARTESIAN_POINT('Ctrl Pts',(81.8391510188038,404.119263465071,48.2277286140151));
#31176=CARTESIAN_POINT('Ctrl Pts',(82.5929447446449,403.907107455519,50.7445233499528));
#31177=CARTESIAN_POINT('Ctrl Pts',(82.8125681355735,403.845294229133,51.4778101567128));
#31178=CARTESIAN_POINT('Ctrl Pts',(82.915101607755,403.783481002747,52.2457112160404));
#31179=CARTESIAN_POINT('Ctrl Pts',(82.9078799846978,403.721667776361,53.0152967906599));
#31180=CARTESIAN_POINT('Origin',(74.9879498948689,255.,53.0228109606356));
#31181=CARTESIAN_POINT('',(82.9129498948689,398.278332223638,53.0228109606356));
#31182=CARTESIAN_POINT('',(82.9080990005812,399.721667776361,53.0247995869528));
#31183=CARTESIAN_POINT('',(82.9129498948689,255.,53.0228109606356));
#31184=CARTESIAN_POINT('Ctrl Pts',(82.9129498948689,398.278332223638,53.0228109606356));
#31185=CARTESIAN_POINT('Ctrl Pts',(82.9129498948689,398.455428795637,50.8182135007258));
#31186=CARTESIAN_POINT('Ctrl Pts',(81.9432795991107,398.632525367635,48.6308565362895));
#31187=CARTESIAN_POINT('Ctrl Pts',(80.3096882702543,398.809621939634,47.1504412801786));
#31188=CARTESIAN_POINT('Ctrl Pts',(78.6760969413979,398.986718511633,45.6700260240676));
#31189=CARTESIAN_POINT('Ctrl Pts',(76.4041347530446,399.163815083631,44.9197069006031));
#31190=CARTESIAN_POINT('Ctrl Pts',(74.2101800112221,399.34091165563,45.136068983869));
#31191=CARTESIAN_POINT('Ctrl Pts',(72.0162252693995,399.518008227629,45.3524310671349));
#31192=CARTESIAN_POINT('Ctrl Pts',(69.934592507698,399.695104799628,46.5320903475013));
#31193=CARTESIAN_POINT('Ctrl Pts',(68.6216467656608,399.872201371626,48.3030853894784));
#31194=CARTESIAN_POINT('Ctrl Pts',(67.3087010236236,400.049297943625,50.0740804314554));
#31195=CARTESIAN_POINT('Ctrl Pts',(66.7849774198239,400.226394515624,52.4087119996406));
#31196=CARTESIAN_POINT('Ctrl Pts',(67.2156126057605,400.403491087623,54.5708413428747));
#31197=CARTESIAN_POINT('Ctrl Pts',(67.6462477916972,400.580587659621,56.7329706861089));
#31198=CARTESIAN_POINT('Ctrl Pts',(69.0245064207965,400.75768423162,58.6887810357228));
#31199=CARTESIAN_POINT('Ctrl Pts',(70.9158061804463,400.934780803619,59.8215807441397));
#31200=CARTESIAN_POINT('Ctrl Pts',(72.8071059400962,401.111877375617,60.9543804525566));
#31201=CARTESIAN_POINT('Ctrl Pts',(75.1818659698098,401.288973947616,61.2464519739654));
#31202=CARTESIAN_POINT('Ctrl Pts',(77.2912945088664,401.466070519615,60.6057014773956));
#31203=CARTESIAN_POINT('Ctrl Pts',(79.400723047923,401.643167091614,59.9649509808257));
#31204=CARTESIAN_POINT('Ctrl Pts',(81.2118275942074,401.820263663612,58.4014001198777));
#31205=CARTESIAN_POINT('Ctrl Pts',(82.1535440633098,401.997360235611,56.4080561826551));
#31206=CARTESIAN_POINT('Ctrl Pts',(82.651569792991,402.091017564953,55.3538784110938));
#31207=CARTESIAN_POINT('Ctrl Pts',(82.9129498948689,402.184674894296,54.188709927733));
#31208=CARTESIAN_POINT('Ctrl Pts',(82.9129498948689,402.278332223638,53.0228109606358));
#31209=CARTESIAN_POINT('Ctrl Pts',(82.9129498948689,403.721667776361,53.0228109606491));
#31210=CARTESIAN_POINT('Ctrl Pts',(82.9129498948652,403.544571204362,55.2274084205589));
#31211=CARTESIAN_POINT('Ctrl Pts',(81.9432795991032,403.367474632363,57.4147653849934));
#31212=CARTESIAN_POINT('Ctrl Pts',(80.3096882702443,403.190378060364,58.8951806411016));
#31213=CARTESIAN_POINT('Ctrl Pts',(78.6760969413854,403.013281488366,60.3755958972097));
#31214=CARTESIAN_POINT('Ctrl Pts',(76.4041347530309,402.836184916367,61.1259150206704));
#31215=CARTESIAN_POINT('Ctrl Pts',(74.2101800112088,402.659088344368,60.9095529374008));
#31216=CARTESIAN_POINT('Ctrl Pts',(72.0162252693866,402.481991772369,60.6931908541313));
#31217=CARTESIAN_POINT('Ctrl Pts',(69.9345925076871,402.304895200371,59.5135315737614));
#31218=CARTESIAN_POINT('Ctrl Pts',(68.6216467656529,402.127798628372,57.7425365317821));
#31219=CARTESIAN_POINT('Ctrl Pts',(67.3087010236187,401.950702056373,55.9715414898029));
#31220=CARTESIAN_POINT('Ctrl Pts',(66.7849774198229,401.773605484375,53.6369099216169));
#31221=CARTESIAN_POINT('Ctrl Pts',(67.2156126057631,401.596508912376,51.4747805783835));
#31222=CARTESIAN_POINT('Ctrl Pts',(67.6462477917033,401.419412340377,49.3126512351501));
#31223=CARTESIAN_POINT('Ctrl Pts',(69.0245064208058,401.242315768378,47.3568408855385));
#31224=CARTESIAN_POINT('Ctrl Pts',(70.9158061804575,401.06521919638,46.2240411771248));
#31225=CARTESIAN_POINT('Ctrl Pts',(72.8071059401091,400.888122624381,45.091241468711));
#31226=CARTESIAN_POINT('Ctrl Pts',(75.1818659698232,400.711026052382,44.7991699473061));
#31227=CARTESIAN_POINT('Ctrl Pts',(77.2912945088787,400.533929480384,45.4399204438793));
#31228=CARTESIAN_POINT('Ctrl Pts',(79.4007230479342,400.356832908385,46.0806709404525));
#31229=CARTESIAN_POINT('Ctrl Pts',(81.2118275942161,400.179736336386,47.6442218014035));
#31230=CARTESIAN_POINT('Ctrl Pts',(82.1535440633153,400.002639764387,49.6375657386276));
#31231=CARTESIAN_POINT('Ctrl Pts',(82.6515697929948,399.908982435045,50.6917435101899));
#31232=CARTESIAN_POINT('Ctrl Pts',(82.9129498948709,399.815325105703,51.8569119935514));
#31233=CARTESIAN_POINT('Ctrl Pts',(82.9129498948689,399.721667776361,53.0228109606489));
#31234=CARTESIAN_POINT('Origin',(74.9879498948689,255.,53.0228109606356));
#31235=CARTESIAN_POINT('',(82.9143243890985,394.278332223638,53.0219084888199));
#31236=CARTESIAN_POINT('',(82.9141514706698,395.72166777636,53.0235187303091));
#31237=CARTESIAN_POINT('',(82.9129498948689,255.,53.0228109606356));
#31238=CARTESIAN_POINT('Ctrl Pts',(82.9129498948689,394.278332223638,53.0228109606354));
#31239=CARTESIAN_POINT('Ctrl Pts',(82.9129498948689,394.455428795637,50.8182135007256));
#31240=CARTESIAN_POINT('Ctrl Pts',(81.9432795991106,394.632525367635,48.6308565362894));
#31241=CARTESIAN_POINT('Ctrl Pts',(80.3096882702542,394.809621939634,47.1504412801785));
#31242=CARTESIAN_POINT('Ctrl Pts',(78.6760969413978,394.986718511633,45.6700260240676));
#31243=CARTESIAN_POINT('Ctrl Pts',(76.4041347530445,395.163815083631,44.9197069006031));
#31244=CARTESIAN_POINT('Ctrl Pts',(74.210180011222,395.34091165563,45.136068983869));
#31245=CARTESIAN_POINT('Ctrl Pts',(72.0162252693995,395.518008227629,45.3524310671349));
#31246=CARTESIAN_POINT('Ctrl Pts',(69.934592507698,395.695104799628,46.5320903475013));
#31247=CARTESIAN_POINT('Ctrl Pts',(68.6216467656608,395.872201371626,48.3030853894784));
#31248=CARTESIAN_POINT('Ctrl Pts',(67.3087010236237,396.049297943625,50.0740804314554));
#31249=CARTESIAN_POINT('Ctrl Pts',(66.7849774198239,396.226394515624,52.4087119996405));
#31250=CARTESIAN_POINT('Ctrl Pts',(67.2156126057605,396.403491087623,54.5708413428747));
#31251=CARTESIAN_POINT('Ctrl Pts',(67.6462477916971,396.580587659621,56.7329706861088));
#31252=CARTESIAN_POINT('Ctrl Pts',(69.0245064207964,396.75768423162,58.6887810357227));
#31253=CARTESIAN_POINT('Ctrl Pts',(70.9158061804462,396.934780803619,59.8215807441396));
#31254=CARTESIAN_POINT('Ctrl Pts',(72.807105940096,397.111877375617,60.9543804525565));
#31255=CARTESIAN_POINT('Ctrl Pts',(75.1818659698097,397.288973947616,61.2464519739654));
#31256=CARTESIAN_POINT('Ctrl Pts',(77.2912945088662,397.466070519615,60.6057014773956));
#31257=CARTESIAN_POINT('Ctrl Pts',(79.4007230479228,397.643167091614,59.9649509808258));
#31258=CARTESIAN_POINT('Ctrl Pts',(81.2118275942073,397.820263663612,58.4014001198779));
#31259=CARTESIAN_POINT('Ctrl Pts',(82.1535440633097,397.997360235611,56.4080561826553));
#31260=CARTESIAN_POINT('Ctrl Pts',(82.651569792991,398.091017564953,55.3538784110939));
#31261=CARTESIAN_POINT('Ctrl Pts',(82.9129498948689,398.184674894296,54.188709927733));
#31262=CARTESIAN_POINT('Ctrl Pts',(82.9129498948689,398.278332223638,53.0228109606356));
#31263=CARTESIAN_POINT('Ctrl Pts',(82.9010717510546,399.721667776361,53.0276804110265));
#31264=CARTESIAN_POINT('Ctrl Pts',(82.9051844314699,399.631722269214,54.1519767949023));
#31265=CARTESIAN_POINT('Ctrl Pts',(82.682030927726,399.541776762067,55.2743640202701));
#31266=CARTESIAN_POINT('Ctrl Pts',(82.2236377097832,399.45183125492,56.2895162508407));
#31267=CARTESIAN_POINT('Ctrl Pts',(81.1424177688497,399.239675245368,58.6839732188166));
#31268=CARTESIAN_POINT('Ctrl Pts',(78.7524307261704,399.027519235815,60.4818233008151));
#31269=CARTESIAN_POINT('Ctrl Pts',(76.1506171505183,398.815363226263,60.8723217293589));
#31270=CARTESIAN_POINT('Ctrl Pts',(74.8497103626923,398.709285221487,61.0675709436308));
#31271=CARTESIAN_POINT('Ctrl Pts',(73.4958469416232,398.603207216711,60.9109822445391));
#31272=CARTESIAN_POINT('Ctrl Pts',(72.2527737980831,398.497129211935,60.4534117111886));
#31273=CARTESIAN_POINT('Ctrl Pts',(71.0097006545431,398.391051207159,59.9958411778381));
#31274=CARTESIAN_POINT('Ctrl Pts',(69.8774177885321,398.284973202383,59.2372888102288));
#31275=CARTESIAN_POINT('Ctrl Pts',(69.0135656461932,398.178895197606,58.2452000025176));
#31276=CARTESIAN_POINT('Ctrl Pts',(67.2858613615155,397.966739188054,56.2610223870953));
#31277=CARTESIAN_POINT('Ctrl Pts',(66.6318799715259,397.754583178501,53.3426990112652));
#31278=CARTESIAN_POINT('Ctrl Pts',(67.3611311303832,397.542427168949,50.8186836628596));
#31279=CARTESIAN_POINT('Ctrl Pts',(68.0903822892405,397.330271159396,48.294668314454));
#31280=CARTESIAN_POINT('Ctrl Pts',(70.2028659969447,397.118115149844,46.1649609934728));
#31281=CARTESIAN_POINT('Ctrl Pts',(72.7227932883516,396.905959140292,45.41403492531));
#31282=CARTESIAN_POINT('Ctrl Pts',(75.2427205797584,396.69380313074,44.6631088571472));
#31283=CARTESIAN_POINT('Ctrl Pts',(78.1700914548679,396.481647121188,45.2909640418026));
#31284=CARTESIAN_POINT('Ctrl Pts',(80.1632479148308,396.269491111635,47.0051009148426));
#31285=CARTESIAN_POINT('Ctrl Pts',(81.8788056026618,396.08688333321,48.4804997355617));
#31286=CARTESIAN_POINT('Ctrl Pts',(82.9022543906452,395.904275554785,50.7606658688838));
#31287=CARTESIAN_POINT('Ctrl Pts',(82.9211264258404,395.72166777636,53.027627219884));
#31288=CARTESIAN_POINT('Origin',(74.9879498948689,255.,53.0228109606356));
#31289=CARTESIAN_POINT('',(82.9098809662586,390.278332223638,53.0204521529043));
#31290=CARTESIAN_POINT('',(82.9135501799002,391.721667776361,53.0222178200602));
#31291=CARTESIAN_POINT('',(82.9129498948689,255.,53.0228109606356));
#31292=CARTESIAN_POINT('Ctrl Pts',(82.9082332267955,390.278332223638,53.0191856846757));
#31293=CARTESIAN_POINT('Ctrl Pts',(82.9121642338603,390.357600451624,52.0301359862952));
#31294=CARTESIAN_POINT('Ctrl Pts',(82.7366213310048,390.436868679611,51.0426507506166));
#31295=CARTESIAN_POINT('Ctrl Pts',(82.3762602245192,390.516136907597,50.1280769610102));
#31296=CARTESIAN_POINT('Ctrl Pts',(81.4117782839996,390.728292917149,47.6802825473726));
#31297=CARTESIAN_POINT('Ctrl Pts',(79.1233904318443,390.940448926702,45.7547737775995));
#31298=CARTESIAN_POINT('Ctrl Pts',(76.5473531371437,391.152604936254,45.2385445765189));
#31299=CARTESIAN_POINT('Ctrl Pts',(73.9713158424431,391.364760945806,44.7223153754382));
#31300=CARTESIAN_POINT('Ctrl Pts',(71.1076291051971,391.576916955359,45.6153657430501));
#31301=CARTESIAN_POINT('Ctrl Pts',(69.2797206269608,391.789072964911,47.5055176176273));
#31302=CARTESIAN_POINT('Ctrl Pts',(67.4518121487245,392.001228974463,49.3956694922046));
#31303=CARTESIAN_POINT('Ctrl Pts',(66.6596819294979,392.213384984015,52.2829228737472));
#31304=CARTESIAN_POINT('Ctrl Pts',(67.2621650360527,392.425540993568,54.8418195109206));
#31305=CARTESIAN_POINT('Ctrl Pts',(67.8646481426075,392.63769700312,57.400716148094));
#31306=CARTESIAN_POINT('Ctrl Pts',(69.8617445749438,392.849853012673,59.6312560408981));
#31307=CARTESIAN_POINT('Ctrl Pts',(72.34094729345,393.062009022225,60.5073139124612));
#31308=CARTESIAN_POINT('Ctrl Pts',(74.8201500119563,393.274165031777,61.3833717840243));
#31309=CARTESIAN_POINT('Ctrl Pts',(77.7814590166324,393.48632104133,60.9049476343463));
#31310=CARTESIAN_POINT('Ctrl Pts',(79.8565710669365,393.698477050882,59.2936218726151));
#31311=CARTESIAN_POINT('Ctrl Pts',(81.7471050800219,393.891762108467,57.8256210683852));
#31312=CARTESIAN_POINT('Ctrl Pts',(82.9020824215423,394.085047166052,55.4172950521791));
#31313=CARTESIAN_POINT('Ctrl Pts',(82.9194691672999,394.278332223638,53.0185305064141));
#31314=CARTESIAN_POINT('Ctrl Pts',(82.9129498948689,395.721667776361,53.0228109606487));
#31315=CARTESIAN_POINT('Ctrl Pts',(82.9129498948652,395.544571204362,55.2274084205586));
#31316=CARTESIAN_POINT('Ctrl Pts',(81.9432795991034,395.367474632363,57.4147653849932));
#31317=CARTESIAN_POINT('Ctrl Pts',(80.3096882702445,395.190378060364,58.8951806411014));
#31318=CARTESIAN_POINT('Ctrl Pts',(78.6760969413857,395.013281488366,60.3755958972096));
#31319=CARTESIAN_POINT('Ctrl Pts',(76.4041347530312,394.836184916367,61.1259150206704));
#31320=CARTESIAN_POINT('Ctrl Pts',(74.210180011209,394.659088344368,60.9095529374009));
#31321=CARTESIAN_POINT('Ctrl Pts',(72.0162252693868,394.481991772369,60.6931908541313));
#31322=CARTESIAN_POINT('Ctrl Pts',(69.9345925076872,394.304895200371,59.5135315737615));
#31323=CARTESIAN_POINT('Ctrl Pts',(68.621646765653,394.127798628372,57.7425365317822));
#31324=CARTESIAN_POINT('Ctrl Pts',(67.3087010236187,393.950702056373,55.971541489803));
#31325=CARTESIAN_POINT('Ctrl Pts',(66.7849774198229,393.773605484375,53.636909921617));
#31326=CARTESIAN_POINT('Ctrl Pts',(67.2156126057631,393.596508912376,51.4747805783835));
#31327=CARTESIAN_POINT('Ctrl Pts',(67.6462477917033,393.419412340377,49.31265123515));
#31328=CARTESIAN_POINT('Ctrl Pts',(69.0245064208059,393.242315768378,47.3568408855384));
#31329=CARTESIAN_POINT('Ctrl Pts',(70.9158061804576,393.06521919638,46.2240411771247));
#31330=CARTESIAN_POINT('Ctrl Pts',(72.8071059401093,392.888122624381,45.0912414687109));
#31331=CARTESIAN_POINT('Ctrl Pts',(75.1818659698234,392.711026052382,44.7991699473061));
#31332=CARTESIAN_POINT('Ctrl Pts',(77.291294508879,392.533929480383,45.4399204438794));
#31333=CARTESIAN_POINT('Ctrl Pts',(79.4007230479345,392.356832908385,46.0806709404527));
#31334=CARTESIAN_POINT('Ctrl Pts',(81.2118275942164,392.179736336386,47.6442218014037));
#31335=CARTESIAN_POINT('Ctrl Pts',(82.1535440633154,392.002639764387,49.6375657386279));
#31336=CARTESIAN_POINT('Ctrl Pts',(82.6515697929948,391.908982435045,50.6917435101901));
#31337=CARTESIAN_POINT('Ctrl Pts',(82.9129498948708,391.815325105703,51.8569119935513));
#31338=CARTESIAN_POINT('Ctrl Pts',(82.9129498948689,391.721667776361,53.0228109606485));
#31339=CARTESIAN_POINT('Origin',(74.9879498948689,255.,53.0228109606356));
#31340=CARTESIAN_POINT('',(82.90619017154,386.278332223638,53.0253308023074));
#31341=CARTESIAN_POINT('',(82.9082610542908,387.72166777636,53.0217421360302));
#31342=CARTESIAN_POINT('',(82.9129498948689,255.,53.0228109606356));
#31343=CARTESIAN_POINT('Ctrl Pts',(82.9129498948689,386.278332223638,53.022810960636));
#31344=CARTESIAN_POINT('Ctrl Pts',(82.912949894869,386.455428795637,50.8182135007262));
#31345=CARTESIAN_POINT('Ctrl Pts',(81.9432795991109,386.632525367635,48.6308565362899));
#31346=CARTESIAN_POINT('Ctrl Pts',(80.3096882702546,386.809621939634,47.1504412801789));
#31347=CARTESIAN_POINT('Ctrl Pts',(78.6760969413983,386.986718511633,45.6700260240679));
#31348=CARTESIAN_POINT('Ctrl Pts',(76.4041347530451,387.163815083631,44.9197069006032));
#31349=CARTESIAN_POINT('Ctrl Pts',(74.2101800112225,387.34091165563,45.136068983869));
#31350=CARTESIAN_POINT('Ctrl Pts',(72.0162252694,387.518008227629,45.3524310671347));
#31351=CARTESIAN_POINT('Ctrl Pts',(69.9345925076984,387.695104799628,46.532090347501));
#31352=CARTESIAN_POINT('Ctrl Pts',(68.6216467656611,387.872201371626,48.3030853894779));
#31353=CARTESIAN_POINT('Ctrl Pts',(67.3087010236239,388.049297943625,50.0740804314549));
#31354=CARTESIAN_POINT('Ctrl Pts',(66.784977419824,388.226394515624,52.40871199964));
#31355=CARTESIAN_POINT('Ctrl Pts',(67.2156126057604,388.403491087623,54.5708413428741));
#31356=CARTESIAN_POINT('Ctrl Pts',(67.6462477916969,388.580587659621,56.7329706861083));
#31357=CARTESIAN_POINT('Ctrl Pts',(69.024506420796,388.75768423162,58.6887810357223));
#31358=CARTESIAN_POINT('Ctrl Pts',(70.9158061804458,388.934780803619,59.8215807441393));
#31359=CARTESIAN_POINT('Ctrl Pts',(72.8071059400955,389.111877375617,60.9543804525564));
#31360=CARTESIAN_POINT('Ctrl Pts',(75.1818659698091,389.288973947616,61.2464519739654));
#31361=CARTESIAN_POINT('Ctrl Pts',(77.2912945088657,389.466070519615,60.6057014773958));
#31362=CARTESIAN_POINT('Ctrl Pts',(79.4007230479223,389.643167091614,59.9649509808262));
#31363=CARTESIAN_POINT('Ctrl Pts',(81.2118275942069,389.820263663612,58.4014001198783));
#31364=CARTESIAN_POINT('Ctrl Pts',(82.1535440633095,389.997360235611,56.4080561826558));
#31365=CARTESIAN_POINT('Ctrl Pts',(82.6515697929909,390.091017564953,55.3538784110942));
#31366=CARTESIAN_POINT('Ctrl Pts',(82.9129498948689,390.184674894296,54.1887099277329));
#31367=CARTESIAN_POINT('Ctrl Pts',(82.9129498948689,390.278332223638,53.0228109606353));
#31368=CARTESIAN_POINT('Ctrl Pts',(82.918916717821,391.721667776361,53.0169151530433));
#31369=CARTESIAN_POINT('Ctrl Pts',(82.9005549932558,391.5403608117,55.2681042080206));
#31370=CARTESIAN_POINT('Ctrl Pts',(81.8968913010544,391.35905384704,57.533901780382));
#31371=CARTESIAN_POINT('Ctrl Pts',(80.2020049922721,391.17774688238,59.0092987998488));
#31372=CARTESIAN_POINT('Ctrl Pts',(78.2187369110388,390.965590872827,60.7357318949143));
#31373=CARTESIAN_POINT('Ctrl Pts',(75.2890145455258,390.753434863275,61.3799116440399));
#31374=CARTESIAN_POINT('Ctrl Pts',(72.7667373037651,390.541278853723,60.6446713789343));
#31375=CARTESIAN_POINT('Ctrl Pts',(70.2444600620044,390.32912284417,59.9094311138287));
#31376=CARTESIAN_POINT('Ctrl Pts',(68.129627943996,390.116966834618,57.7947708344919));
#31377=CARTESIAN_POINT('Ctrl Pts',(67.3786141600463,389.904810825066,55.2732829401444));
#31378=CARTESIAN_POINT('Ctrl Pts',(67.0031072680715,389.79873282029,54.0125389929706));
#31379=CARTESIAN_POINT('Ctrl Pts',(66.9685549596114,389.692654815514,52.650088142044));
#31380=CARTESIAN_POINT('Ctrl Pts',(67.2475337798262,389.586576810738,51.3551856549928));
#31381=CARTESIAN_POINT('Ctrl Pts',(67.526512600041,389.480498805961,50.0602831679415));
#31382=CARTESIAN_POINT('Ctrl Pts',(68.1190225489307,389.374420801185,48.8329290447656));
#31383=CARTESIAN_POINT('Ctrl Pts',(68.9803591730895,389.268342796408,47.8386554676558));
#31384=CARTESIAN_POINT('Ctrl Pts',(70.7030324214069,389.056186786856,45.850108313436));
#31385=CARTESIAN_POINT('Ctrl Pts',(73.5010123708004,388.844030777304,44.7938833434809));
#31386=CARTESIAN_POINT('Ctrl Pts',(76.1022808095363,388.631874767752,45.162479655689));
#31387=CARTESIAN_POINT('Ctrl Pts',(78.7035492482722,388.4197187582,45.5310759678972));
#31388=CARTESIAN_POINT('Ctrl Pts',(81.1081061763504,388.207562748647,47.3244935622687));
#31389=CARTESIAN_POINT('Ctrl Pts',(82.2045282531435,387.995406739095,49.7144270641254));
#31390=CARTESIAN_POINT('Ctrl Pts',(82.6760891619508,387.904160418183,50.7423151721622));
#31391=CARTESIAN_POINT('Ctrl Pts',(82.9056739193359,387.812914097272,51.8805455919368));
#31392=CARTESIAN_POINT('Ctrl Pts',(82.9013757710113,387.72166777636,53.0201726307016));
#31393=CARTESIAN_POINT('Origin',(74.9879498948689,255.,53.0228109606356));
#31394=CARTESIAN_POINT('',(82.9169094223468,382.278332223638,53.0242849124606));
#31395=CARTESIAN_POINT('',(82.9129498948689,383.721667776361,53.0228109606488));
#31396=CARTESIAN_POINT('',(82.9129498948689,255.,53.0228109606356));
#31397=CARTESIAN_POINT('Ctrl Pts',(82.9257214576602,382.278332223638,53.0275652320441));
#31398=CARTESIAN_POINT('Ctrl Pts',(82.9150137442642,382.478395003663,50.5485677664457));
#31399=CARTESIAN_POINT('Ctrl Pts',(81.6577189855839,382.678457783688,48.0552956934044));
#31400=CARTESIAN_POINT('Ctrl Pts',(79.6514807652487,382.878520563714,46.5981796849265));
#31401=CARTESIAN_POINT('Ctrl Pts',(77.5239711156085,383.090676573266,45.0529851326245));
#31402=CARTESIAN_POINT('Ctrl Pts',(74.554238438814,383.302832582818,44.6729980251841));
#31403=CARTESIAN_POINT('Ctrl Pts',(72.1049313448895,383.514988592371,45.627897314676));
#31404=CARTESIAN_POINT('Ctrl Pts',(69.655624250965,383.727144601923,46.5827966041679));
#31405=CARTESIAN_POINT('Ctrl Pts',(67.7267427399103,383.939300611475,48.872582290592));
#31406=CARTESIAN_POINT('Ctrl Pts',(67.2065107590059,384.151456621028,51.4500388275331));
#31407=CARTESIAN_POINT('Ctrl Pts',(66.6862787781014,384.36361263058,54.0274953644742));
#31408=CARTESIAN_POINT('Ctrl Pts',(67.5746963273472,384.575768640132,56.8926227519322));
#31409=CARTESIAN_POINT('Ctrl Pts',(69.4607464568784,384.787924649684,58.7216322217361));
#31410=CARTESIAN_POINT('Ctrl Pts',(71.3467965864096,385.000080659237,60.55064169154));
#31411=CARTESIAN_POINT('Ctrl Pts',(74.2304792962261,385.212236668789,61.3435332436897));
#31412=CARTESIAN_POINT('Ctrl Pts',(76.7935642786192,385.424392678341,60.7498007466388));
#31413=CARTESIAN_POINT('Ctrl Pts',(78.0751067698158,385.530470683118,60.4529344981132));
#31414=CARTESIAN_POINT('Ctrl Pts',(79.2764998291565,385.636548687894,59.8094122372876));
#31415=CARTESIAN_POINT('Ctrl Pts',(80.2641755681491,385.74262669267,58.9267468036688));
#31416=CARTESIAN_POINT('Ctrl Pts',(81.2518513071416,385.848704697446,58.04408137005));
#31417=CARTESIAN_POINT('Ctrl Pts',(82.025809725786,385.954782702222,56.922272763638));
#31418=CARTESIAN_POINT('Ctrl Pts',(82.4642624635814,386.060860706998,55.6820147570218));
#31419=CARTESIAN_POINT('Ctrl Pts',(82.7638878259559,386.133351212545,54.8344598836305));
#31420=CARTESIAN_POINT('Ctrl Pts',(82.906833950516,386.205841718091,53.9315898164796));
#31421=CARTESIAN_POINT('Ctrl Pts',(82.9011087758377,386.278332223638,53.0272250089215));
#31422=CARTESIAN_POINT('Ctrl Pts',(82.9129498948689,387.721667776361,53.0228109606484));
#31423=CARTESIAN_POINT('Ctrl Pts',(82.9129498948653,387.544571204362,55.2274084205582));
#31424=CARTESIAN_POINT('Ctrl Pts',(81.9432795991036,387.367474632363,57.4147653849929));
#31425=CARTESIAN_POINT('Ctrl Pts',(80.3096882702448,387.190378060364,58.8951806411012));
#31426=CARTESIAN_POINT('Ctrl Pts',(78.676096941386,387.013281488366,60.3755958972095));
#31427=CARTESIAN_POINT('Ctrl Pts',(76.4041347530315,386.836184916367,61.1259150206703));
#31428=CARTESIAN_POINT('Ctrl Pts',(74.2101800112093,386.659088344368,60.9095529374009));
#31429=CARTESIAN_POINT('Ctrl Pts',(72.016225269387,386.48199177237,60.6931908541314));
#31430=CARTESIAN_POINT('Ctrl Pts',(69.9345925076875,386.304895200371,59.5135315737616));
#31431=CARTESIAN_POINT('Ctrl Pts',(68.6216467656532,386.127798628372,57.7425365317824));
#31432=CARTESIAN_POINT('Ctrl Pts',(67.3087010236189,385.950702056373,55.9715414898033));
#31433=CARTESIAN_POINT('Ctrl Pts',(66.7849774198229,385.773605484375,53.6369099216173));
#31434=CARTESIAN_POINT('Ctrl Pts',(67.2156126057631,385.596508912376,51.4747805783838));
#31435=CARTESIAN_POINT('Ctrl Pts',(67.6462477917032,385.419412340377,49.3126512351503));
#31436=CARTESIAN_POINT('Ctrl Pts',(69.0245064208057,385.242315768378,47.3568408855387));
#31437=CARTESIAN_POINT('Ctrl Pts',(70.9158061804574,385.06521919638,46.2240411771248));
#31438=CARTESIAN_POINT('Ctrl Pts',(72.807105940109,384.888122624381,45.091241468711));
#31439=CARTESIAN_POINT('Ctrl Pts',(75.1818659698231,384.711026052382,44.7991699473061));
#31440=CARTESIAN_POINT('Ctrl Pts',(77.2912945088787,384.533929480384,45.4399204438793));
#31441=CARTESIAN_POINT('Ctrl Pts',(79.4007230479342,384.356832908385,46.0806709404525));
#31442=CARTESIAN_POINT('Ctrl Pts',(81.2118275942162,384.179736336386,47.6442218014035));
#31443=CARTESIAN_POINT('Ctrl Pts',(82.1535440633153,384.002639764387,49.6375657386277));
#31444=CARTESIAN_POINT('Ctrl Pts',(82.6515697929949,383.908982435045,50.69174351019));
#31445=CARTESIAN_POINT('Ctrl Pts',(82.9129498948709,383.815325105703,51.8569119935516));
#31446=CARTESIAN_POINT('Ctrl Pts',(82.9129498948689,383.721667776361,53.0228109606491));
#31447=CARTESIAN_POINT('Origin',(74.9879498948689,255.,53.0228109606356));
#31448=CARTESIAN_POINT('',(82.9129498948689,378.278332223638,53.0228109606357));
#31449=CARTESIAN_POINT('',(82.917669415744,379.721667776361,53.0222330588015));
#31450=CARTESIAN_POINT('',(82.9129498948689,255.,53.0228109606356));
#31451=CARTESIAN_POINT('Ctrl Pts',(82.9129498948689,378.278332223638,53.0228109606356));
#31452=CARTESIAN_POINT('Ctrl Pts',(82.9129498948689,378.455428795637,50.8182135007257));
#31453=CARTESIAN_POINT('Ctrl Pts',(81.9432795991107,378.632525367635,48.6308565362895));
#31454=CARTESIAN_POINT('Ctrl Pts',(80.3096882702542,378.809621939634,47.1504412801785));
#31455=CARTESIAN_POINT('Ctrl Pts',(78.6760969413978,378.986718511633,45.6700260240676));
#31456=CARTESIAN_POINT('Ctrl Pts',(76.4041347530444,379.163815083631,44.9197069006031));
#31457=CARTESIAN_POINT('Ctrl Pts',(74.2101800112218,379.34091165563,45.136068983869));
#31458=CARTESIAN_POINT('Ctrl Pts',(72.0162252693992,379.518008227629,45.352431067135));
#31459=CARTESIAN_POINT('Ctrl Pts',(69.9345925076977,379.695104799628,46.5320903475015));
#31460=CARTESIAN_POINT('Ctrl Pts',(68.6216467656606,379.872201371626,48.3030853894787));
#31461=CARTESIAN_POINT('Ctrl Pts',(67.3087010236235,380.049297943625,50.0740804314558));
#31462=CARTESIAN_POINT('Ctrl Pts',(66.7849774198239,380.226394515624,52.408711999641));
#31463=CARTESIAN_POINT('Ctrl Pts',(67.2156126057606,380.403491087623,54.5708413428752));
#31464=CARTESIAN_POINT('Ctrl Pts',(67.6462477916974,380.580587659621,56.7329706861094));
#31465=CARTESIAN_POINT('Ctrl Pts',(69.0245064207969,380.75768423162,58.6887810357232));
#31466=CARTESIAN_POINT('Ctrl Pts',(70.9158061804468,380.934780803619,59.82158074414));
#31467=CARTESIAN_POINT('Ctrl Pts',(72.8071059400968,381.111877375617,60.9543804525568));
#31468=CARTESIAN_POINT('Ctrl Pts',(75.1818659698105,381.288973947616,61.2464519739654));
#31469=CARTESIAN_POINT('Ctrl Pts',(77.2912945088671,381.466070519615,60.6057014773954));
#31470=CARTESIAN_POINT('Ctrl Pts',(79.4007230479236,381.643167091614,59.9649509808253));
#31471=CARTESIAN_POINT('Ctrl Pts',(81.211827594208,381.820263663612,58.4014001198771));
#31472=CARTESIAN_POINT('Ctrl Pts',(82.1535440633102,381.997360235611,56.4080561826543));
#31473=CARTESIAN_POINT('Ctrl Pts',(82.6515697929911,382.091017564953,55.3538784110933));
#31474=CARTESIAN_POINT('Ctrl Pts',(82.9129498948689,382.184674894296,54.1887099277327));
#31475=CARTESIAN_POINT('Ctrl Pts',(82.9129498948689,382.278332223638,53.0228109606358));
#31476=CARTESIAN_POINT('Ctrl Pts',(82.9129498948689,383.721667776361,53.0228109606491));
#31477=CARTESIAN_POINT('Ctrl Pts',(82.9129498948652,383.544571204362,55.2274084205589));
#31478=CARTESIAN_POINT('Ctrl Pts',(81.9432795991032,383.367474632363,57.4147653849935));
#31479=CARTESIAN_POINT('Ctrl Pts',(80.3096882702443,383.190378060364,58.8951806411016));
#31480=CARTESIAN_POINT('Ctrl Pts',(78.6760969413854,383.013281488366,60.3755958972097));
#31481=CARTESIAN_POINT('Ctrl Pts',(76.4041347530309,382.836184916367,61.1259150206704));
#31482=CARTESIAN_POINT('Ctrl Pts',(74.2101800112088,382.659088344368,60.9095529374008));
#31483=CARTESIAN_POINT('Ctrl Pts',(72.0162252693866,382.481991772369,60.6931908541312));
#31484=CARTESIAN_POINT('Ctrl Pts',(69.9345925076871,382.304895200371,59.5135315737613));
#31485=CARTESIAN_POINT('Ctrl Pts',(68.6216467656529,382.127798628372,57.7425365317821));
#31486=CARTESIAN_POINT('Ctrl Pts',(67.3087010236187,381.950702056373,55.9715414898029));
#31487=CARTESIAN_POINT('Ctrl Pts',(66.7849774198229,381.773605484375,53.6369099216169));
#31488=CARTESIAN_POINT('Ctrl Pts',(67.2156126057631,381.596508912376,51.4747805783835));
#31489=CARTESIAN_POINT('Ctrl Pts',(67.6462477917033,381.419412340377,49.3126512351501));
#31490=CARTESIAN_POINT('Ctrl Pts',(69.0245064208058,381.242315768378,47.3568408855385));
#31491=CARTESIAN_POINT('Ctrl Pts',(70.9158061804575,381.06521919638,46.2240411771248));
#31492=CARTESIAN_POINT('Ctrl Pts',(72.8071059401092,380.888122624381,45.091241468711));
#31493=CARTESIAN_POINT('Ctrl Pts',(75.1818659698232,380.711026052382,44.7991699473061));
#31494=CARTESIAN_POINT('Ctrl Pts',(77.2912945088787,380.533929480384,45.4399204438793));
#31495=CARTESIAN_POINT('Ctrl Pts',(79.4007230479342,380.356832908385,46.0806709404526));
#31496=CARTESIAN_POINT('Ctrl Pts',(81.2118275942161,380.179736336386,47.6442218014035));
#31497=CARTESIAN_POINT('Ctrl Pts',(82.1535440633153,380.002639764387,49.6375657386276));
#31498=CARTESIAN_POINT('Ctrl Pts',(82.6515697929948,379.908982435045,50.69174351019));
#31499=CARTESIAN_POINT('Ctrl Pts',(82.9129498948709,379.815325105703,51.8569119935514));
#31500=CARTESIAN_POINT('Ctrl Pts',(82.9129498948689,379.721667776361,53.0228109606489));
#31501=CARTESIAN_POINT('Origin',(74.9879498948689,255.,53.0228109606356));
#31502=CARTESIAN_POINT('',(82.9087440841051,374.278332223638,53.0229220451327));
#31503=CARTESIAN_POINT('',(82.9105410465356,375.721667776361,53.0211223461501));
#31504=CARTESIAN_POINT('',(82.9129498948689,255.,53.0228109606356));
#31505=CARTESIAN_POINT('Ctrl Pts',(82.9129498948689,374.278332223638,53.0228109606354));
#31506=CARTESIAN_POINT('Ctrl Pts',(82.9129498948689,374.455428795637,50.8182135007257));
#31507=CARTESIAN_POINT('Ctrl Pts',(81.9432795991107,374.632525367635,48.6308565362895));
#31508=CARTESIAN_POINT('Ctrl Pts',(80.3096882702543,374.809621939634,47.1504412801786));
#31509=CARTESIAN_POINT('Ctrl Pts',(78.676096941398,374.986718511633,45.6700260240677));
#31510=CARTESIAN_POINT('Ctrl Pts',(76.4041347530448,375.163815083631,44.9197069006031));
#31511=CARTESIAN_POINT('Ctrl Pts',(74.2101800112223,375.34091165563,45.136068983869));
#31512=CARTESIAN_POINT('Ctrl Pts',(72.0162252693998,375.518008227629,45.3524310671348));
#31513=CARTESIAN_POINT('Ctrl Pts',(69.9345925076983,375.695104799628,46.5320903475011));
#31514=CARTESIAN_POINT('Ctrl Pts',(68.6216467656611,375.872201371626,48.303085389478));
#31515=CARTESIAN_POINT('Ctrl Pts',(67.3087010236239,376.049297943625,50.0740804314549));
#31516=CARTESIAN_POINT('Ctrl Pts',(66.784977419824,376.226394515624,52.4087119996399));
#31517=CARTESIAN_POINT('Ctrl Pts',(67.2156126057604,376.403491087623,54.570841342874));
#31518=CARTESIAN_POINT('Ctrl Pts',(67.6462477916968,376.580587659621,56.7329706861082));
#31519=CARTESIAN_POINT('Ctrl Pts',(69.0245064207959,376.75768423162,58.6887810357221));
#31520=CARTESIAN_POINT('Ctrl Pts',(70.9158061804455,376.934780803619,59.8215807441392));
#31521=CARTESIAN_POINT('Ctrl Pts',(72.8071059400951,377.111877375617,60.9543804525563));
#31522=CARTESIAN_POINT('Ctrl Pts',(75.1818659698087,377.288973947616,61.2464519739654));
#31523=CARTESIAN_POINT('Ctrl Pts',(77.2912945088653,377.466070519615,60.6057014773959));
#31524=CARTESIAN_POINT('Ctrl Pts',(79.4007230479219,377.643167091614,59.9649509808264));
#31525=CARTESIAN_POINT('Ctrl Pts',(81.2118275942065,377.820263663612,58.4014001198787));
#31526=CARTESIAN_POINT('Ctrl Pts',(82.1535440633092,377.997360235611,56.4080561826563));
#31527=CARTESIAN_POINT('Ctrl Pts',(82.6515697929908,378.091017564953,55.3538784110947));
#31528=CARTESIAN_POINT('Ctrl Pts',(82.9129498948689,378.184674894296,54.1887099277333));
#31529=CARTESIAN_POINT('Ctrl Pts',(82.9129498948689,378.278332223638,53.0228109606356));
#31530=CARTESIAN_POINT('Ctrl Pts',(82.9268750308129,379.721667776361,53.0211058379808));
#31531=CARTESIAN_POINT('Ctrl Pts',(82.9277596348217,379.509396630207,55.6497794910386));
#31532=CARTESIAN_POINT('Ctrl Pts',(81.4883940862173,379.297125484052,58.28388116542));
#31533=CARTESIAN_POINT('Ctrl Pts',(79.2743564499831,379.084854337897,59.7049607683006));
#31534=CARTESIAN_POINT('Ctrl Pts',(77.0615197154011,378.872698328345,61.1252695727021));
#31535=CARTESIAN_POINT('Ctrl Pts',(74.0748514262754,378.660542318793,61.3338718358065));
#31536=CARTESIAN_POINT('Ctrl Pts',(71.6845021330615,378.448386309241,60.2397200411031));
#31537=CARTESIAN_POINT('Ctrl Pts',(69.2941528398476,378.236230299689,59.1455682463996));
#31538=CARTESIAN_POINT('Ctrl Pts',(67.5001225425455,378.024074290136,56.7486623938882));
#31539=CARTESIAN_POINT('Ctrl Pts',(67.1289520079351,377.811918280584,54.1455573349225));
#31540=CARTESIAN_POINT('Ctrl Pts',(66.7577814733247,377.599762271031,51.5424522759567));
#31541=CARTESIAN_POINT('Ctrl Pts',(67.809470701406,377.387606261479,48.7331480105366));
#31542=CARTESIAN_POINT('Ctrl Pts',(69.7975664214702,377.175450251927,47.0156101973868));
#31543=CARTESIAN_POINT('Ctrl Pts',(71.7856621415344,376.963294242375,45.2980723842371));
#31544=CARTESIAN_POINT('Ctrl Pts',(74.7101643535816,376.751138232822,44.6723010233578));
#31545=CARTESIAN_POINT('Ctrl Pts',(77.2348699696133,376.53898222327,45.4124256462436));
#31546=CARTESIAN_POINT('Ctrl Pts',(78.4972227776292,376.432904218494,45.7824879576864));
#31547=CARTESIAN_POINT('Ctrl Pts',(79.6596264366412,376.326826213718,46.4940242650705));
#31548=CARTESIAN_POINT('Ctrl Pts',(80.5949158999949,376.220748208942,47.4320196023935));
#31549=CARTESIAN_POINT('Ctrl Pts',(81.5302053633485,376.114670204165,48.3700149397164));
#31550=CARTESIAN_POINT('Ctrl Pts',(82.2383806310438,376.008592199389,49.5344693069782));
#31551=CARTESIAN_POINT('Ctrl Pts',(82.6047945844103,375.902514194613,50.7978859211772));
#31552=CARTESIAN_POINT('Ctrl Pts',(82.8130207578564,375.842232055196,51.5158618733096));
#31553=CARTESIAN_POINT('Ctrl Pts',(82.9108773156051,375.781949915778,52.2657970458251));
#31554=CARTESIAN_POINT('Ctrl Pts',(82.9047414110188,375.721667776361,53.0170567732019));
#31555=CARTESIAN_POINT('Origin',(74.9879498948689,255.,53.0228109606356));
#31556=CARTESIAN_POINT('',(82.9146081634051,370.278332223638,53.029785282215));
#31557=CARTESIAN_POINT('',(82.9117595115795,371.72166777636,53.02320991057));
#31558=CARTESIAN_POINT('',(82.9129498948689,255.,53.0228109606356));
#31559=CARTESIAN_POINT('Ctrl Pts',(82.9146081634051,370.278332223638,53.029785282215));
#31560=CARTESIAN_POINT('Ctrl Pts',(82.895835554435,370.447430822169,50.9271921297301));
#31561=CARTESIAN_POINT('Ctrl Pts',(82.0366188183737,370.616529420701,48.8106954290504));
#31562=CARTESIAN_POINT('Ctrl Pts',(80.5375948247923,370.785628019232,47.3460294464692));
#31563=CARTESIAN_POINT('Ctrl Pts',(78.6568758155066,370.997784028784,45.5084169949747));
#31564=CARTESIAN_POINT('Ctrl Pts',(75.7690400495532,371.209940038336,44.6968473571427));
#31565=CARTESIAN_POINT('Ctrl Pts',(73.2086602687691,371.422096047889,45.2858432059296));
#31566=CARTESIAN_POINT('Ctrl Pts',(70.6482804879848,371.634252057441,45.8748390547165));
#31567=CARTESIAN_POINT('Ctrl Pts',(68.4153566923697,371.846408066993,47.8644003901223));
#31568=CARTESIAN_POINT('Ctrl Pts',(67.5206027772723,372.058564076546,50.3385342459275));
#31569=CARTESIAN_POINT('Ctrl Pts',(67.0732258197235,372.164642081322,51.5756011738301));
#31570=CARTESIAN_POINT('Ctrl Pts',(66.9603913323042,372.270720086098,52.9338112318324));
#31571=CARTESIAN_POINT('Ctrl Pts',(67.1644532117948,372.376798090874,54.2426123559298));
#31572=CARTESIAN_POINT('Ctrl Pts',(67.3685150912855,372.48287609565,55.5514134800272));
#31573=CARTESIAN_POINT('Ctrl Pts',(67.8894733376861,372.588954100426,56.8108056702197));
#31574=CARTESIAN_POINT('Ctrl Pts',(68.6922153662661,372.695032105203,57.8529601509983));
#31575=CARTESIAN_POINT('Ctrl Pts',(70.2976994234263,372.907188114755,59.9372691125558));
#31576=CARTESIAN_POINT('Ctrl Pts',(73.0303186093043,373.119344124307,61.1526272364583));
#31577=CARTESIAN_POINT('Ctrl Pts',(75.6484772999912,373.33150013386,60.9342106571487));
#31578=CARTESIAN_POINT('Ctrl Pts',(78.2666359906781,373.543656143412,60.7157940778391));
#31579=CARTESIAN_POINT('Ctrl Pts',(80.770334186174,373.755812152964,59.0636027953172));
#31580=CARTESIAN_POINT('Ctrl Pts',(82.0023607164196,373.967968162516,56.7406662609825));
#31581=CARTESIAN_POINT('Ctrl Pts',(82.6031399231037,374.071422849557,55.6079211990747));
#31582=CARTESIAN_POINT('Ctrl Pts',(82.9015310543615,374.174877536597,54.315681063604));
#31583=CARTESIAN_POINT('Ctrl Pts',(82.9001803294088,374.278332223638,53.0231482322911));
#31584=CARTESIAN_POINT('Ctrl Pts',(82.9129498948689,375.721667776361,53.0228109606487));
#31585=CARTESIAN_POINT('Ctrl Pts',(82.9129498948652,375.544571204362,55.2274084205585));
#31586=CARTESIAN_POINT('Ctrl Pts',(81.9432795991034,375.367474632363,57.4147653849932));
#31587=CARTESIAN_POINT('Ctrl Pts',(80.3096882702445,375.190378060364,58.8951806411014));
#31588=CARTESIAN_POINT('Ctrl Pts',(78.6760969413857,375.013281488366,60.3755958972096));
#31589=CARTESIAN_POINT('Ctrl Pts',(76.4041347530311,374.836184916367,61.1259150206704));
#31590=CARTESIAN_POINT('Ctrl Pts',(74.2101800112089,374.659088344368,60.9095529374008));
#31591=CARTESIAN_POINT('Ctrl Pts',(72.0162252693867,374.481991772369,60.6931908541313));
#31592=CARTESIAN_POINT('Ctrl Pts',(69.9345925076872,374.304895200371,59.5135315737614));
#31593=CARTESIAN_POINT('Ctrl Pts',(68.621646765653,374.127798628372,57.7425365317822));
#31594=CARTESIAN_POINT('Ctrl Pts',(67.3087010236187,373.950702056373,55.9715414898029));
#31595=CARTESIAN_POINT('Ctrl Pts',(66.7849774198229,373.773605484375,53.6369099216169));
#31596=CARTESIAN_POINT('Ctrl Pts',(67.2156126057631,373.596508912376,51.4747805783835));
#31597=CARTESIAN_POINT('Ctrl Pts',(67.6462477917033,373.419412340377,49.31265123515));
#31598=CARTESIAN_POINT('Ctrl Pts',(69.0245064208059,373.242315768378,47.3568408855384));
#31599=CARTESIAN_POINT('Ctrl Pts',(70.9158061804577,373.06521919638,46.2240411771247));
#31600=CARTESIAN_POINT('Ctrl Pts',(72.8071059401094,372.888122624381,45.0912414687109));
#31601=CARTESIAN_POINT('Ctrl Pts',(75.1818659698235,372.711026052382,44.7991699473061));
#31602=CARTESIAN_POINT('Ctrl Pts',(77.291294508879,372.533929480383,45.4399204438794));
#31603=CARTESIAN_POINT('Ctrl Pts',(79.4007230479345,372.356832908385,46.0806709404527));
#31604=CARTESIAN_POINT('Ctrl Pts',(81.2118275942164,372.179736336386,47.6442218014038));
#31605=CARTESIAN_POINT('Ctrl Pts',(82.1535440633154,372.002639764387,49.637565738628));
#31606=CARTESIAN_POINT('Ctrl Pts',(82.6515697929949,371.908982435045,50.6917435101901));
#31607=CARTESIAN_POINT('Ctrl Pts',(82.9129498948708,371.815325105703,51.8569119935514));
#31608=CARTESIAN_POINT('Ctrl Pts',(82.9129498948689,371.721667776361,53.0228109606486));
#31609=CARTESIAN_POINT('Origin',(74.9879498948689,255.,53.0228109606356));
#31610=CARTESIAN_POINT('',(82.9246351989638,366.278332223638,53.0200841918108));
#31611=CARTESIAN_POINT('',(82.9134155880036,367.721667776361,53.023873582756));
#31612=CARTESIAN_POINT('',(82.9129498948689,255.,53.0228109606356));
#31613=CARTESIAN_POINT('Ctrl Pts',(82.9246351989638,366.278332223638,53.0200841918108));
#31614=CARTESIAN_POINT('Ctrl Pts',(82.9259058467681,366.295672088636,52.8050527487061));
#31615=CARTESIAN_POINT('Ctrl Pts',(82.9179101534511,366.313011953635,52.590100792154));
#31616=CARTESIAN_POINT('Ctrl Pts',(82.9003407545765,366.330351818633,52.3759121346824));
#31617=CARTESIAN_POINT('Ctrl Pts',(82.6853763614975,366.542507828186,49.7552798019267));
#31618=CARTESIAN_POINT('Ctrl Pts',(81.0372366544246,366.754663837738,47.2489126711698));
#31619=CARTESIAN_POINT('Ctrl Pts',(78.7179356483762,366.96681984729,46.0146908211446));
#31620=CARTESIAN_POINT('Ctrl Pts',(76.3986346423277,367.178975856842,44.7804689711194));
#31621=CARTESIAN_POINT('Ctrl Pts',(73.4081723373038,367.391131866395,44.8183924018261));
#31622=CARTESIAN_POINT('Ctrl Pts',(71.110277134158,367.603287875947,46.0996420029512));
#31623=CARTESIAN_POINT('Ctrl Pts',(69.9613295325851,367.709365880723,46.7402668035138));
#31624=CARTESIAN_POINT('Ctrl Pts',(68.9855237064817,367.815443885499,47.691723146681));
#31625=CARTESIAN_POINT('Ctrl Pts',(68.2813726222647,367.921521890276,48.8136736285187));
#31626=CARTESIAN_POINT('Ctrl Pts',(67.5772215380476,368.027599895052,49.9356241103564));
#31627=CARTESIAN_POINT('Ctrl Pts',(67.1447251957169,368.133677899828,51.2280687308647));
#31628=CARTESIAN_POINT('Ctrl Pts',(67.0674236777374,368.239755904604,52.5412729044698));
#31629=CARTESIAN_POINT('Ctrl Pts',(66.9128206417784,368.451911914156,55.1676812516801));
#31630=CARTESIAN_POINT('Ctrl Pts',(68.1789969032245,368.664067923708,57.8771278112779));
#31631=CARTESIAN_POINT('Ctrl Pts',(70.2989217094926,368.876223933261,59.4290232805367));
#31632=CARTESIAN_POINT('Ctrl Pts',(72.4188465157607,369.088379942813,60.9809187497954));
#31633=CARTESIAN_POINT('Ctrl Pts',(75.3925198668508,369.300535952365,61.3752631287152));
#31634=CARTESIAN_POINT('Ctrl Pts',(77.8459107292913,369.512691961918,60.4293261382823));
#31635=CARTESIAN_POINT('Ctrl Pts',(80.2993015917319,369.72484797147,59.4833891478494));
#31636=CARTESIAN_POINT('Ctrl Pts',(82.2324099655229,369.937003981022,57.1971707880637));
#31637=CARTESIAN_POINT('Ctrl Pts',(82.7621630261094,370.149159990575,54.6222339755923));
#31638=CARTESIAN_POINT('Ctrl Pts',(82.8696772809139,370.192217401596,54.0996463151173));
#31639=CARTESIAN_POINT('Ctrl Pts',(82.9193882144959,370.235274812617,53.5651665234718));
#31640=CARTESIAN_POINT('Ctrl Pts',(82.9146081634051,370.278332223638,53.029785282215));
#31641=CARTESIAN_POINT('Ctrl Pts',(82.9066444346458,371.721667776361,53.0249241981763));
#31642=CARTESIAN_POINT('Ctrl Pts',(82.9091713020796,371.630191182245,54.1669385451946));
#31643=CARTESIAN_POINT('Ctrl Pts',(82.6734524996546,371.53871458813,55.3078024227671));
#31644=CARTESIAN_POINT('Ctrl Pts',(82.1975929589684,371.447237994014,56.3375751067078));
#31645=CARTESIAN_POINT('Ctrl Pts',(81.093961344394,371.235081984462,58.7258632309372));
#31646=CARTESIAN_POINT('Ctrl Pts',(78.6986449422475,371.02292597491,60.5166067407603));
#31647=CARTESIAN_POINT('Ctrl Pts',(76.0971869326856,370.810769965358,60.8838627226355));
#31648=CARTESIAN_POINT('Ctrl Pts',(73.4957289231237,370.598613955805,61.2511187045107));
#31649=CARTESIAN_POINT('Ctrl Pts',(70.6881293061464,370.386457946253,60.1948871584381));
#31650=CARTESIAN_POINT('Ctrl Pts',(68.9719265086356,370.1743019367,58.2027597851027));
#31651=CARTESIAN_POINT('Ctrl Pts',(67.2557237111248,369.962145927148,56.2106324117673));
#31652=CARTESIAN_POINT('Ctrl Pts',(66.6309177330805,369.749989917596,53.2826092111691));
#31653=CARTESIAN_POINT('Ctrl Pts',(67.3795376632359,369.537833908044,50.7625881609405));
#31654=CARTESIAN_POINT('Ctrl Pts',(68.1281575933913,369.325677898491,48.2425671107118));
#31655=CARTESIAN_POINT('Ctrl Pts',(70.2502034317463,369.113521888939,46.1305482108527));
#31656=CARTESIAN_POINT('Ctrl Pts',(72.7756768019202,368.901365879387,45.3984909929256));
#31657=CARTESIAN_POINT('Ctrl Pts',(75.3011501720939,368.689209869834,44.6664337749986));
#31658=CARTESIAN_POINT('Ctrl Pts',(78.2300510740863,368.477053860282,45.3143382390034));
#31659=CARTESIAN_POINT('Ctrl Pts',(80.2090806414343,368.26489785073,47.0423147154921));
#31660=CARTESIAN_POINT('Ctrl Pts',(81.8981967174103,368.083821159273,48.517155159264));
#31661=CARTESIAN_POINT('Ctrl Pts',(82.8953556346456,367.902744467817,50.778800650978));
#31662=CARTESIAN_POINT('Ctrl Pts',(82.9154483188492,367.72166777636,53.0285118833292));
#31663=CARTESIAN_POINT('Origin',(74.9879498948689,255.,53.0228109606356));
#31664=CARTESIAN_POINT('',(82.9101891893477,362.278332223638,53.0206763621601));
#31665=CARTESIAN_POINT('',(82.9152412871326,363.721667776361,53.0213275785589));
#31666=CARTESIAN_POINT('',(82.9129498948689,255.,53.0228109606356));
#31667=CARTESIAN_POINT('Ctrl Pts',(82.9036741822449,362.278332223638,53.0156389091875));
#31668=CARTESIAN_POINT('Ctrl Pts',(82.9096131525181,362.356069364656,52.0448043091272));
#31669=CARTESIAN_POINT('Ctrl Pts',(82.7445708386648,362.433806505673,51.0762468411838));
#31670=CARTESIAN_POINT('Ctrl Pts',(82.3994985579666,362.511543646691,50.1775538500318));
#31671=CARTESIAN_POINT('Ctrl Pts',(81.4577459141023,362.723699656244,47.7248894438173));
#31672=CARTESIAN_POINT('Ctrl Pts',(79.1750872235282,362.935855665796,45.7925922910192));
#31673=CARTESIAN_POINT('Ctrl Pts',(76.6000313647351,363.148011675349,45.2531386515664));
#31674=CARTESIAN_POINT('Ctrl Pts',(75.3125034353385,363.254089680125,44.98341183184));
#31675=CARTESIAN_POINT('Ctrl Pts',(73.9518762138872,363.360167684901,45.0618958904499));
#31676=CARTESIAN_POINT('Ctrl Pts',(72.6845498691734,363.466245689677,45.4472341432798));
#31677=CARTESIAN_POINT('Ctrl Pts',(71.4172235244595,363.572323694453,45.8325723961097));
#31678=CARTESIAN_POINT('Ctrl Pts',(70.243198056483,363.678401699229,46.5247648431596));
#31679=CARTESIAN_POINT('Ctrl Pts',(69.323731138859,363.784479704005,47.4655418165443));
#31680=CARTESIAN_POINT('Ctrl Pts',(67.484797303611,363.996635713558,49.3470957633138));
#31681=CARTESIAN_POINT('Ctrl Pts',(66.6640976697729,364.20879172311,52.2229878154227));
#31682=CARTESIAN_POINT('Ctrl Pts',(67.2470143817554,364.420947732662,54.7847584606265));
#31683=CARTESIAN_POINT('Ctrl Pts',(67.8299310937379,364.633103742214,57.3465291058304));
#31684=CARTESIAN_POINT('Ctrl Pts',(69.816464151541,364.845259751767,59.5941783441292));
#31685=CARTESIAN_POINT('Ctrl Pts',(72.2890450298562,365.057415761319,60.4887549556984));
#31686=CARTESIAN_POINT('Ctrl Pts',(74.7616259081713,365.269571770872,61.3833315672676));
#31687=CARTESIAN_POINT('Ctrl Pts',(77.7202546069985,365.481727780424,60.9248355521071));
#31688=CARTESIAN_POINT('Ctrl Pts',(79.8086744168695,365.693883789976,59.3281387771497));
#31689=CARTESIAN_POINT('Ctrl Pts',(81.7264041876525,365.88869993453,57.8619426963731));
#31690=CARTESIAN_POINT('Ctrl Pts',(82.9103592685377,366.083516079084,55.435996697892));
#31691=CARTESIAN_POINT('Ctrl Pts',(82.9246351989638,366.278332223638,53.0200841918108));
#31692=CARTESIAN_POINT('Ctrl Pts',(82.9129498948689,367.721667776361,53.0228109606493));
#31693=CARTESIAN_POINT('Ctrl Pts',(82.9129498948651,367.544571204362,55.2274084205591));
#31694=CARTESIAN_POINT('Ctrl Pts',(81.9432795991031,367.367474632363,57.4147653849936));
#31695=CARTESIAN_POINT('Ctrl Pts',(80.3096882702442,367.190378060364,58.8951806411017));
#31696=CARTESIAN_POINT('Ctrl Pts',(78.6760969413853,367.013281488366,60.3755958972098));
#31697=CARTESIAN_POINT('Ctrl Pts',(76.4041347530308,366.836184916367,61.1259150206705));
#31698=CARTESIAN_POINT('Ctrl Pts',(74.2101800112086,366.659088344368,60.9095529374008));
#31699=CARTESIAN_POINT('Ctrl Pts',(72.0162252693864,366.481991772369,60.6931908541312));
#31700=CARTESIAN_POINT('Ctrl Pts',(69.934592507687,366.304895200371,59.5135315737612));
#31701=CARTESIAN_POINT('Ctrl Pts',(68.6216467656528,366.127798628372,57.742536531782));
#31702=CARTESIAN_POINT('Ctrl Pts',(67.3087010236187,365.950702056373,55.9715414898028));
#31703=CARTESIAN_POINT('Ctrl Pts',(66.7849774198229,365.773605484375,53.6369099216168));
#31704=CARTESIAN_POINT('Ctrl Pts',(67.2156126057631,365.596508912376,51.4747805783834));
#31705=CARTESIAN_POINT('Ctrl Pts',(67.6462477917034,365.419412340377,49.31265123515));
#31706=CARTESIAN_POINT('Ctrl Pts',(69.024506420806,365.242315768378,47.3568408855384));
#31707=CARTESIAN_POINT('Ctrl Pts',(70.9158061804577,365.06521919638,46.2240411771247));
#31708=CARTESIAN_POINT('Ctrl Pts',(72.8071059401093,364.888122624381,45.091241468711));
#31709=CARTESIAN_POINT('Ctrl Pts',(75.1818659698234,364.711026052382,44.7991699473061));
#31710=CARTESIAN_POINT('Ctrl Pts',(77.2912945088789,364.533929480384,45.4399204438794));
#31711=CARTESIAN_POINT('Ctrl Pts',(79.4007230479344,364.356832908385,46.0806709404526));
#31712=CARTESIAN_POINT('Ctrl Pts',(81.2118275942163,364.179736336386,47.6442218014036));
#31713=CARTESIAN_POINT('Ctrl Pts',(82.1535440633153,364.002639764387,49.6375657386278));
#31714=CARTESIAN_POINT('Ctrl Pts',(82.6515697929949,363.908982435045,50.6917435101901));
#31715=CARTESIAN_POINT('Ctrl Pts',(82.9129498948709,363.815325105703,51.8569119935516));
#31716=CARTESIAN_POINT('Ctrl Pts',(82.9129498948689,363.721667776361,53.0228109606491));
#31717=CARTESIAN_POINT('Origin',(74.9879498948689,255.,53.0228109606356));
#31718=CARTESIAN_POINT('',(82.910167501573,358.278332223638,53.0247970047267));
#31719=CARTESIAN_POINT('',(82.9091777645014,359.721667776361,53.0220250865809));
#31720=CARTESIAN_POINT('',(82.9129498948689,255.,53.0228109606356));
#31721=CARTESIAN_POINT('Ctrl Pts',(82.9129498948689,358.278332223638,53.0228109606355));
#31722=CARTESIAN_POINT('Ctrl Pts',(82.9129498948689,358.455428795637,50.8182135007257));
#31723=CARTESIAN_POINT('Ctrl Pts',(81.9432795991106,358.632525367635,48.6308565362894));
#31724=CARTESIAN_POINT('Ctrl Pts',(80.3096882702542,358.809621939634,47.1504412801785));
#31725=CARTESIAN_POINT('Ctrl Pts',(78.6760969413977,358.986718511633,45.6700260240675));
#31726=CARTESIAN_POINT('Ctrl Pts',(76.4041347530443,359.163815083631,44.919706900603));
#31727=CARTESIAN_POINT('Ctrl Pts',(74.2101800112218,359.34091165563,45.136068983869));
#31728=CARTESIAN_POINT('Ctrl Pts',(72.0162252693992,359.518008227629,45.352431067135));
#31729=CARTESIAN_POINT('Ctrl Pts',(69.9345925076977,359.695104799628,46.5320903475016));
#31730=CARTESIAN_POINT('Ctrl Pts',(68.6216467656606,359.872201371626,48.3030853894787));
#31731=CARTESIAN_POINT('Ctrl Pts',(67.3087010236235,360.049297943625,50.0740804314559));
#31732=CARTESIAN_POINT('Ctrl Pts',(66.7849774198239,360.226394515624,52.4087119996411));
#31733=CARTESIAN_POINT('Ctrl Pts',(67.2156126057607,360.403491087623,54.5708413428753));
#31734=CARTESIAN_POINT('Ctrl Pts',(67.6462477916974,360.580587659621,56.7329706861094));
#31735=CARTESIAN_POINT('Ctrl Pts',(69.0245064207969,360.75768423162,58.6887810357233));
#31736=CARTESIAN_POINT('Ctrl Pts',(70.9158061804469,360.934780803619,59.82158074414));
#31737=CARTESIAN_POINT('Ctrl Pts',(72.8071059400968,361.111877375618,60.9543804525568));
#31738=CARTESIAN_POINT('Ctrl Pts',(75.1818659698106,361.288973947616,61.2464519739654));
#31739=CARTESIAN_POINT('Ctrl Pts',(77.2912945088671,361.466070519615,60.6057014773953));
#31740=CARTESIAN_POINT('Ctrl Pts',(79.4007230479237,361.643167091614,59.9649509808253));
#31741=CARTESIAN_POINT('Ctrl Pts',(81.211827594208,361.820263663612,58.4014001198771));
#31742=CARTESIAN_POINT('Ctrl Pts',(82.1535440633102,361.997360235611,56.4080561826543));
#31743=CARTESIAN_POINT('Ctrl Pts',(82.6515697929911,362.091017564953,55.3538784110932));
#31744=CARTESIAN_POINT('Ctrl Pts',(82.9129498948689,362.184674894296,54.1887099277327));
#31745=CARTESIAN_POINT('Ctrl Pts',(82.9129498948689,362.278332223638,53.0228109606358));
#31746=CARTESIAN_POINT('Ctrl Pts',(82.9208104299352,363.721667776361,53.0177222740361));
#31747=CARTESIAN_POINT('Ctrl Pts',(82.9006493036487,363.538829724732,55.2853910421037));
#31748=CARTESIAN_POINT('Ctrl Pts',(81.8727588800135,363.355991673103,57.5656941132477));
#31749=CARTESIAN_POINT('Ctrl Pts',(80.1547284126926,363.173153621474,59.0453531318087));
#31750=CARTESIAN_POINT('Ctrl Pts',(79.1579706672753,363.067075616698,59.9038138025483));
#31751=CARTESIAN_POINT('Ctrl Pts',(77.9289099623936,362.960997611922,60.4927755728916));
#31752=CARTESIAN_POINT('Ctrl Pts',(76.6332069362866,362.854919607146,60.7680123822706));
#31753=CARTESIAN_POINT('Ctrl Pts',(75.3375039101796,362.748841602369,61.0432491916497));
#31754=CARTESIAN_POINT('Ctrl Pts',(73.9751585628473,362.642763597593,61.0047610400644));
#31755=CARTESIAN_POINT('Ctrl Pts',(72.7155046793147,362.536685592817,60.6256135490307));
#31756=CARTESIAN_POINT('Ctrl Pts',(70.1961969122495,362.324529583265,59.8673185669634));
#31757=CARTESIAN_POINT('Ctrl Pts',(68.0876550003827,362.112373573713,57.7463862271029));
#31758=CARTESIAN_POINT('Ctrl Pts',(67.3597044157122,361.90021756416,55.2219954732745));
#31759=CARTESIAN_POINT('Ctrl Pts',(66.6317538310416,361.688061554608,52.697604719446));
#31760=CARTESIAN_POINT('Ctrl Pts',(67.2843945735672,361.475905545056,49.7697555516497));
#31761=CARTESIAN_POINT('Ctrl Pts',(69.0165499320151,361.263749535503,47.7914832427962));
#31762=CARTESIAN_POINT('Ctrl Pts',(70.748705290463,361.051593525951,45.8132109339427));
#31763=CARTESIAN_POINT('Ctrl Pts',(73.5603752648332,360.839437516399,44.7845154840321));
#31764=CARTESIAN_POINT('Ctrl Pts',(76.1604012109173,360.627281506846,45.1728490688669));
#31765=CARTESIAN_POINT('Ctrl Pts',(78.7604271570015,360.415125497294,45.5611826537016));
#31766=CARTESIAN_POINT('Ctrl Pts',(81.1488090747995,360.202969487742,47.3665452732815));
#31767=CARTESIAN_POINT('Ctrl Pts',(82.22732492823,359.99081347819,49.7646126342361));
#31768=CARTESIAN_POINT('Ctrl Pts',(82.6834011068206,359.901098244247,50.7786926725667));
#31769=CARTESIAN_POINT('Ctrl Pts',(82.9052440041322,359.811383010304,51.8987615445487));
#31770=CARTESIAN_POINT('Ctrl Pts',(82.9009763088175,359.721667776361,53.0203164204654));
#31771=CARTESIAN_POINT('Origin',(74.9879498948689,255.,53.0228109606356));
#31772=CARTESIAN_POINT('',(82.9154091900529,354.278332223638,53.0231896391828));
#31773=CARTESIAN_POINT('',(82.9122147864747,355.721667776361,53.0240094724492));
#31774=CARTESIAN_POINT('',(82.9129498948689,255.,53.0228109606356));
#31775=CARTESIAN_POINT('Ctrl Pts',(82.9228124950414,354.278332223638,53.0243295888637));
#31776=CARTESIAN_POINT('Ctrl Pts',(82.9198720468438,354.370785911918,51.8773028605082));
#31777=CARTESIAN_POINT('Ctrl Pts',(82.6535218078163,354.463239600199,50.7278473767095));
#31778=CARTESIAN_POINT('Ctrl Pts',(82.1663005056112,354.55569328848,49.6812098020159));
#31779=CARTESIAN_POINT('Ctrl Pts',(81.6072804753287,354.661771293256,48.4803358540751));
#31780=CARTESIAN_POINT('Ctrl Pts',(80.757496184371,354.767849298032,47.4148158673777));
#31781=CARTESIAN_POINT('Ctrl Pts',(79.6972259522975,354.873927302808,46.6361582011118));
#31782=CARTESIAN_POINT('Ctrl Pts',(77.5766854881505,355.086083312361,45.0788428685798));
#31783=CARTESIAN_POINT('Ctrl Pts',(74.6142012595406,355.298239321913,44.6689768177737));
#31784=CARTESIAN_POINT('Ctrl Pts',(72.1593083598743,355.510395331465,45.6049050110154));
#31785=CARTESIAN_POINT('Ctrl Pts',(69.7044154602081,355.722551341017,46.5408332042571));
#31786=CARTESIAN_POINT('Ctrl Pts',(67.7571138894853,355.93470735057,48.8225556415467));
#31787=CARTESIAN_POINT('Ctrl Pts',(67.2176183240624,356.146863360122,51.3960489966313));
#31788=CARTESIAN_POINT('Ctrl Pts',(66.6781227586394,356.359019369674,53.969542351716));
#31789=CARTESIAN_POINT('Ctrl Pts',(67.5464331985163,356.571175379227,56.8348066245959));
#31790=CARTESIAN_POINT('Ctrl Pts',(69.4198621488847,356.783331388779,58.6790413876732));
#31791=CARTESIAN_POINT('Ctrl Pts',(71.2932910992532,356.995487398331,60.5232761507505));
#31792=CARTESIAN_POINT('Ctrl Pts',(74.1718385601131,357.207643407883,61.3464814040251));
#31793=CARTESIAN_POINT('Ctrl Pts',(76.7365419224931,357.419799417436,60.7666364447703));
#31794=CARTESIAN_POINT('Ctrl Pts',(79.301245284873,357.631955426988,60.1867914855154));
#31795=CARTESIAN_POINT('Ctrl Pts',(81.5521045487729,357.844111436541,58.2038963137311));
#31796=CARTESIAN_POINT('Ctrl Pts',(82.4493639735543,358.056267446093,55.7346077003086));
#31797=CARTESIAN_POINT('Ctrl Pts',(82.7624193126962,358.130289038608,54.8730687039335));
#31798=CARTESIAN_POINT('Ctrl Pts',(82.9106976993204,358.204310631123,53.9523198681941));
#31799=CARTESIAN_POINT('Ctrl Pts',(82.9035224954183,358.278332223638,53.029540142668));
#31800=CARTESIAN_POINT('Ctrl Pts',(82.9129498948689,359.721667776361,53.0228109606489));
#31801=CARTESIAN_POINT('Ctrl Pts',(82.9129498948652,359.544571204362,55.2274084205588));
#31802=CARTESIAN_POINT('Ctrl Pts',(81.9432795991032,359.367474632363,57.4147653849934));
#31803=CARTESIAN_POINT('Ctrl Pts',(80.3096882702443,359.190378060364,58.8951806411016));
#31804=CARTESIAN_POINT('Ctrl Pts',(78.6760969413853,359.013281488366,60.3755958972098));
#31805=CARTESIAN_POINT('Ctrl Pts',(76.4041347530307,358.836184916367,61.1259150206705));
#31806=CARTESIAN_POINT('Ctrl Pts',(74.2101800112085,358.659088344368,60.9095529374008));
#31807=CARTESIAN_POINT('Ctrl Pts',(72.0162252693863,358.481991772369,60.6931908541311));
#31808=CARTESIAN_POINT('Ctrl Pts',(69.9345925076867,358.304895200371,59.5135315737611));
#31809=CARTESIAN_POINT('Ctrl Pts',(68.6216467656526,358.127798628372,57.7425365317817));
#31810=CARTESIAN_POINT('Ctrl Pts',(67.3087010236185,357.950702056373,55.9715414898024));
#31811=CARTESIAN_POINT('Ctrl Pts',(66.7849774198228,357.773605484375,53.6369099216163));
#31812=CARTESIAN_POINT('Ctrl Pts',(67.2156126057632,357.596508912376,51.4747805783828));
#31813=CARTESIAN_POINT('Ctrl Pts',(67.6462477917036,357.419412340377,49.3126512351494));
#31814=CARTESIAN_POINT('Ctrl Pts',(69.0245064208065,357.242315768378,47.3568408855378));
#31815=CARTESIAN_POINT('Ctrl Pts',(70.9158061804583,357.06521919638,46.2240411771243));
#31816=CARTESIAN_POINT('Ctrl Pts',(72.8071059401102,356.888122624381,45.0912414687107));
#31817=CARTESIAN_POINT('Ctrl Pts',(75.1818659698244,356.711026052382,44.7991699473061));
#31818=CARTESIAN_POINT('Ctrl Pts',(77.2912945088799,356.533929480383,45.4399204438797));
#31819=CARTESIAN_POINT('Ctrl Pts',(79.4007230479353,356.356832908385,46.0806709404532));
#31820=CARTESIAN_POINT('Ctrl Pts',(81.2118275942171,356.179736336386,47.6442218014045));
#31821=CARTESIAN_POINT('Ctrl Pts',(82.1535440633159,356.002639764387,49.6375657386289));
#31822=CARTESIAN_POINT('Ctrl Pts',(82.6515697929952,355.908982435045,50.6917435101911));
#31823=CARTESIAN_POINT('Ctrl Pts',(82.912949894871,355.815325105703,51.8569119935523));
#31824=CARTESIAN_POINT('Ctrl Pts',(82.9129498948689,355.721667776361,53.0228109606495));
#31825=CARTESIAN_POINT('Origin',(74.9879498948689,255.,53.0228109606356));
#31826=CARTESIAN_POINT('',(82.9131455474441,350.278332223638,53.0224568952625));
#31827=CARTESIAN_POINT('',(82.9249635206133,351.72166777636,53.0231874323186));
#31828=CARTESIAN_POINT('',(82.9129498948689,255.,53.0228109606356));
#31829=CARTESIAN_POINT('Ctrl Pts',(82.9129498948689,350.278332223638,53.0228109606361));
#31830=CARTESIAN_POINT('Ctrl Pts',(82.912949894869,350.455428795636,50.8182135007263));
#31831=CARTESIAN_POINT('Ctrl Pts',(81.943279599111,350.632525367635,48.63085653629));
#31832=CARTESIAN_POINT('Ctrl Pts',(80.3096882702547,350.809621939634,47.150441280179));
#31833=CARTESIAN_POINT('Ctrl Pts',(78.6760969413985,350.986718511633,45.6700260240679));
#31834=CARTESIAN_POINT('Ctrl Pts',(76.4041347530453,351.163815083631,44.9197069006032));
#31835=CARTESIAN_POINT('Ctrl Pts',(74.2101800112228,351.34091165563,45.1360689838689));
#31836=CARTESIAN_POINT('Ctrl Pts',(72.0162252694002,351.518008227629,45.3524310671346));
#31837=CARTESIAN_POINT('Ctrl Pts',(69.9345925076986,351.695104799628,46.5320903475008));
#31838=CARTESIAN_POINT('Ctrl Pts',(68.6216467656613,351.872201371626,48.3030853894777));
#31839=CARTESIAN_POINT('Ctrl Pts',(67.308701023624,352.049297943625,50.0740804314546));
#31840=CARTESIAN_POINT('Ctrl Pts',(66.784977419824,352.226394515624,52.4087119996397));
#31841=CARTESIAN_POINT('Ctrl Pts',(67.2156126057604,352.403491087622,54.5708413428738));
#31842=CARTESIAN_POINT('Ctrl Pts',(67.6462477916967,352.580587659621,56.732970686108));
#31843=CARTESIAN_POINT('Ctrl Pts',(69.0245064207958,352.75768423162,58.688781035722));
#31844=CARTESIAN_POINT('Ctrl Pts',(70.9158061804454,352.934780803619,59.8215807441392));
#31845=CARTESIAN_POINT('Ctrl Pts',(72.8071059400951,353.111877375617,60.9543804525563));
#31846=CARTESIAN_POINT('Ctrl Pts',(75.1818659698087,353.288973947616,61.2464519739654));
#31847=CARTESIAN_POINT('Ctrl Pts',(77.2912945088653,353.466070519615,60.6057014773959));
#31848=CARTESIAN_POINT('Ctrl Pts',(79.4007230479219,353.643167091614,59.9649509808264));
#31849=CARTESIAN_POINT('Ctrl Pts',(81.2118275942066,353.820263663612,58.4014001198787));
#31850=CARTESIAN_POINT('Ctrl Pts',(82.1535440633093,353.997360235611,56.4080561826562));
#31851=CARTESIAN_POINT('Ctrl Pts',(82.6515697929907,354.091017564953,55.3538784110948));
#31852=CARTESIAN_POINT('Ctrl Pts',(82.9129498948688,354.184674894296,54.1887099277338));
#31853=CARTESIAN_POINT('Ctrl Pts',(82.9129498948689,354.278332223638,53.0228109606363));
#31854=CARTESIAN_POINT('Ctrl Pts',(82.9091135838053,355.721667776361,53.0290656354458));
#31855=CARTESIAN_POINT('Ctrl Pts',(82.9157961825277,355.659624276771,53.8021586410643));
#31856=CARTESIAN_POINT('Ctrl Pts',(82.8118813088041,355.597580777181,54.5736419934824));
#31857=CARTESIAN_POINT('Ctrl Pts',(82.5901503636487,355.535537277591,55.3099391250131));
#31858=CARTESIAN_POINT('Ctrl Pts',(81.8319476054334,355.323381268038,57.8276865490433));
#31859=CARTESIAN_POINT('Ctrl Pts',(79.6961464125835,355.111225258486,59.9340089253166));
#31860=CARTESIAN_POINT('Ctrl Pts',(77.1700348613008,354.899069248934,60.6559654075322));
#31861=CARTESIAN_POINT('Ctrl Pts',(74.6439233100181,354.686913239382,61.3779218897477));
#31862=CARTESIAN_POINT('Ctrl Pts',(71.7275014003028,354.474757229829,60.7155124779055));
#31863=CARTESIAN_POINT('Ctrl Pts',(69.7483232334138,354.262601220277,58.9820833075226));
#31864=CARTESIAN_POINT('Ctrl Pts',(68.7587341499693,354.156523215501,58.1153687223312));
#31865=CARTESIAN_POINT('Ctrl Pts',(68.0034560022314,354.050445210725,56.9808991975047));
#31866=CARTESIAN_POINT('Ctrl Pts',(67.5494784950457,353.944367205949,55.7365093646672));
#31867=CARTESIAN_POINT('Ctrl Pts',(67.0955009878599,353.838289201172,54.4921195318297));
#31868=CARTESIAN_POINT('Ctrl Pts',(66.9428241212262,353.732211196396,53.1378093909812));
#31869=CARTESIAN_POINT('Ctrl Pts',(67.1418307132696,353.62613319162,51.8374720875944));
#31870=CARTESIAN_POINT('Ctrl Pts',(67.5398438973563,353.413977182067,49.2367974808209));
#31871=CARTESIAN_POINT('Ctrl Pts',(69.3445909161509,353.201821172515,46.8520142238943));
#31872=CARTESIAN_POINT('Ctrl Pts',(71.7421614310037,352.989665162963,45.7777161469878));
#31873=CARTESIAN_POINT('Ctrl Pts',(74.1397319458566,352.777509153411,44.7034180700812));
#31874=CARTESIAN_POINT('Ctrl Pts',(77.1301259567676,352.565353143858,44.9396051731948));
#31875=CARTESIAN_POINT('Ctrl Pts',(79.3314781915037,352.353197134306,46.3776496274446));
#31876=CARTESIAN_POINT('Ctrl Pts',(81.5157490438013,352.142687348324,47.8045355824324));
#31877=CARTESIAN_POINT('Ctrl Pts',(82.9231757438946,351.932177562342,50.4146996390436));
#31878=CARTESIAN_POINT('Ctrl Pts',(82.9249635206133,351.72166777636,53.0231874323186));
#31879=CARTESIAN_POINT('Origin',(74.9879498948689,255.,53.0228109606356));
#31880=CARTESIAN_POINT('',(82.9073270357724,346.278332223638,53.0223005851992));
#31881=CARTESIAN_POINT('',(82.9121137244291,347.721667776361,53.0207950825717));
#31882=CARTESIAN_POINT('',(82.9129498948689,255.,53.0228109606356));
#31883=CARTESIAN_POINT('Ctrl Pts',(82.8972748771451,346.278332223638,53.0213881712888));
#31884=CARTESIAN_POINT('Ctrl Pts',(82.8983129557911,346.385502459181,51.6828751929879));
#31885=CARTESIAN_POINT('Ctrl Pts',(82.5784150468752,346.492672694724,50.3448798377769));
#31886=CARTESIAN_POINT('Ctrl Pts',(81.9366274606094,346.599842930268,49.1832248243079));
#31887=CARTESIAN_POINT('Ctrl Pts',(80.6661339080663,346.81199893982,46.8835929266593));
#31888=CARTESIAN_POINT('Ctrl Pts',(78.1341923471884,347.024154949372,45.275018209567));
#31889=CARTESIAN_POINT('Ctrl Pts',(75.5105072571905,347.236310958925,45.1012365583537));
#31890=CARTESIAN_POINT('Ctrl Pts',(72.8868221671925,347.448466968477,44.9274549071403));
#31891=CARTESIAN_POINT('Ctrl Pts',(70.1713935480745,347.660622978029,46.1884663218059));
#31892=CARTESIAN_POINT('Ctrl Pts',(68.6076916836926,347.872778987582,48.301704210154));
#31893=CARTESIAN_POINT('Ctrl Pts',(67.0439898193109,348.084934997134,50.4149420985021));
#31894=CARTESIAN_POINT('Ctrl Pts',(66.6320147096651,348.297091006686,53.3804064605326));
#31895=CARTESIAN_POINT('Ctrl Pts',(67.5653121245716,348.509247016239,55.8386333518315));
#31896=CARTESIAN_POINT('Ctrl Pts',(68.4986095394781,348.721403025791,58.2968602431304));
#31897=CARTESIAN_POINT('Ctrl Pts',(70.7771794789368,348.933559035343,60.2478496636975));
#31898=CARTESIAN_POINT('Ctrl Pts',(73.3477887194659,349.145715044896,60.7904626604485));
#31899=CARTESIAN_POINT('Ctrl Pts',(75.918397959995,349.357871054448,61.3330756571995));
#31900=CARTESIAN_POINT('Ctrl Pts',(78.7810465015946,349.570027064,60.4673122301343));
#31901=CARTESIAN_POINT('Ctrl Pts',(80.633488508501,349.782183073552,58.5990559532621));
#31902=CARTESIAN_POINT('Ctrl Pts',(81.5597095119541,349.888261078329,57.664927814826));
#31903=CARTESIAN_POINT('Ctrl Pts',(82.233378881734,349.994339083105,56.4801764639381));
#31904=CARTESIAN_POINT('Ctrl Pts',(82.5987666386957,350.100417087881,55.2069547942504));
#31905=CARTESIAN_POINT('Ctrl Pts',(82.8030440240684,350.159722133134,54.4951345738729));
#31906=CARTESIAN_POINT('Ctrl Pts',(82.9109650860172,350.219027178386,53.755662121584));
#31907=CARTESIAN_POINT('Ctrl Pts',(82.9157605881844,350.278332223638,53.0177245508215));
#31908=CARTESIAN_POINT('Ctrl Pts',(82.9249635206133,351.72166777636,53.0231874323186));
#31909=CARTESIAN_POINT('Ctrl Pts',(82.9249775013419,351.72002155279,53.0435862658865));
#31910=CARTESIAN_POINT('Ctrl Pts',(82.924905520008,351.718375329219,53.0639849969422));
#31911=CARTESIAN_POINT('Ctrl Pts',(82.9247472758945,351.716729105649,53.0843830587884));
#31912=CARTESIAN_POINT('Ctrl Pts',(82.9043536669879,351.504573096097,55.7131702304965));
#31913=CARTESIAN_POINT('Ctrl Pts',(81.4512559906136,351.292417086545,58.3308427685267));
#31914=CARTESIAN_POINT('Ctrl Pts',(79.2278579260863,351.080261076992,59.7345608885324));
#31915=CARTESIAN_POINT('Ctrl Pts',(77.004459861559,350.86810506744,61.1382790085381));
#31916=CARTESIAN_POINT('Ctrl Pts',(74.0107614088787,350.655949057887,61.3280427105194));
#31917=CARTESIAN_POINT('Ctrl Pts',(71.6301468441837,350.443793048335,60.2166764225214));
#31918=CARTESIAN_POINT('Ctrl Pts',(69.2495322794886,350.231637038783,59.1053101345234));
#31919=CARTESIAN_POINT('Ctrl Pts',(67.4820016027788,350.019481029231,56.6928138565462));
#31920=CARTESIAN_POINT('Ctrl Pts',(67.1243849295486,349.807325019679,54.0862772233772));
#31921=CARTESIAN_POINT('Ctrl Pts',(66.9455765929335,349.701247014902,52.7830089067927));
#31922=CARTESIAN_POINT('Ctrl Pts',(67.1192467571882,349.595169010126,51.4312305014103));
#31923=CARTESIAN_POINT('Ctrl Pts',(67.5924759203216,349.48909100535,50.1940337538151));
#31924=CARTESIAN_POINT('Ctrl Pts',(68.065705083455,349.383013000574,48.95683700622));
#31925=CARTESIAN_POINT('Ctrl Pts',(68.8384932454669,349.276934995797,47.8342219164121));
#31926=CARTESIAN_POINT('Ctrl Pts',(69.8414100122834,349.170856991021,46.9829647959755));
#31927=CARTESIAN_POINT('Ctrl Pts',(71.8472435459166,348.958700981469,45.2804505551021));
#31928=CARTESIAN_POINT('Ctrl Pts',(74.7735914987686,348.746544971917,44.663368191714));
#31929=CARTESIAN_POINT('Ctrl Pts',(77.2881980920006,348.534388962364,45.4244295644106));
#31930=CARTESIAN_POINT('Ctrl Pts',(79.8028046852326,348.322232952812,46.1854909371071));
#31931=CARTESIAN_POINT('Ctrl Pts',(81.9056699188448,348.11007694326,48.3246960458882));
#31932=CARTESIAN_POINT('Ctrl Pts',(82.6247194016904,347.897920933707,50.8539036994817));
#31933=CARTESIAN_POINT('Ctrl Pts',(82.823841330733,347.839169881258,51.5543015426731));
#31934=CARTESIAN_POINT('Ctrl Pts',(82.9168428557268,347.78041882881,52.2846074336755));
#31935=CARTESIAN_POINT('Ctrl Pts',(82.910294861139,347.721667776361,53.0164100834644));
#31936=CARTESIAN_POINT('Origin',(74.9879498948689,255.,53.0228109606356));
#31937=CARTESIAN_POINT('',(82.9129498948689,342.278332223638,53.0228109606362));
#31938=CARTESIAN_POINT('',(82.9129498948689,343.721667776361,53.0228109606494));
#31939=CARTESIAN_POINT('',(82.9129498948689,255.,53.0228109606356));
#31940=CARTESIAN_POINT('Ctrl Pts',(82.9129498948689,342.278332223638,53.0228109606367));
#31941=CARTESIAN_POINT('Ctrl Pts',(82.9129498948692,342.455428795636,50.8182135007268));
#31942=CARTESIAN_POINT('Ctrl Pts',(81.9432795991113,342.632525367635,48.6308565362905));
#31943=CARTESIAN_POINT('Ctrl Pts',(80.3096882702551,342.809621939634,47.1504412801793));
#31944=CARTESIAN_POINT('Ctrl Pts',(78.6760969413989,342.986718511633,45.6700260240681));
#31945=CARTESIAN_POINT('Ctrl Pts',(76.4041347530457,343.163815083631,44.9197069006033));
#31946=CARTESIAN_POINT('Ctrl Pts',(74.2101800112231,343.34091165563,45.1360689838689));
#31947=CARTESIAN_POINT('Ctrl Pts',(72.0162252694005,343.518008227629,45.3524310671345));
#31948=CARTESIAN_POINT('Ctrl Pts',(69.9345925076989,343.695104799628,46.5320903475007));
#31949=CARTESIAN_POINT('Ctrl Pts',(68.6216467656614,343.872201371626,48.3030853894775));
#31950=CARTESIAN_POINT('Ctrl Pts',(67.308701023624,344.049297943625,50.0740804314544));
#31951=CARTESIAN_POINT('Ctrl Pts',(66.784977419824,344.226394515624,52.4087119996395));
#31952=CARTESIAN_POINT('Ctrl Pts',(67.2156126057603,344.403491087622,54.5708413428737));
#31953=CARTESIAN_POINT('Ctrl Pts',(67.6462477916967,344.580587659621,56.7329706861079));
#31954=CARTESIAN_POINT('Ctrl Pts',(69.0245064207958,344.75768423162,58.688781035722));
#31955=CARTESIAN_POINT('Ctrl Pts',(70.9158061804454,344.934780803619,59.8215807441392));
#31956=CARTESIAN_POINT('Ctrl Pts',(72.8071059400951,345.111877375617,60.9543804525563));
#31957=CARTESIAN_POINT('Ctrl Pts',(75.1818659698087,345.288973947616,61.2464519739654));
#31958=CARTESIAN_POINT('Ctrl Pts',(77.2912945088654,345.466070519615,60.6057014773959));
#31959=CARTESIAN_POINT('Ctrl Pts',(79.4007230479221,345.643167091614,59.9649509808263));
#31960=CARTESIAN_POINT('Ctrl Pts',(81.2118275942068,345.820263663612,58.4014001198785));
#31961=CARTESIAN_POINT('Ctrl Pts',(82.1535440633093,345.997360235611,56.408056182656));
#31962=CARTESIAN_POINT('Ctrl Pts',(82.6515697929908,346.091017564953,55.3538784110945));
#31963=CARTESIAN_POINT('Ctrl Pts',(82.9129498948689,346.184674894296,54.1887099277335));
#31964=CARTESIAN_POINT('Ctrl Pts',(82.9129498948689,346.278332223638,53.0228109606359));
#31965=CARTESIAN_POINT('Ctrl Pts',(82.9129498948689,347.721667776361,53.0228109606492));
#31966=CARTESIAN_POINT('Ctrl Pts',(82.9129498948651,347.544571204362,55.227408420559));
#31967=CARTESIAN_POINT('Ctrl Pts',(81.9432795991031,347.367474632363,57.4147653849935));
#31968=CARTESIAN_POINT('Ctrl Pts',(80.3096882702442,347.190378060364,58.8951806411017));
#31969=CARTESIAN_POINT('Ctrl Pts',(78.6760969413853,347.013281488366,60.3755958972098));
#31970=CARTESIAN_POINT('Ctrl Pts',(76.4041347530308,346.836184916367,61.1259150206704));
#31971=CARTESIAN_POINT('Ctrl Pts',(74.2101800112087,346.659088344368,60.9095529374008));
#31972=CARTESIAN_POINT('Ctrl Pts',(72.0162252693865,346.481991772369,60.6931908541312));
#31973=CARTESIAN_POINT('Ctrl Pts',(69.934592507687,346.304895200371,59.5135315737613));
#31974=CARTESIAN_POINT('Ctrl Pts',(68.6216467656529,346.127798628372,57.7425365317821));
#31975=CARTESIAN_POINT('Ctrl Pts',(67.3087010236187,345.950702056373,55.9715414898028));
#31976=CARTESIAN_POINT('Ctrl Pts',(66.7849774198229,345.773605484375,53.6369099216168));
#31977=CARTESIAN_POINT('Ctrl Pts',(67.2156126057631,345.596508912376,51.4747805783834));
#31978=CARTESIAN_POINT('Ctrl Pts',(67.6462477917033,345.419412340377,49.31265123515));
#31979=CARTESIAN_POINT('Ctrl Pts',(69.0245064208059,345.242315768378,47.3568408855384));
#31980=CARTESIAN_POINT('Ctrl Pts',(70.9158061804576,345.06521919638,46.2240411771247));
#31981=CARTESIAN_POINT('Ctrl Pts',(72.8071059401093,344.888122624381,45.091241468711));
#31982=CARTESIAN_POINT('Ctrl Pts',(75.1818659698233,344.711026052382,44.7991699473061));
#31983=CARTESIAN_POINT('Ctrl Pts',(77.2912945088788,344.533929480384,45.4399204438793));
#31984=CARTESIAN_POINT('Ctrl Pts',(79.4007230479343,344.356832908385,46.0806709404526));
#31985=CARTESIAN_POINT('Ctrl Pts',(81.2118275942162,344.179736336386,47.6442218014036));
#31986=CARTESIAN_POINT('Ctrl Pts',(82.1535440633153,344.002639764387,49.6375657386277));
#31987=CARTESIAN_POINT('Ctrl Pts',(82.6515697929949,343.908982435045,50.69174351019));
#31988=CARTESIAN_POINT('Ctrl Pts',(82.9129498948709,343.815325105703,51.8569119935515));
#31989=CARTESIAN_POINT('Ctrl Pts',(82.9129498948689,343.721667776361,53.022810960649));
#31990=CARTESIAN_POINT('Origin',(74.9879498948689,255.,53.0228109606356));
#31991=CARTESIAN_POINT('',(82.9170870675938,338.278332223638,53.0212355344904));
#31992=CARTESIAN_POINT('',(82.9129498948689,339.721667776361,53.0228109606494));
#31993=CARTESIAN_POINT('',(82.9129498948689,255.,53.0228109606356));
#31994=CARTESIAN_POINT('Ctrl Pts',(82.9129498948689,338.278332223638,53.0228109606365));
#31995=CARTESIAN_POINT('Ctrl Pts',(82.9129498948692,338.455428795636,50.8182135007266));
#31996=CARTESIAN_POINT('Ctrl Pts',(81.9432795991111,338.632525367635,48.6308565362901));
#31997=CARTESIAN_POINT('Ctrl Pts',(80.3096882702548,338.809621939634,47.150441280179));
#31998=CARTESIAN_POINT('Ctrl Pts',(78.6760969413984,338.986718511633,45.6700260240679));
#31999=CARTESIAN_POINT('Ctrl Pts',(76.4041347530451,339.163815083631,44.9197069006032));
#32000=CARTESIAN_POINT('Ctrl Pts',(74.2101800112225,339.34091165563,45.136068983869));
#32001=CARTESIAN_POINT('Ctrl Pts',(72.0162252693998,339.518008227629,45.3524310671347));
#32002=CARTESIAN_POINT('Ctrl Pts',(69.9345925076982,339.695104799628,46.5320903475011));
#32003=CARTESIAN_POINT('Ctrl Pts',(68.6216467656609,339.872201371626,48.3030853894782));
#32004=CARTESIAN_POINT('Ctrl Pts',(67.3087010236237,340.049297943625,50.0740804314553));
#32005=CARTESIAN_POINT('Ctrl Pts',(66.7849774198239,340.226394515624,52.4087119996405));
#32006=CARTESIAN_POINT('Ctrl Pts',(67.2156126057605,340.403491087623,54.5708413428748));
#32007=CARTESIAN_POINT('Ctrl Pts',(67.6462477916972,340.580587659621,56.732970686109));
#32008=CARTESIAN_POINT('Ctrl Pts',(69.0245064207966,340.75768423162,58.688781035723));
#32009=CARTESIAN_POINT('Ctrl Pts',(70.9158061804466,340.934780803619,59.8215807441398));
#32010=CARTESIAN_POINT('Ctrl Pts',(72.8071059400965,341.111877375617,60.9543804525567));
#32011=CARTESIAN_POINT('Ctrl Pts',(75.1818659698102,341.288973947616,61.2464519739654));
#32012=CARTESIAN_POINT('Ctrl Pts',(77.2912945088669,341.466070519615,60.6057014773954));
#32013=CARTESIAN_POINT('Ctrl Pts',(79.4007230479235,341.643167091614,59.9649509808254));
#32014=CARTESIAN_POINT('Ctrl Pts',(81.2118275942079,341.820263663612,58.4014001198772));
#32015=CARTESIAN_POINT('Ctrl Pts',(82.1535440633101,341.997360235611,56.4080561826544));
#32016=CARTESIAN_POINT('Ctrl Pts',(82.6515697929909,342.091017564953,55.3538784110936));
#32017=CARTESIAN_POINT('Ctrl Pts',(82.9129498948687,342.184674894296,54.1887099277334));
#32018=CARTESIAN_POINT('Ctrl Pts',(82.9129498948689,342.278332223638,53.0228109606367));
#32019=CARTESIAN_POINT('Ctrl Pts',(82.9129498948689,343.721667776361,53.022810960649));
#32020=CARTESIAN_POINT('Ctrl Pts',(82.9129498948652,343.544571204362,55.2274084205589));
#32021=CARTESIAN_POINT('Ctrl Pts',(81.9432795991032,343.367474632363,57.4147653849935));
#32022=CARTESIAN_POINT('Ctrl Pts',(80.3096882702443,343.190378060364,58.8951806411016));
#32023=CARTESIAN_POINT('Ctrl Pts',(78.6760969413854,343.013281488366,60.3755958972098));
#32024=CARTESIAN_POINT('Ctrl Pts',(76.4041347530308,342.836184916367,61.1259150206705));
#32025=CARTESIAN_POINT('Ctrl Pts',(74.2101800112086,342.659088344368,60.9095529374008));
#32026=CARTESIAN_POINT('Ctrl Pts',(72.0162252693864,342.481991772369,60.6931908541312));
#32027=CARTESIAN_POINT('Ctrl Pts',(69.9345925076869,342.304895200371,59.5135315737612));
#32028=CARTESIAN_POINT('Ctrl Pts',(68.6216467656528,342.127798628372,57.7425365317819));
#32029=CARTESIAN_POINT('Ctrl Pts',(67.3087010236186,341.950702056373,55.9715414898026));
#32030=CARTESIAN_POINT('Ctrl Pts',(66.7849774198229,341.773605484375,53.6369099216166));
#32031=CARTESIAN_POINT('Ctrl Pts',(67.2156126057632,341.596508912376,51.4747805783831));
#32032=CARTESIAN_POINT('Ctrl Pts',(67.6462477917035,341.419412340377,49.3126512351497));
#32033=CARTESIAN_POINT('Ctrl Pts',(69.0245064208062,341.242315768378,47.3568408855382));
#32034=CARTESIAN_POINT('Ctrl Pts',(70.9158061804579,341.06521919638,46.2240411771245));
#32035=CARTESIAN_POINT('Ctrl Pts',(72.8071059401097,340.888122624381,45.0912414687108));
#32036=CARTESIAN_POINT('Ctrl Pts',(75.1818659698238,340.711026052382,44.7991699473061));
#32037=CARTESIAN_POINT('Ctrl Pts',(77.2912945088793,340.533929480383,45.4399204438795));
#32038=CARTESIAN_POINT('Ctrl Pts',(79.4007230479348,340.356832908385,46.0806709404529));
#32039=CARTESIAN_POINT('Ctrl Pts',(81.2118275942166,340.179736336386,47.644221801404));
#32040=CARTESIAN_POINT('Ctrl Pts',(82.1535440633156,340.002639764387,49.6375657386283));
#32041=CARTESIAN_POINT('Ctrl Pts',(82.6515697929949,339.908982435045,50.6917435101904));
#32042=CARTESIAN_POINT('Ctrl Pts',(82.9129498948709,339.815325105703,51.8569119935516));
#32043=CARTESIAN_POINT('Ctrl Pts',(82.9129498948689,339.721667776361,53.0228109606489));
#32044=CARTESIAN_POINT('Origin',(74.9879498948689,255.,53.0228109606356));
#32045=CARTESIAN_POINT('',(82.9037265626259,334.278332223638,53.0173862307939));
#32046=CARTESIAN_POINT('',(82.913275875755,335.721667776361,53.0223309921515));
#32047=CARTESIAN_POINT('',(82.9129498948689,255.,53.0228109606356));
#32048=CARTESIAN_POINT('Ctrl Pts',(82.9037265626259,334.278332223638,53.0173862307939));
#32049=CARTESIAN_POINT('Ctrl Pts',(82.909334688827,334.354538277687,52.0664523593613));
#32050=CARTESIAN_POINT('Ctrl Pts',(82.7505377378628,334.430744331736,51.1174380195998));
#32051=CARTESIAN_POINT('Ctrl Pts',(82.4186752153905,334.506950385786,50.2333907696849));
#32052=CARTESIAN_POINT('Ctrl Pts',(81.494777116139,334.719106395338,47.7722223082382));
#32053=CARTESIAN_POINT('Ctrl Pts',(79.2295281067083,334.931262404891,45.8145836033915));
#32054=CARTESIAN_POINT('Ctrl Pts',(76.6588454982678,335.143418414443,45.2618499962738));
#32055=CARTESIAN_POINT('Ctrl Pts',(74.0881628898271,335.355574423995,44.7091163891561));
#32056=CARTESIAN_POINT('Ctrl Pts',(71.2120466823766,335.567730433547,45.5612878797677));
#32057=CARTESIAN_POINT('Ctrl Pts',(69.3593696430875,335.7798864431,47.4240945041463));
#32058=CARTESIAN_POINT('Ctrl Pts',(67.5066926037986,335.992042452652,49.2869011285248));
#32059=CARTESIAN_POINT('Ctrl Pts',(66.6774547326711,336.204198462204,52.1603428866702));
#32060=CARTESIAN_POINT('Ctrl Pts',(67.2387782634214,336.416354471757,54.7307200572133));
#32061=CARTESIAN_POINT('Ctrl Pts',(67.5194400287966,336.522432476533,56.0159086424849));
#32062=CARTESIAN_POINT('Ctrl Pts',(68.1477421446412,336.628510481309,57.2253310808559));
#32063=CARTESIAN_POINT('Ctrl Pts',(69.0178667763073,336.734588486085,58.2240726682886));
#32064=CARTESIAN_POINT('Ctrl Pts',(69.8879914079735,336.840666490862,59.2228142557214));
#32065=CARTESIAN_POINT('Ctrl Pts',(70.9999385554612,336.946744495638,60.0108749922159));
#32066=CARTESIAN_POINT('Ctrl Pts',(72.2345617728081,337.052822500414,60.4649523396405));
#32067=CARTESIAN_POINT('Ctrl Pts',(74.7038082075017,337.264978509966,61.3731070344896));
#32068=CARTESIAN_POINT('Ctrl Pts',(77.6637589216318,337.477134519518,60.9453281730592));
#32069=CARTESIAN_POINT('Ctrl Pts',(79.7628065854718,337.689290529071,59.3653093008097));
#32070=CARTESIAN_POINT('Ctrl Pts',(81.7054439799919,337.885637760593,57.9030253335823));
#32071=CARTESIAN_POINT('Ctrl Pts',(82.9106983513784,338.081984992116,55.4538216170673));
#32072=CARTESIAN_POINT('Ctrl Pts',(82.9246711232106,338.278332223638,53.018347543027));
#32073=CARTESIAN_POINT('Ctrl Pts',(82.9129498948689,339.721667776361,53.0228109606489));
#32074=CARTESIAN_POINT('Ctrl Pts',(82.9129498948652,339.544571204362,55.2274084205586));
#32075=CARTESIAN_POINT('Ctrl Pts',(81.9432795991034,339.367474632363,57.4147653849932));
#32076=CARTESIAN_POINT('Ctrl Pts',(80.3096882702446,339.190378060364,58.8951806411014));
#32077=CARTESIAN_POINT('Ctrl Pts',(78.6760969413858,339.013281488366,60.3755958972096));
#32078=CARTESIAN_POINT('Ctrl Pts',(76.4041347530314,338.836184916367,61.1259150206703));
#32079=CARTESIAN_POINT('Ctrl Pts',(74.2101800112092,338.659088344368,60.9095529374009));
#32080=CARTESIAN_POINT('Ctrl Pts',(72.0162252693871,338.48199177237,60.6931908541314));
#32081=CARTESIAN_POINT('Ctrl Pts',(69.9345925076876,338.304895200371,59.5135315737617));
#32082=CARTESIAN_POINT('Ctrl Pts',(68.6216467656533,338.127798628372,57.7425365317826));
#32083=CARTESIAN_POINT('Ctrl Pts',(67.308701023619,337.950702056373,55.9715414898035));
#32084=CARTESIAN_POINT('Ctrl Pts',(66.784977419823,337.773605484375,53.6369099216176));
#32085=CARTESIAN_POINT('Ctrl Pts',(67.215612605763,337.596508912376,51.4747805783842));
#32086=CARTESIAN_POINT('Ctrl Pts',(67.646247791703,337.419412340377,49.3126512351508));
#32087=CARTESIAN_POINT('Ctrl Pts',(69.0245064208053,337.242315768378,47.3568408855391));
#32088=CARTESIAN_POINT('Ctrl Pts',(70.9158061804568,337.06521919638,46.2240411771252));
#32089=CARTESIAN_POINT('Ctrl Pts',(72.8071059401083,336.888122624381,45.0912414687112));
#32090=CARTESIAN_POINT('Ctrl Pts',(75.1818659698223,336.711026052382,44.7991699473061));
#32091=CARTESIAN_POINT('Ctrl Pts',(77.2912945088779,336.533929480384,45.4399204438791));
#32092=CARTESIAN_POINT('Ctrl Pts',(79.4007230479334,336.356832908385,46.080670940452));
#32093=CARTESIAN_POINT('Ctrl Pts',(81.2118275942155,336.179736336386,47.6442218014027));
#32094=CARTESIAN_POINT('Ctrl Pts',(82.1535440633148,336.002639764387,49.6375657386267));
#32095=CARTESIAN_POINT('Ctrl Pts',(82.6515697929948,335.908982435045,50.6917435101894));
#32096=CARTESIAN_POINT('Ctrl Pts',(82.912949894871,335.815325105703,51.8569119935515));
#32097=CARTESIAN_POINT('Ctrl Pts',(82.9129498948689,335.721667776361,53.0228109606495));
#32098=CARTESIAN_POINT('Origin',(74.9879498948689,255.,53.0228109606356));
#32099=CARTESIAN_POINT('',(82.903889038595,330.278332223638,53.0283217876032));
#32100=CARTESIAN_POINT('',(82.9116685845283,331.721667776361,53.0222624917929));
#32101=CARTESIAN_POINT('',(82.9129498948689,255.,53.0228109606356));
#32102=CARTESIAN_POINT('Ctrl Pts',(82.903889038595,330.278332223638,53.0283217876032));
#32103=CARTESIAN_POINT('Ctrl Pts',(82.8936426485269,330.414935553707,51.3238139604592));
#32104=CARTESIAN_POINT('Ctrl Pts',(82.3548623019608,330.551538883775,49.6130285715222));
#32105=CARTESIAN_POINT('Ctrl Pts',(81.3385495151766,330.688142213844,48.2589583526772));
#32106=CARTESIAN_POINT('Ctrl Pts',(79.7601336362042,330.900298223397,46.1559778899091));
#32107=CARTESIAN_POINT('Ctrl Pts',(77.0298808687583,331.112454232949,44.9134158133818));
#32108=CARTESIAN_POINT('Ctrl Pts',(74.4096204600999,331.324610242501,45.1049781336692));
#32109=CARTESIAN_POINT('Ctrl Pts',(71.7893600514415,331.536766252054,45.2965404539567));
#32110=CARTESIAN_POINT('Ctrl Pts',(69.2790920015704,331.748922261606,46.9222271710588));
#32111=CARTESIAN_POINT('Ctrl Pts',(68.0174220572677,331.961078271158,49.230930672305));
#32112=CARTESIAN_POINT('Ctrl Pts',(67.3865870851163,332.067156275934,50.3852824229281));
#32113=CARTESIAN_POINT('Ctrl Pts',(67.0679016393569,332.17323428071,51.7103883695873));
#32114=CARTESIAN_POINT('Ctrl Pts',(67.0699408517118,332.279312285487,53.0350005674449));
#32115=CARTESIAN_POINT('Ctrl Pts',(67.0719800640667,332.385390290263,54.3596127653023));
#32116=CARTESIAN_POINT('Ctrl Pts',(67.3947439345357,332.491468295039,55.6837312143581));
#32117=CARTESIAN_POINT('Ctrl Pts',(68.0291301081419,332.597546299815,56.8361351838901));
#32118=CARTESIAN_POINT('Ctrl Pts',(69.2979024553544,332.809702309367,59.1409431229542));
#32119=CARTESIAN_POINT('Ctrl Pts',(71.8131640151158,333.02185831892,60.7588931439228));
#32120=CARTESIAN_POINT('Ctrl Pts',(74.4340018146482,333.234014328472,60.9423869047961));
#32121=CARTESIAN_POINT('Ctrl Pts',(77.0548396141805,333.446170338024,61.1258806656693));
#32122=CARTESIAN_POINT('Ctrl Pts',(79.7812536534837,333.658326347577,59.8749181664473));
#32123=CARTESIAN_POINT('Ctrl Pts',(81.3531870785991,333.870482357129,57.7670878078129));
#32124=CARTESIAN_POINT('Ctrl Pts',(82.3604848669058,334.006432312632,56.4163862930702));
#32125=CARTESIAN_POINT('Ctrl Pts',(82.8937217865357,334.142382268135,54.7138317313537));
#32126=CARTESIAN_POINT('Ctrl Pts',(82.9037265626259,334.278332223638,53.0173862307939));
#32127=CARTESIAN_POINT('Ctrl Pts',(82.9166114764614,335.721667776361,53.0174197121561));
#32128=CARTESIAN_POINT('Ctrl Pts',(82.8968976708308,335.537298637763,55.3072955719158));
#32129=CARTESIAN_POINT('Ctrl Pts',(81.8585861362189,335.352929499166,57.6087979274022));
#32130=CARTESIAN_POINT('Ctrl Pts',(80.1156668069684,335.168560360569,59.0835915110494));
#32131=CARTESIAN_POINT('Ctrl Pts',(78.1100664517325,334.956404351016,60.7806560197863));
#32132=CARTESIAN_POINT('Ctrl Pts',(75.1714660480381,334.744248341464,61.3830415737116));
#32133=CARTESIAN_POINT('Ctrl Pts',(72.6576542686765,334.532092331911,60.611890582194));
#32134=CARTESIAN_POINT('Ctrl Pts',(70.1438424893148,334.319936322359,59.8407395906763));
#32135=CARTESIAN_POINT('Ctrl Pts',(68.0548193342858,334.107780312807,57.6960520537159));
#32136=CARTESIAN_POINT('Ctrl Pts',(67.3453868006718,333.895624303255,55.164719721984));
#32137=CARTESIAN_POINT('Ctrl Pts',(66.6359542670578,333.683468293703,52.6333873902521));
#32138=CARTESIAN_POINT('Ctrl Pts',(67.3061123548589,333.47131228415,49.7154102637488));
#32139=CARTESIAN_POINT('Ctrl Pts',(69.0530157877858,333.259156274598,47.7501489809154));
#32140=CARTESIAN_POINT('Ctrl Pts',(70.7999192207128,333.047000265045,45.7848876980819));
#32141=CARTESIAN_POINT('Ctrl Pts',(73.6235679987656,332.834844255493,44.7723422589182));
#32142=CARTESIAN_POINT('Ctrl Pts',(76.2190150425094,332.622688245941,45.1799147983004));
#32143=CARTESIAN_POINT('Ctrl Pts',(78.8144620862531,332.410532236388,45.5874873376827));
#32144=CARTESIAN_POINT('Ctrl Pts',(81.1817073956878,332.198376226836,47.4151778556106));
#32145=CARTESIAN_POINT('Ctrl Pts',(82.2481526773765,331.986220217284,49.8203010055111));
#32146=CARTESIAN_POINT('Ctrl Pts',(82.6914282068279,331.898036070309,50.8200074658179));
#32147=CARTESIAN_POINT('Ctrl Pts',(82.9099634665863,331.809851923335,51.9194774275631));
#32148=CARTESIAN_POINT('Ctrl Pts',(82.9069840420526,331.72166777636,53.0202572588894));
#32149=CARTESIAN_POINT('Origin',(74.9879498948689,255.,53.0228109606356));
#32150=CARTESIAN_POINT('',(82.915920021327,326.278332223638,53.0238964569577));
#32151=CARTESIAN_POINT('',(82.9099077959009,327.721667776361,53.0246025132965));
#32152=CARTESIAN_POINT('',(82.9129498948689,255.,53.0228109606356));
#32153=CARTESIAN_POINT('Ctrl Pts',(82.9248220017562,326.278332223638,53.0271498763471));
#32154=CARTESIAN_POINT('Ctrl Pts',(82.9112391805045,326.475332829726,50.5837044358842));
#32155=CARTESIAN_POINT('Ctrl Pts',(81.6968655677976,326.672333435814,48.1267829301193));
#32156=CARTESIAN_POINT('Ctrl Pts',(79.74325571597,326.869334041903,46.6656411376162));
#32157=CARTESIAN_POINT('Ctrl Pts',(77.6393532020857,327.081490051455,45.0920926179295));
#32158=CARTESIAN_POINT('Ctrl Pts',(74.6780994082307,327.293646061007,44.6734293251219));
#32159=CARTESIAN_POINT('Ctrl Pts',(72.2116608408273,327.505802070559,45.5891824022388));
#32160=CARTESIAN_POINT('Ctrl Pts',(70.9784415571256,327.611880075336,46.0470589407973));
#32161=CARTESIAN_POINT('Ctrl Pts',(69.8689260800369,327.717958080112,46.8385395718368));
#32162=CARTESIAN_POINT('Ctrl Pts',(69.0018806483926,327.824036084888,47.839955495699));
#32163=CARTESIAN_POINT('Ctrl Pts',(68.1348352167483,327.930114089664,48.8413714195611));
#32164=CARTESIAN_POINT('Ctrl Pts',(67.5102598305485,328.03619209444,50.0527226362459));
#32165=CARTESIAN_POINT('Ctrl Pts',(67.2335564272066,328.142270099216,51.338769273361));
#32166=CARTESIAN_POINT('Ctrl Pts',(66.6801496205226,328.354426108769,53.910862547591));
#32167=CARTESIAN_POINT('Ctrl Pts',(67.5182307452699,328.566582118321,56.7817375035421));
#32168=CARTESIAN_POINT('Ctrl Pts',(69.3766344918117,328.778738127873,58.6388309978433));
#32169=CARTESIAN_POINT('Ctrl Pts',(71.2350382383536,328.990894137426,60.4959244921446));
#32170=CARTESIAN_POINT('Ctrl Pts',(74.1137646066901,329.203050146978,61.3392365247959));
#32171=CARTESIAN_POINT('Ctrl Pts',(76.6827331908784,329.41520615653,60.7785905337908));
#32172=CARTESIAN_POINT('Ctrl Pts',(79.2517017750665,329.627362166082,60.2179445427857));
#32173=CARTESIAN_POINT('Ctrl Pts',(81.5109125751065,329.839518175635,58.2533405281243));
#32174=CARTESIAN_POINT('Ctrl Pts',(82.4272284798771,330.051674185187,55.7893390962893));
#32175=CARTESIAN_POINT('Ctrl Pts',(82.7535455236642,330.127226864671,54.9118626070814));
#32176=CARTESIAN_POINT('Ctrl Pts',(82.9095561202415,330.202779544154,53.9710523453169));
#32177=CARTESIAN_POINT('Ctrl Pts',(82.903889038595,330.278332223638,53.0283217876032));
#32178=CARTESIAN_POINT('Ctrl Pts',(82.9129498948689,331.721667776361,53.0228109606494));
#32179=CARTESIAN_POINT('Ctrl Pts',(82.9129498948651,331.544571204362,55.2274084205592));
#32180=CARTESIAN_POINT('Ctrl Pts',(81.9432795991031,331.367474632363,57.4147653849937));
#32181=CARTESIAN_POINT('Ctrl Pts',(80.3096882702442,331.190378060364,58.8951806411017));
#32182=CARTESIAN_POINT('Ctrl Pts',(78.6760969413853,331.013281488366,60.3755958972098));
#32183=CARTESIAN_POINT('Ctrl Pts',(76.4041347530308,330.836184916367,61.1259150206704));
#32184=CARTESIAN_POINT('Ctrl Pts',(74.2101800112087,330.659088344368,60.9095529374008));
#32185=CARTESIAN_POINT('Ctrl Pts',(72.0162252693866,330.481991772369,60.6931908541312));
#32186=CARTESIAN_POINT('Ctrl Pts',(69.9345925076871,330.304895200371,59.5135315737613));
#32187=CARTESIAN_POINT('Ctrl Pts',(68.6216467656529,330.127798628372,57.7425365317822));
#32188=CARTESIAN_POINT('Ctrl Pts',(67.3087010236188,329.950702056373,55.971541489803));
#32189=CARTESIAN_POINT('Ctrl Pts',(66.7849774198229,329.773605484375,53.636909921617));
#32190=CARTESIAN_POINT('Ctrl Pts',(67.2156126057631,329.596508912376,51.4747805783836));
#32191=CARTESIAN_POINT('Ctrl Pts',(67.6462477917032,329.419412340377,49.3126512351503));
#32192=CARTESIAN_POINT('Ctrl Pts',(69.0245064208057,329.242315768378,47.3568408855387));
#32193=CARTESIAN_POINT('Ctrl Pts',(70.9158061804573,329.06521919638,46.2240411771249));
#32194=CARTESIAN_POINT('Ctrl Pts',(72.8071059401089,328.888122624381,45.0912414687111));
#32195=CARTESIAN_POINT('Ctrl Pts',(75.1818659698229,328.711026052382,44.7991699473061));
#32196=CARTESIAN_POINT('Ctrl Pts',(77.2912945088784,328.533929480384,45.4399204438792));
#32197=CARTESIAN_POINT('Ctrl Pts',(79.4007230479339,328.356832908385,46.0806709404524));
#32198=CARTESIAN_POINT('Ctrl Pts',(81.2118275942159,328.179736336386,47.6442218014032));
#32199=CARTESIAN_POINT('Ctrl Pts',(82.1535440633151,328.002639764387,49.6375657386272));
#32200=CARTESIAN_POINT('Ctrl Pts',(82.6515697929948,327.908982435045,50.6917435101897));
#32201=CARTESIAN_POINT('Ctrl Pts',(82.9129498948709,327.815325105703,51.8569119935515));
#32202=CARTESIAN_POINT('Ctrl Pts',(82.9129498948689,327.721667776361,53.0228109606492));
#32203=CARTESIAN_POINT('Origin',(74.9879498948689,255.,53.0228109606356));
#32204=CARTESIAN_POINT('',(82.9129498948689,322.278332223638,53.0228109606357));
#32205=CARTESIAN_POINT('',(82.9174913560738,323.721667776361,53.0236500017445));
#32206=CARTESIAN_POINT('',(82.9129498948689,255.,53.0228109606356));
#32207=CARTESIAN_POINT('Ctrl Pts',(82.9129498948689,322.278332223638,53.0228109606357));
#32208=CARTESIAN_POINT('Ctrl Pts',(82.9129498948689,322.455428795637,50.8182135007259));
#32209=CARTESIAN_POINT('Ctrl Pts',(81.9432795991108,322.632525367635,48.6308565362897));
#32210=CARTESIAN_POINT('Ctrl Pts',(80.3096882702545,322.809621939634,47.1504412801788));
#32211=CARTESIAN_POINT('Ctrl Pts',(78.6760969413982,322.986718511633,45.6700260240678));
#32212=CARTESIAN_POINT('Ctrl Pts',(76.4041347530451,323.163815083631,44.9197069006032));
#32213=CARTESIAN_POINT('Ctrl Pts',(74.2101800112226,323.34091165563,45.136068983869));
#32214=CARTESIAN_POINT('Ctrl Pts',(72.0162252694001,323.518008227629,45.3524310671347));
#32215=CARTESIAN_POINT('Ctrl Pts',(69.9345925076986,323.695104799628,46.5320903475009));
#32216=CARTESIAN_POINT('Ctrl Pts',(68.6216467656613,323.872201371626,48.3030853894778));
#32217=CARTESIAN_POINT('Ctrl Pts',(67.308701023624,324.049297943625,50.0740804314546));
#32218=CARTESIAN_POINT('Ctrl Pts',(66.784977419824,324.226394515624,52.4087119996396));
#32219=CARTESIAN_POINT('Ctrl Pts',(67.2156126057604,324.403491087622,54.5708413428738));
#32220=CARTESIAN_POINT('Ctrl Pts',(67.6462477916967,324.580587659621,56.7329706861079));
#32221=CARTESIAN_POINT('Ctrl Pts',(69.0245064207957,324.75768423162,58.6887810357219));
#32222=CARTESIAN_POINT('Ctrl Pts',(70.9158061804453,324.934780803619,59.8215807441391));
#32223=CARTESIAN_POINT('Ctrl Pts',(72.8071059400949,325.111877375617,60.9543804525562));
#32224=CARTESIAN_POINT('Ctrl Pts',(75.1818659698084,325.288973947616,61.2464519739654));
#32225=CARTESIAN_POINT('Ctrl Pts',(77.291294508865,325.466070519615,60.605701477396));
#32226=CARTESIAN_POINT('Ctrl Pts',(79.4007230479217,325.643167091614,59.9649509808266));
#32227=CARTESIAN_POINT('Ctrl Pts',(81.2118275942064,325.820263663612,58.401400119879));
#32228=CARTESIAN_POINT('Ctrl Pts',(82.1535440633091,325.997360235611,56.4080561826566));
#32229=CARTESIAN_POINT('Ctrl Pts',(82.6515697929907,326.091017564953,55.3538784110949));
#32230=CARTESIAN_POINT('Ctrl Pts',(82.9129498948689,326.184674894295,54.1887099277336));
#32231=CARTESIAN_POINT('Ctrl Pts',(82.9129498948689,326.278332223638,53.0228109606359));
#32232=CARTESIAN_POINT('Ctrl Pts',(82.9036744121771,327.721667776361,53.0282734770033));
#32233=CARTESIAN_POINT('Ctrl Pts',(82.909810152162,327.658093189802,53.8208117728148));
#32234=CARTESIAN_POINT('Ctrl Pts',(82.800678889337,327.594518603244,54.6119493203552));
#32235=CARTESIAN_POINT('Ctrl Pts',(82.569358847217,327.530944016685,55.3656410340849));
#32236=CARTESIAN_POINT('Ctrl Pts',(82.18338750456,327.424866011909,56.623220792551));
#32237=CARTESIAN_POINT('Ctrl Pts',(81.4572313483912,327.318788007133,57.776547901427));
#32238=CARTESIAN_POINT('Ctrl Pts',(80.5075017688919,327.212710002357,58.6999196353046));
#32239=CARTESIAN_POINT('Ctrl Pts',(79.5577721893926,327.106631997581,59.6232913691821));
#32240=CARTESIAN_POINT('Ctrl Pts',(78.3844691865628,327.000553992804,60.3167077280612));
#32241=CARTESIAN_POINT('Ctrl Pts',(77.1165269206526,326.894475988028,60.6671405127356));
#32242=CARTESIAN_POINT('Ctrl Pts',(74.5806423888323,326.682319978476,61.3680060820842));
#32243=CARTESIAN_POINT('Ctrl Pts',(71.6662008046903,326.470163968924,60.6969373546137));
#32244=CARTESIAN_POINT('Ctrl Pts',(69.7049914022054,326.258007959371,58.9487616164966));
#32245=CARTESIAN_POINT('Ctrl Pts',(67.7437819997204,326.045851949819,57.2005858783795));
#32246=CARTESIAN_POINT('Ctrl Pts',(66.7358047788924,325.833695940267,54.3753031296159));
#32247=CARTESIAN_POINT('Ctrl Pts',(67.1473169532818,325.621539930714,51.7782699676972));
#32248=CARTESIAN_POINT('Ctrl Pts',(67.5588291276712,325.409383921162,49.1812368057785));
#32249=CARTESIAN_POINT('Ctrl Pts',(69.3898306972781,325.19722791161,46.8124532307048));
#32250=CARTESIAN_POINT('Ctrl Pts',(71.7968676918125,324.985071902057,45.7555186062534));
#32251=CARTESIAN_POINT('Ctrl Pts',(74.2039046863469,324.772915892505,44.6985839818021));
#32252=CARTESIAN_POINT('Ctrl Pts',(77.1869771058089,324.560759882953,44.953498307973));
#32253=CARTESIAN_POINT('Ctrl Pts',(79.3775118827791,324.3486038734,46.4079675942286));
#32254=CARTESIAN_POINT('Ctrl Pts',(81.535240569327,324.139625174387,47.8406543224425));
#32255=CARTESIAN_POINT('Ctrl Pts',(82.9239924073639,323.930646475374,50.4372352852841));
#32256=CARTESIAN_POINT('Ctrl Pts',(82.926795049106,323.721667776361,53.0253688716062));
#32257=CARTESIAN_POINT('Origin',(74.9879498948689,255.,53.0228109606356));
#32258=CARTESIAN_POINT('',(82.9077404809001,318.278332223638,53.0233273752923));
#32259=CARTESIAN_POINT('',(82.9129498948689,319.721667776361,53.0228109606489));
#32260=CARTESIAN_POINT('',(82.9129498948689,255.,53.0228109606356));
#32261=CARTESIAN_POINT('Ctrl Pts',(82.9129498948689,318.278332223638,53.0228109606357));
#32262=CARTESIAN_POINT('Ctrl Pts',(82.9129498948689,318.455428795637,50.818213500726));
#32263=CARTESIAN_POINT('Ctrl Pts',(81.9432795991108,318.632525367635,48.6308565362898));
#32264=CARTESIAN_POINT('Ctrl Pts',(80.3096882702546,318.809621939634,47.1504412801788));
#32265=CARTESIAN_POINT('Ctrl Pts',(78.6760969413983,318.986718511633,45.6700260240679));
#32266=CARTESIAN_POINT('Ctrl Pts',(76.4041347530451,319.163815083631,44.9197069006032));
#32267=CARTESIAN_POINT('Ctrl Pts',(74.2101800112226,319.34091165563,45.1360689838689));
#32268=CARTESIAN_POINT('Ctrl Pts',(72.0162252694001,319.518008227629,45.3524310671347));
#32269=CARTESIAN_POINT('Ctrl Pts',(69.9345925076986,319.695104799628,46.5320903475009));
#32270=CARTESIAN_POINT('Ctrl Pts',(68.6216467656613,319.872201371626,48.3030853894777));
#32271=CARTESIAN_POINT('Ctrl Pts',(67.308701023624,320.049297943625,50.0740804314546));
#32272=CARTESIAN_POINT('Ctrl Pts',(66.784977419824,320.226394515624,52.4087119996396));
#32273=CARTESIAN_POINT('Ctrl Pts',(67.2156126057603,320.403491087623,54.5708413428737));
#32274=CARTESIAN_POINT('Ctrl Pts',(67.6462477916967,320.580587659621,56.7329706861079));
#32275=CARTESIAN_POINT('Ctrl Pts',(69.0245064207957,320.75768423162,58.6887810357219));
#32276=CARTESIAN_POINT('Ctrl Pts',(70.9158061804453,320.934780803619,59.821580744139));
#32277=CARTESIAN_POINT('Ctrl Pts',(72.8071059400948,321.111877375617,60.9543804525562));
#32278=CARTESIAN_POINT('Ctrl Pts',(75.1818659698083,321.288973947616,61.2464519739654));
#32279=CARTESIAN_POINT('Ctrl Pts',(77.291294508865,321.466070519615,60.605701477396));
#32280=CARTESIAN_POINT('Ctrl Pts',(79.4007230479216,321.643167091614,59.9649509808266));
#32281=CARTESIAN_POINT('Ctrl Pts',(81.2118275942063,321.820263663612,58.401400119879));
#32282=CARTESIAN_POINT('Ctrl Pts',(82.1535440633091,321.997360235611,56.4080561826566));
#32283=CARTESIAN_POINT('Ctrl Pts',(82.6515697929907,322.091017564953,55.3538784110949));
#32284=CARTESIAN_POINT('Ctrl Pts',(82.9129498948689,322.184674894295,54.1887099277335));
#32285=CARTESIAN_POINT('Ctrl Pts',(82.9129498948689,322.278332223638,53.0228109606357));
#32286=CARTESIAN_POINT('Ctrl Pts',(82.9129498948689,323.721667776361,53.0228109606491));
#32287=CARTESIAN_POINT('Ctrl Pts',(82.9129498948652,323.544571204362,55.2274084205588));
#32288=CARTESIAN_POINT('Ctrl Pts',(81.9432795991032,323.367474632363,57.4147653849934));
#32289=CARTESIAN_POINT('Ctrl Pts',(80.3096882702444,323.190378060364,58.8951806411015));
#32290=CARTESIAN_POINT('Ctrl Pts',(78.6760969413856,323.013281488366,60.3755958972097));
#32291=CARTESIAN_POINT('Ctrl Pts',(76.4041347530311,322.836184916367,61.1259150206704));
#32292=CARTESIAN_POINT('Ctrl Pts',(74.210180011209,322.659088344368,60.9095529374009));
#32293=CARTESIAN_POINT('Ctrl Pts',(72.0162252693869,322.48199177237,60.6931908541313));
#32294=CARTESIAN_POINT('Ctrl Pts',(69.9345925076874,322.304895200371,59.5135315737615));
#32295=CARTESIAN_POINT('Ctrl Pts',(68.6216467656531,322.127798628372,57.7425365317824));
#32296=CARTESIAN_POINT('Ctrl Pts',(67.3087010236189,321.950702056373,55.9715414898033));
#32297=CARTESIAN_POINT('Ctrl Pts',(66.784977419823,321.773605484375,53.6369099216174));
#32298=CARTESIAN_POINT('Ctrl Pts',(67.215612605763,321.596508912376,51.474780578384));
#32299=CARTESIAN_POINT('Ctrl Pts',(67.6462477917031,321.419412340377,49.3126512351506));
#32300=CARTESIAN_POINT('Ctrl Pts',(69.0245064208055,321.242315768378,47.3568408855389));
#32301=CARTESIAN_POINT('Ctrl Pts',(70.915806180457,321.06521919638,46.2240411771251));
#32302=CARTESIAN_POINT('Ctrl Pts',(72.8071059401085,320.888122624381,45.0912414687112));
#32303=CARTESIAN_POINT('Ctrl Pts',(75.1818659698225,320.711026052382,44.7991699473061));
#32304=CARTESIAN_POINT('Ctrl Pts',(77.2912945088781,320.533929480384,45.4399204438791));
#32305=CARTESIAN_POINT('Ctrl Pts',(79.4007230479336,320.356832908385,46.0806709404522));
#32306=CARTESIAN_POINT('Ctrl Pts',(81.2118275942156,320.179736336386,47.6442218014029));
#32307=CARTESIAN_POINT('Ctrl Pts',(82.1535440633149,320.002639764387,49.6375657386269));
#32308=CARTESIAN_POINT('Ctrl Pts',(82.6515697929947,319.908982435045,50.6917435101893));
#32309=CARTESIAN_POINT('Ctrl Pts',(82.9129498948708,319.815325105703,51.856911993551));
#32310=CARTESIAN_POINT('Ctrl Pts',(82.9129498948689,319.721667776361,53.0228109606487));
#32311=CARTESIAN_POINT('Origin',(74.9879498948689,255.,53.0228109606356));
#32312=CARTESIAN_POINT('',(82.9130547149714,314.278332223638,53.0229888658931));
#32313=CARTESIAN_POINT('',(82.9100618310243,315.721667776361,53.0233010180067));
#32314=CARTESIAN_POINT('',(82.9129498948689,255.,53.0228109606356));
#32315=CARTESIAN_POINT('Ctrl Pts',(82.9159347025624,314.278332223638,53.0278769066855));
#32316=CARTESIAN_POINT('Ctrl Pts',(82.9110875624937,314.338290643456,52.2818585047472));
#32317=CARTESIAN_POINT('Ctrl Pts',(82.8007484662297,314.398249063274,51.534267327686));
#32318=CARTESIAN_POINT('Ctrl Pts',(82.5920056934082,314.458207483092,50.8152441537794));
#32319=CARTESIAN_POINT('Ctrl Pts',(82.2226994822118,314.564285487869,49.5431535298568));
#32320=CARTESIAN_POINT('Ctrl Pts',(81.5453855151546,314.670363492644,48.3604819891323));
#32321=CARTESIAN_POINT('Ctrl Pts',(80.6162927679135,314.77644149742,47.4292100668239));
#32322=CARTESIAN_POINT('Ctrl Pts',(78.7581072734314,314.988597506973,45.5666662222072));
#32323=CARTESIAN_POINT('Ctrl Pts',(75.8928066582134,315.200753516525,44.7097208512549));
#32324=CARTESIAN_POINT('Ctrl Pts',(73.3238802807332,315.412909526078,45.2602460539687));
#32325=CARTESIAN_POINT('Ctrl Pts',(70.7549539032529,315.62506553563,45.8107712566825));
#32326=CARTESIAN_POINT('Ctrl Pts',(68.4824017635105,315.837221545182,47.7687670330626));
#32327=CARTESIAN_POINT('Ctrl Pts',(67.5566775306894,316.049377554734,50.229855848718));
#32328=CARTESIAN_POINT('Ctrl Pts',(66.6309532978684,316.261533564287,52.6909446643735));
#32329=CARTESIAN_POINT('Ctrl Pts',(67.0520569719687,316.473689573839,55.6551265193043));
#32330=CARTESIAN_POINT('Ctrl Pts',(68.6222579787399,316.685845583392,57.7635398307203));
#32331=CARTESIAN_POINT('Ctrl Pts',(70.1924589855109,316.898001592944,59.8719531421361));
#32332=CARTESIAN_POINT('Ctrl Pts',(72.9117573249526,317.110157602496,61.1245979100374));
#32333=CARTESIAN_POINT('Ctrl Pts',(75.5348949136829,317.322313612048,60.9427388867091));
#32334=CARTESIAN_POINT('Ctrl Pts',(78.1580325024134,317.534469621601,60.7608798633808));
#32335=CARTESIAN_POINT('Ctrl Pts',(80.6850093404324,317.746625631153,59.1445170488228));
#32336=CARTESIAN_POINT('Ctrl Pts',(81.9484164186813,317.958781640706,56.840984264952));
#32337=CARTESIAN_POINT('Ctrl Pts',(82.5827333838041,318.065298501683,55.6844528906374));
#32338=CARTESIAN_POINT('Ctrl Pts',(82.898538739761,318.17181536266,54.3547046353364));
#32339=CARTESIAN_POINT('Ctrl Pts',(82.8973003436811,318.278332223638,53.0243623170167));
#32340=CARTESIAN_POINT('Ctrl Pts',(82.9129498948689,319.721667776361,53.0228109606487));
#32341=CARTESIAN_POINT('Ctrl Pts',(82.9129498948653,319.544571204362,55.2274084205585));
#32342=CARTESIAN_POINT('Ctrl Pts',(81.9432795991034,319.367474632363,57.4147653849932));
#32343=CARTESIAN_POINT('Ctrl Pts',(80.3096882702445,319.190378060364,58.8951806411014));
#32344=CARTESIAN_POINT('Ctrl Pts',(78.6760969413857,319.013281488366,60.3755958972096));
#32345=CARTESIAN_POINT('Ctrl Pts',(76.4041347530312,318.836184916367,61.1259150206704));
#32346=CARTESIAN_POINT('Ctrl Pts',(74.210180011209,318.659088344368,60.9095529374009));
#32347=CARTESIAN_POINT('Ctrl Pts',(72.0162252693868,318.481991772369,60.6931908541313));
#32348=CARTESIAN_POINT('Ctrl Pts',(69.9345925076872,318.304895200371,59.5135315737614));
#32349=CARTESIAN_POINT('Ctrl Pts',(68.621646765653,318.127798628372,57.7425365317822));
#32350=CARTESIAN_POINT('Ctrl Pts',(67.3087010236187,317.950702056373,55.971541489803));
#32351=CARTESIAN_POINT('Ctrl Pts',(66.7849774198229,317.773605484375,53.6369099216169));
#32352=CARTESIAN_POINT('Ctrl Pts',(67.2156126057631,317.596508912376,51.4747805783835));
#32353=CARTESIAN_POINT('Ctrl Pts',(67.6462477917033,317.419412340377,49.31265123515));
#32354=CARTESIAN_POINT('Ctrl Pts',(69.0245064208059,317.242315768378,47.3568408855384));
#32355=CARTESIAN_POINT('Ctrl Pts',(70.9158061804576,317.06521919638,46.2240411771247));
#32356=CARTESIAN_POINT('Ctrl Pts',(72.8071059401093,316.888122624381,45.0912414687109));
#32357=CARTESIAN_POINT('Ctrl Pts',(75.1818659698235,316.711026052382,44.7991699473061));
#32358=CARTESIAN_POINT('Ctrl Pts',(77.291294508879,316.533929480384,45.4399204438794));
#32359=CARTESIAN_POINT('Ctrl Pts',(79.4007230479345,316.356832908385,46.0806709404527));
#32360=CARTESIAN_POINT('Ctrl Pts',(81.2118275942164,316.179736336386,47.6442218014038));
#32361=CARTESIAN_POINT('Ctrl Pts',(82.1535440633154,316.002639764387,49.637565738628));
#32362=CARTESIAN_POINT('Ctrl Pts',(82.6515697929949,315.908982435045,50.6917435101901));
#32363=CARTESIAN_POINT('Ctrl Pts',(82.9129498948708,315.815325105703,51.8569119935514));
#32364=CARTESIAN_POINT('Ctrl Pts',(82.9129498948689,315.721667776361,53.0228109606487));
#32365=CARTESIAN_POINT('Origin',(74.9879498948689,255.,53.0228109606356));
#32366=CARTESIAN_POINT('',(82.9151502769548,310.278332223638,53.0224445370273));
#32367=CARTESIAN_POINT('',(82.9178004843628,311.721667776361,53.029085373757));
#32368=CARTESIAN_POINT('',(82.9129498948689,255.,53.0228109606356));
#32369=CARTESIAN_POINT('Ctrl Pts',(82.9129498948689,310.278332223638,53.0228109606354));
#32370=CARTESIAN_POINT('Ctrl Pts',(82.9129498948688,310.455428795637,50.8182135007256));
#32371=CARTESIAN_POINT('Ctrl Pts',(81.9432795991106,310.632525367635,48.6308565362894));
#32372=CARTESIAN_POINT('Ctrl Pts',(80.3096882702541,310.809621939634,47.1504412801784));
#32373=CARTESIAN_POINT('Ctrl Pts',(78.6760969413977,310.986718511633,45.6700260240675));
#32374=CARTESIAN_POINT('Ctrl Pts',(76.4041347530444,311.163815083631,44.9197069006031));
#32375=CARTESIAN_POINT('Ctrl Pts',(74.2101800112218,311.34091165563,45.136068983869));
#32376=CARTESIAN_POINT('Ctrl Pts',(72.0162252693993,311.518008227629,45.352431067135));
#32377=CARTESIAN_POINT('Ctrl Pts',(69.9345925076978,311.695104799628,46.5320903475014));
#32378=CARTESIAN_POINT('Ctrl Pts',(68.6216467656607,311.872201371626,48.3030853894785));
#32379=CARTESIAN_POINT('Ctrl Pts',(67.3087010236236,312.049297943625,50.0740804314556));
#32380=CARTESIAN_POINT('Ctrl Pts',(66.7849774198239,312.226394515624,52.4087119996408));
#32381=CARTESIAN_POINT('Ctrl Pts',(67.2156126057606,312.403491087623,54.5708413428749));
#32382=CARTESIAN_POINT('Ctrl Pts',(67.6462477916973,312.580587659621,56.7329706861091));
#32383=CARTESIAN_POINT('Ctrl Pts',(69.0245064207967,312.75768423162,58.688781035723));
#32384=CARTESIAN_POINT('Ctrl Pts',(70.9158061804465,312.934780803619,59.8215807441398));
#32385=CARTESIAN_POINT('Ctrl Pts',(72.8071059400964,313.111877375617,60.9543804525566));
#32386=CARTESIAN_POINT('Ctrl Pts',(75.18186596981,313.288973947616,61.2464519739654));
#32387=CARTESIAN_POINT('Ctrl Pts',(77.2912945088666,313.466070519615,60.6057014773955));
#32388=CARTESIAN_POINT('Ctrl Pts',(79.4007230479232,313.643167091614,59.9649509808256));
#32389=CARTESIAN_POINT('Ctrl Pts',(81.2118275942076,313.820263663612,58.4014001198776));
#32390=CARTESIAN_POINT('Ctrl Pts',(82.1535440633099,313.997360235611,56.4080561826549));
#32391=CARTESIAN_POINT('Ctrl Pts',(82.6515697929911,314.091017564953,55.3538784110935));
#32392=CARTESIAN_POINT('Ctrl Pts',(82.9129498948689,314.184674894296,54.1887099277326));
#32393=CARTESIAN_POINT('Ctrl Pts',(82.9129498948689,314.278332223638,53.0228109606353));
#32394=CARTESIAN_POINT('Ctrl Pts',(82.9009180699073,315.721667776361,53.0248525651369));
#32395=CARTESIAN_POINT('Ctrl Pts',(82.9045269433347,315.627129008308,54.2057564279726));
#32396=CARTESIAN_POINT('Ctrl Pts',(82.6573714271191,315.532590240256,55.385490302401));
#32397=CARTESIAN_POINT('Ctrl Pts',(82.1523311861863,315.438051472203,56.4427594866264));
#32398=CARTESIAN_POINT('Ctrl Pts',(81.0189620468701,315.225895462651,58.8153947109755));
#32399=CARTESIAN_POINT('Ctrl Pts',(78.5868702499663,315.013739453099,60.5712905449027));
#32400=CARTESIAN_POINT('Ctrl Pts',(75.9801962493432,314.801583443546,60.8994846737545));
#32401=CARTESIAN_POINT('Ctrl Pts',(73.3735222487202,314.589427433994,61.2276788026062));
#32402=CARTESIAN_POINT('Ctrl Pts',(70.5922660443779,314.377271424442,60.1281712263825));
#32403=CARTESIAN_POINT('Ctrl Pts',(68.9006517877288,314.165115414889,58.1131367076396));
#32404=CARTESIAN_POINT('Ctrl Pts',(68.0548446594043,314.059037410113,57.1056194482682));
#32405=CARTESIAN_POINT('Ctrl Pts',(67.4814480180031,313.952959405337,55.869220453267));
#32406=CARTESIAN_POINT('Ctrl Pts',(67.2225927592744,313.846881400561,54.5701455562236));
#32407=CARTESIAN_POINT('Ctrl Pts',(66.9637375005457,313.740803395785,53.2710706591802));
#32408=CARTESIAN_POINT('Ctrl Pts',(67.0194236244894,313.634725391009,51.9093198600946));
#32409=CARTESIAN_POINT('Ctrl Pts',(67.4144453457865,313.528647386232,50.6545535209066));
#32410=CARTESIAN_POINT('Ctrl Pts',(68.2044887883807,313.31649137668,48.1450208425304));
#32411=CARTESIAN_POINT('Ctrl Pts',(70.351874620388,313.104335367128,46.0634260037446));
#32412=CARTESIAN_POINT('Ctrl Pts',(72.8852552910209,312.892179357576,45.3674065288727));
#32413=CARTESIAN_POINT('Ctrl Pts',(75.4186359616536,312.680023348023,44.6713870540009));
#32414=CARTESIAN_POINT('Ctrl Pts',(78.3380114709119,312.467867338471,45.360942943043));
#32415=CARTESIAN_POINT('Ctrl Pts',(80.2942558082632,312.255711328918,47.1179379932229));
#32416=CARTESIAN_POINT('Ctrl Pts',(81.935688886677,312.077696811399,48.5921862447881));
#32417=CARTESIAN_POINT('Ctrl Pts',(82.8990346722933,311.89968229388,50.8179592648528));
#32418=CARTESIAN_POINT('Ctrl Pts',(82.9178004843628,311.721667776361,53.029085373757));
#32419=CARTESIAN_POINT('Origin',(74.9879498948689,255.,53.0228109606356));
#32420=CARTESIAN_POINT('',(82.909363478242,306.278332223638,53.0203308108944));
#32421=CARTESIAN_POINT('',(82.9221877016763,307.721667776361,53.0184879124944));
#32422=CARTESIAN_POINT('',(82.9129498948689,255.,53.0228109606356));
#32423=CARTESIAN_POINT('Ctrl Pts',(82.9033131639287,306.278332223638,53.0161467779089));
#32424=CARTESIAN_POINT('Ctrl Pts',(82.9104530950279,306.353007190719,52.0851637795933));
#32425=CARTESIAN_POINT('Ctrl Pts',(82.7594722917077,306.427682157799,51.156220880406));
#32426=CARTESIAN_POINT('Ctrl Pts',(82.4409791193906,306.50235712488,50.288053752156));
#32427=CARTESIAN_POINT('Ctrl Pts',(81.5361211308319,306.714513134433,47.8215394602294));
#32428=CARTESIAN_POINT('Ctrl Pts',(79.2791673003925,306.926669143985,45.8455839709954));
#32429=CARTESIAN_POINT('Ctrl Pts',(76.7126907808753,307.138825153537,45.2736383542251));
#32430=CARTESIAN_POINT('Ctrl Pts',(74.146214261358,307.35098116309,44.7016927374548));
#32431=CARTESIAN_POINT('Ctrl Pts',(71.2702150527629,307.563137172642,45.5337569931483));
#32432=CARTESIAN_POINT('Ctrl Pts',(69.402473289473,307.775293182194,47.3837512091079));
#32433=CARTESIAN_POINT('Ctrl Pts',(67.5347315261831,307.987449191747,49.2337454250674));
#32434=CARTESIAN_POINT('Ctrl Pts',(66.6752472081982,308.199605201299,52.101669601293));
#32435=CARTESIAN_POINT('Ctrl Pts',(67.2226638744058,308.411761210851,54.6734896780741));
#32436=CARTESIAN_POINT('Ctrl Pts',(67.7700805406134,308.623917220403,57.2453097548552));
#32437=CARTESIAN_POINT('Ctrl Pts',(69.7243981910132,308.836073229956,59.5210257321916));
#32438=CARTESIAN_POINT('Ctrl Pts',(72.1821611308745,309.048229239508,60.4493909960724));
#32439=CARTESIAN_POINT('Ctrl Pts',(74.6399240707361,309.260385249061,61.3777562599533));
#32440=CARTESIAN_POINT('Ctrl Pts',(77.6011323000593,309.472541258613,60.9587708103782));
#32441=CARTESIAN_POINT('Ctrl Pts',(79.716867816474,309.684697268165,59.3949338209173));
#32442=CARTESIAN_POINT('Ctrl Pts',(80.7747355746812,309.790775272941,58.6130153261869));
#32443=CARTESIAN_POINT('Ctrl Pts',(81.6212351546614,309.896853277717,57.5448839464852));
#32444=CARTESIAN_POINT('Ctrl Pts',(82.1765551040712,310.002931282493,56.342294495805));
#32445=CARTESIAN_POINT('Ctrl Pts',(82.6571311261736,310.094731596208,55.3015689554307));
#32446=CARTESIAN_POINT('Ctrl Pts',(82.9196357860859,310.186531909923,54.1601445624674));
#32447=CARTESIAN_POINT('Ctrl Pts',(82.9227432920407,310.278332223638,53.021180093001));
#32448=CARTESIAN_POINT('Ctrl Pts',(82.9178004843628,311.721667776361,53.029085373757));
#32449=CARTESIAN_POINT('Ctrl Pts',(82.9213995887066,311.687526284328,53.4531583397328));
#32450=CARTESIAN_POINT('Ctrl Pts',(82.8902536476416,311.653384792295,53.8766925396881));
#32451=CARTESIAN_POINT('Ctrl Pts',(82.8224826236741,311.619243300262,54.2942828289855));
#32452=CARTESIAN_POINT('Ctrl Pts',(82.4013519362892,311.407087290709,56.8891984032508));
#32453=CARTESIAN_POINT('Ctrl Pts',(80.5659773960746,311.194931281157,59.2545953404634));
#32454=CARTESIAN_POINT('Ctrl Pts',(78.1544837942863,310.982775271605,60.3027471053861));
#32455=CARTESIAN_POINT('Ctrl Pts',(75.7429901924981,310.770619262052,61.3508988703087));
#32456=CARTESIAN_POINT('Ctrl Pts',(72.7553775291362,310.5584632525,61.0818054629415));
#32457=CARTESIAN_POINT('Ctrl Pts',(70.5721394437577,310.346307242948,59.6203225878146));
#32458=CARTESIAN_POINT('Ctrl Pts',(68.3889013583791,310.134151233396,58.1588397126877));
#32459=CARTESIAN_POINT('Ctrl Pts',(67.0100378509841,309.921995223843,55.5049673698008));
#32460=CARTESIAN_POINT('Ctrl Pts',(67.0541876334774,309.709839214291,52.8743830807635));
#32461=CARTESIAN_POINT('Ctrl Pts',(67.0762625247241,309.603761209515,51.5590909362448));
#32462=CARTESIAN_POINT('Ctrl Pts',(67.4540907384429,309.497683204738,50.2496208051885));
#32463=CARTESIAN_POINT('Ctrl Pts',(68.1104952068112,309.391605199962,49.0990840578369));
#32464=CARTESIAN_POINT('Ctrl Pts',(68.7668996751795,309.285527195186,47.9485473104855));
#32465=CARTESIAN_POINT('Ctrl Pts',(69.7018803981972,309.17944919041,46.9569439468388));
#32466=CARTESIAN_POINT('Ctrl Pts',(70.8229059287894,309.073371185634,46.2686253534415));
#32467=CARTESIAN_POINT('Ctrl Pts',(73.0649569899737,308.861215176081,44.891988166647));
#32468=CARTESIAN_POINT('Ctrl Pts',(76.0511872814558,308.649059166529,44.7284900608501));
#32469=CARTESIAN_POINT('Ctrl Pts',(78.4202823957525,308.436903156977,45.8642052853462));
#32470=CARTESIAN_POINT('Ctrl Pts',(80.7893775100491,308.224747147425,46.9999205098423));
#32471=CARTESIAN_POINT('Ctrl Pts',(82.5413374471603,308.012591137873,49.4348490646314));
#32472=CARTESIAN_POINT('Ctrl Pts',(82.8661863365622,307.80043512832,52.0441395261994));
#32473=CARTESIAN_POINT('Ctrl Pts',(82.9063886494091,307.774179344334,52.3670573962203));
#32474=CARTESIAN_POINT('Ctrl Pts',(82.9247336340708,307.747923560347,52.6926457559872));
#32475=CARTESIAN_POINT('Ctrl Pts',(82.9221877016763,307.721667776361,53.0184879124944));
#32476=CARTESIAN_POINT('Origin',(74.9879498948689,255.,53.0228109606356));
#32477=CARTESIAN_POINT('',(82.9095685911471,302.278332223638,53.0255146867421));
#32478=CARTESIAN_POINT('',(82.908600234471,303.721667776361,53.0206776223734));
#32479=CARTESIAN_POINT('',(82.9129498948689,255.,53.0228109606356));
#32480=CARTESIAN_POINT('Ctrl Pts',(82.9129498948689,302.278332223638,53.0228109606348));
#32481=CARTESIAN_POINT('Ctrl Pts',(82.9129498948687,302.455428795637,50.8182135007249));
#32482=CARTESIAN_POINT('Ctrl Pts',(81.9432795991102,302.632525367635,48.6308565362887));
#32483=CARTESIAN_POINT('Ctrl Pts',(80.3096882702535,302.809621939634,47.1504412801779));
#32484=CARTESIAN_POINT('Ctrl Pts',(78.6760969413969,302.986718511633,45.6700260240671));
#32485=CARTESIAN_POINT('Ctrl Pts',(76.4041347530434,303.163815083632,44.9197069006029));
#32486=CARTESIAN_POINT('Ctrl Pts',(74.2101800112208,303.34091165563,45.1360689838691));
#32487=CARTESIAN_POINT('Ctrl Pts',(72.0162252693982,303.518008227629,45.3524310671354));
#32488=CARTESIAN_POINT('Ctrl Pts',(69.9345925076968,303.695104799628,46.5320903475022));
#32489=CARTESIAN_POINT('Ctrl Pts',(68.6216467656599,303.872201371626,48.3030853894795));
#32490=CARTESIAN_POINT('Ctrl Pts',(67.308701023623,304.049297943625,50.0740804314569));
#32491=CARTESIAN_POINT('Ctrl Pts',(66.7849774198238,304.226394515624,52.4087119996423));
#32492=CARTESIAN_POINT('Ctrl Pts',(67.2156126057609,304.403491087623,54.5708413428764));
#32493=CARTESIAN_POINT('Ctrl Pts',(67.646247791698,304.580587659621,56.7329706861105));
#32494=CARTESIAN_POINT('Ctrl Pts',(69.0245064207978,304.75768423162,58.6887810357242));
#32495=CARTESIAN_POINT('Ctrl Pts',(70.915806180448,304.934780803619,59.8215807441407));
#32496=CARTESIAN_POINT('Ctrl Pts',(72.8071059400981,305.111877375618,60.9543804525571));
#32497=CARTESIAN_POINT('Ctrl Pts',(75.1818659698119,305.288973947616,61.2464519739654));
#32498=CARTESIAN_POINT('Ctrl Pts',(77.2912945088684,305.466070519615,60.6057014773949));
#32499=CARTESIAN_POINT('Ctrl Pts',(79.4007230479249,305.643167091614,59.9649509808245));
#32500=CARTESIAN_POINT('Ctrl Pts',(81.211827594209,305.820263663613,58.4014001198759));
#32501=CARTESIAN_POINT('Ctrl Pts',(82.1535440633108,305.997360235611,56.4080561826529));
#32502=CARTESIAN_POINT('Ctrl Pts',(82.6515697929914,306.091017564954,55.353878411092));
#32503=CARTESIAN_POINT('Ctrl Pts',(82.912949894869,306.184674894296,54.1887099277317));
#32504=CARTESIAN_POINT('Ctrl Pts',(82.9129498948689,306.278332223638,53.022810960635));
#32505=CARTESIAN_POINT('Ctrl Pts',(82.9221877016763,307.721667776361,53.0184879124944));
#32506=CARTESIAN_POINT('Ctrl Pts',(82.9041616009639,307.535767550795,55.3255654853793));
#32507=CARTESIAN_POINT('Ctrl Pts',(81.8388445351564,307.349867325229,57.6453662447269));
#32508=CARTESIAN_POINT('Ctrl Pts',(80.069262236979,307.163967099663,59.1200897530678));
#32509=CARTESIAN_POINT('Ctrl Pts',(78.0497514063015,306.95181109011,60.8030971500206));
#32510=CARTESIAN_POINT('Ctrl Pts',(75.112991903254,306.739655080558,61.3854595755789));
#32511=CARTESIAN_POINT('Ctrl Pts',(72.6050182791123,306.527499071006,60.5955280504543));
#32512=CARTESIAN_POINT('Ctrl Pts',(70.0970446549707,306.315343061454,59.8055965253297));
#32513=CARTESIAN_POINT('Ctrl Pts',(68.0178569097347,306.103187051901,57.6433710495224));
#32514=CARTESIAN_POINT('Ctrl Pts',(67.327852786392,305.891031042349,55.1083454004399));
#32515=CARTESIAN_POINT('Ctrl Pts',(66.6378486630492,305.678875032797,52.5733197513572));
#32516=CARTESIAN_POINT('Ctrl Pts',(67.3370281615999,305.466719023245,49.6654939289993));
#32517=CARTESIAN_POINT('Ctrl Pts',(69.0953083595857,305.254563013692,47.7083598890329));
#32518=CARTESIAN_POINT('Ctrl Pts',(69.9744484585786,305.148485008916,46.7297928690498));
#32519=CARTESIAN_POINT('Ctrl Pts',(71.1183637324302,305.04240700414,45.9888987946646));
#32520=CARTESIAN_POINT('Ctrl Pts',(72.3683863154353,304.936328999363,45.550669202924));
#32521=CARTESIAN_POINT('Ctrl Pts',(73.6184088984404,304.830250994587,45.1124396111834));
#32522=CARTESIAN_POINT('Ctrl Pts',(74.9745387905989,304.724172989811,44.9768745020875));
#32523=CARTESIAN_POINT('Ctrl Pts',(76.2722597746717,304.618094985035,45.1922833546281));
#32524=CARTESIAN_POINT('Ctrl Pts',(78.8677017428175,304.405938975483,45.6231010597095));
#32525=CARTESIAN_POINT('Ctrl Pts',(81.2295080786204,304.193782965931,47.4578146113376));
#32526=CARTESIAN_POINT('Ctrl Pts',(82.2734486764291,303.981626956378,49.8687581527721));
#32527=CARTESIAN_POINT('Ctrl Pts',(82.6998360667996,303.894973896372,50.8534846085884));
#32528=CARTESIAN_POINT('Ctrl Pts',(82.906372531569,303.808320836366,51.9343397465352));
#32529=CARTESIAN_POINT('Ctrl Pts',(82.9016479285953,303.721667776361,53.0172677883023));
#32530=CARTESIAN_POINT('Origin',(74.9879498948689,255.,53.0228109606356));
#32531=CARTESIAN_POINT('',(82.9247849645265,298.278332223638,53.0254077151713));
#32532=CARTESIAN_POINT('',(82.9107328264417,299.721667776361,53.0254029102435));
#32533=CARTESIAN_POINT('',(82.9129498948689,255.,53.0228109606356));
#32534=CARTESIAN_POINT('Ctrl Pts',(82.9247849645265,298.278332223638,53.0254077151713));
#32535=CARTESIAN_POINT('Ctrl Pts',(82.9108749806662,298.473801742758,50.6015025294555));
#32536=CARTESIAN_POINT('Ctrl Pts',(81.7179195953142,298.669271261877,48.1678523004493));
#32537=CARTESIAN_POINT('Ctrl Pts',(79.7892377761479,298.864740780997,46.7026702603182));
#32538=CARTESIAN_POINT('Ctrl Pts',(77.6959117154242,299.076896790549,45.112411194343));
#32539=CARTESIAN_POINT('Ctrl Pts',(74.735885354018,299.289052800102,44.6630268229847));
#32540=CARTESIAN_POINT('Ctrl Pts',(72.2660705525556,299.501208809654,45.5652121477675));
#32541=CARTESIAN_POINT('Ctrl Pts',(69.7962557510931,299.713364819206,46.4673974725502));
#32542=CARTESIAN_POINT('Ctrl Pts',(67.8166525095745,299.925520828759,48.721152493474));
#32543=CARTESIAN_POINT('Ctrl Pts',(67.2416261249463,300.137676838311,51.2847057674901));
#32544=CARTESIAN_POINT('Ctrl Pts',(66.6665997403182,300.349832847863,53.848259041506));
#32545=CARTESIAN_POINT('Ctrl Pts',(67.4961502125804,300.561988857416,56.7216105686142));
#32546=CARTESIAN_POINT('Ctrl Pts',(69.3408685422965,300.774144866968,58.5974936110859));
#32547=CARTESIAN_POINT('Ctrl Pts',(70.2632277071545,300.880222871744,59.5354351323217));
#32548=CARTESIAN_POINT('Ctrl Pts',(71.439378836376,300.98630087652,60.2240095323984));
#32549=CARTESIAN_POINT('Ctrl Pts',(72.7078856112961,301.092378881296,60.6054439239807));
#32550=CARTESIAN_POINT('Ctrl Pts',(73.9763923862162,301.198456886072,60.986878315563));
#32551=CARTESIAN_POINT('Ctrl Pts',(75.3372548068349,301.304534890849,61.0611726986508));
#32552=CARTESIAN_POINT('Ctrl Pts',(76.6239461579206,301.410612895625,60.7874829229971));
#32553=CARTESIAN_POINT('Ctrl Pts',(79.1973288600919,301.622768905177,60.2401033716898));
#32554=CARTESIAN_POINT('Ctrl Pts',(81.4740272841313,301.83492491473,58.3007871854165));
#32555=CARTESIAN_POINT('Ctrl Pts',(82.4082238324473,302.047080924282,55.8452347952502));
#32556=CARTESIAN_POINT('Ctrl Pts',(82.7476504115135,302.124164690734,54.9530459416149));
#32557=CARTESIAN_POINT('Ctrl Pts',(82.9098499119628,302.201248457186,53.9927074369835));
#32558=CARTESIAN_POINT('Ctrl Pts',(82.9038476214953,302.278332223638,53.0300892343956));
#32559=CARTESIAN_POINT('Ctrl Pts',(82.9129498948689,303.721667776361,53.0228109606482));
#32560=CARTESIAN_POINT('Ctrl Pts',(82.9129498948654,303.544571204362,55.227408420558));
#32561=CARTESIAN_POINT('Ctrl Pts',(81.9432795991037,303.367474632363,57.4147653849927));
#32562=CARTESIAN_POINT('Ctrl Pts',(80.3096882702449,303.190378060364,58.8951806411011));
#32563=CARTESIAN_POINT('Ctrl Pts',(78.6760969413861,303.013281488366,60.3755958972094));
#32564=CARTESIAN_POINT('Ctrl Pts',(76.4041347530316,302.836184916367,61.1259150206703));
#32565=CARTESIAN_POINT('Ctrl Pts',(74.2101800112094,302.659088344368,60.9095529374009));
#32566=CARTESIAN_POINT('Ctrl Pts',(72.0162252693872,302.48199177237,60.6931908541315));
#32567=CARTESIAN_POINT('Ctrl Pts',(69.9345925076876,302.304895200371,59.5135315737617));
#32568=CARTESIAN_POINT('Ctrl Pts',(68.6216467656533,302.127798628372,57.7425365317826));
#32569=CARTESIAN_POINT('Ctrl Pts',(67.3087010236189,301.950702056373,55.9715414898034));
#32570=CARTESIAN_POINT('Ctrl Pts',(66.7849774198229,301.773605484375,53.6369099216174));
#32571=CARTESIAN_POINT('Ctrl Pts',(67.215612605763,301.596508912376,51.4747805783839));
#32572=CARTESIAN_POINT('Ctrl Pts',(67.6462477917031,301.419412340377,49.3126512351505));
#32573=CARTESIAN_POINT('Ctrl Pts',(69.0245064208056,301.242315768378,47.3568408855388));
#32574=CARTESIAN_POINT('Ctrl Pts',(70.9158061804572,301.06521919638,46.2240411771249));
#32575=CARTESIAN_POINT('Ctrl Pts',(72.8071059401089,300.888122624381,45.0912414687111));
#32576=CARTESIAN_POINT('Ctrl Pts',(75.181865969823,300.711026052382,44.7991699473061));
#32577=CARTESIAN_POINT('Ctrl Pts',(77.2912945088786,300.533929480384,45.4399204438793));
#32578=CARTESIAN_POINT('Ctrl Pts',(79.4007230479341,300.356832908385,46.0806709404525));
#32579=CARTESIAN_POINT('Ctrl Pts',(81.2118275942161,300.179736336386,47.6442218014034));
#32580=CARTESIAN_POINT('Ctrl Pts',(82.1535440633152,300.002639764387,49.6375657386275));
#32581=CARTESIAN_POINT('Ctrl Pts',(82.6515697929947,299.908982435045,50.6917435101896));
#32582=CARTESIAN_POINT('Ctrl Pts',(82.9129498948707,299.815325105703,51.8569119935507));
#32583=CARTESIAN_POINT('Ctrl Pts',(82.9129498948689,299.721667776361,53.0228109606478));
#32584=CARTESIAN_POINT('Origin',(74.9879498948689,255.,53.0228109606356));
#32585=CARTESIAN_POINT('',(82.9143689269116,294.278332223638,53.0158045639297));
#32586=CARTESIAN_POINT('',(82.9232745335521,295.721667776361,53.0227066122654));
#32587=CARTESIAN_POINT('',(82.9129498948689,255.,53.0228109606356));
#32588=CARTESIAN_POINT('Ctrl Pts',(82.9143689269116,294.278332223638,53.0158045639297));
#32589=CARTESIAN_POINT('Ctrl Pts',(82.9192260453689,294.322043009225,52.4722564462004));
#32590=CARTESIAN_POINT('Ctrl Pts',(82.867980282346,294.365753794812,51.929638208115));
#32591=CARTESIAN_POINT('Ctrl Pts',(82.7572016326311,294.409464580398,51.399459111527));
#32592=CARTESIAN_POINT('Ctrl Pts',(82.2195229807472,294.621620589951,48.8261655875135));
#32593=CARTESIAN_POINT('Ctrl Pts',(80.2793846172819,294.833776599503,46.5459100088442));
#32594=CARTESIAN_POINT('Ctrl Pts',(77.823092890938,295.045932609055,45.6075313705159));
#32595=CARTESIAN_POINT('Ctrl Pts',(75.3668011645943,295.258088618608,44.6691527321877));
#32596=CARTESIAN_POINT('Ctrl Pts',(72.394356075372,295.47024462816,45.0726510342002));
#32597=CARTESIAN_POINT('Ctrl Pts',(70.2792195264287,295.682400637712,46.6310662904978));
#32598=CARTESIAN_POINT('Ctrl Pts',(68.1640829774853,295.894556647265,48.1894815467954));
#32599=CARTESIAN_POINT('Ctrl Pts',(66.9062549688212,296.106712656817,50.9028137573782));
#32600=CARTESIAN_POINT('Ctrl Pts',(67.0689438525749,296.318868666369,53.5287336404149));
#32601=CARTESIAN_POINT('Ctrl Pts',(67.1502882944518,296.424946671145,54.8416935819331));
#32602=CARTESIAN_POINT('Ctrl Pts',(67.5867619594331,296.531024675921,56.1328004415649));
#32603=CARTESIAN_POINT('Ctrl Pts',(68.2943641356939,296.637102680698,57.2525775592319));
#32604=CARTESIAN_POINT('Ctrl Pts',(69.0019663119547,296.743180685474,58.372354676899));
#32605=CARTESIAN_POINT('Ctrl Pts',(69.9806969994951,296.84925869025,59.3208020526014));
#32606=CARTESIAN_POINT('Ctrl Pts',(71.1316116069641,296.955336695026,59.9578862641231));
#32607=CARTESIAN_POINT('Ctrl Pts',(73.4334408219021,297.167492704579,61.2320546871664));
#32608=CARTESIAN_POINT('Ctrl Pts',(76.4240057165548,297.379648714131,61.2607704534866));
#32609=CARTESIAN_POINT('Ctrl Pts',(78.7394956215055,297.591804723683,60.0194134412586));
#32610=CARTESIAN_POINT('Ctrl Pts',(81.0549855264564,297.803960733235,58.7780564290305));
#32611=CARTESIAN_POINT('Ctrl Pts',(82.6954004417052,298.016116742788,56.2666266382539));
#32612=CARTESIAN_POINT('Ctrl Pts',(82.9022950193089,298.22827275234,53.6453448625695));
#32613=CARTESIAN_POINT('Ctrl Pts',(82.9185676876959,298.244959242773,53.4391758581496));
#32614=CARTESIAN_POINT('Ctrl Pts',(82.925972407017,298.261645733205,53.2323272946183));
#32615=CARTESIAN_POINT('Ctrl Pts',(82.9247849645265,298.278332223638,53.0254077151713));
#32616=CARTESIAN_POINT('Ctrl Pts',(82.9066314816043,299.721667776361,53.0301977459941));
#32617=CARTESIAN_POINT('Ctrl Pts',(82.9139510729998,299.656562102834,53.8410766346259));
#32618=CARTESIAN_POINT('Ctrl Pts',(82.7999589108879,299.591456429307,54.6501502598461));
#32619=CARTESIAN_POINT('Ctrl Pts',(82.5566825623697,299.52635075578,55.4188133435249));
#32620=CARTESIAN_POINT('Ctrl Pts',(81.7639323069155,299.314194746227,57.9236102942205));
#32621=CARTESIAN_POINT('Ctrl Pts',(79.5983468365648,299.102038736675,59.9992981943577));
#32622=CARTESIAN_POINT('Ctrl Pts',(77.0602620358863,298.889882727123,60.6863564585103));
#32623=CARTESIAN_POINT('Ctrl Pts',(74.5221772352076,298.67772671757,61.373414722663));
#32624=CARTESIAN_POINT('Ctrl Pts',(71.6115931042009,298.465570708018,60.6718433508309));
#32625=CARTESIAN_POINT('Ctrl Pts',(69.6623542357921,298.253414698466,58.9079256295904));
#32626=CARTESIAN_POINT('Ctrl Pts',(67.7131153673835,298.041258688913,57.14400790835));
#32627=CARTESIAN_POINT('Ctrl Pts',(66.7252217615726,297.829102679361,54.3177438377017));
#32628=CARTESIAN_POINT('Ctrl Pts',(67.156146985339,297.616946669809,51.7238612333232));
#32629=CARTESIAN_POINT('Ctrl Pts',(67.5870722091055,297.404790660256,49.1299786289446));
#32630=CARTESIAN_POINT('Ctrl Pts',(69.4368162624498,297.192634650704,46.768477490836));
#32631=CARTESIAN_POINT('Ctrl Pts',(71.8502309745856,296.980478641152,45.7302626002747));
#32632=CARTESIAN_POINT('Ctrl Pts',(74.2636456867215,296.7683226316,44.6920477097135));
#32633=CARTESIAN_POINT('Ctrl Pts',(77.240731057649,296.556166622047,44.9771190666996));
#32634=CARTESIAN_POINT('Ctrl Pts',(79.4248119076536,296.344010612495,46.4439911625783));
#32635=CARTESIAN_POINT('Ctrl Pts',(80.5168523326559,296.237932607719,47.1774272105176));
#32636=CARTESIAN_POINT('Ctrl Pts',(81.4106416274275,296.131854602943,48.20631344318));
#32637=CARTESIAN_POINT('Ctrl Pts',(82.0196085258,296.025776598167,49.382647132992));
#32638=CARTESIAN_POINT('Ctrl Pts',(82.6015457092702,295.924406990898,50.5067678628704));
#32639=CARTESIAN_POINT('Ctrl Pts',(82.9233837151354,295.823037383629,51.7655372820001));
#32640=CARTESIAN_POINT('Ctrl Pts',(82.9232745335521,295.721667776361,53.0227066122654));
#32641=CARTESIAN_POINT('Origin',(74.9879498948689,255.,53.0228109606356));
#32642=CARTESIAN_POINT('',(82.9071525502277,290.278332223638,53.0227160994365));
#32643=CARTESIAN_POINT('',(82.9129498948689,291.721667776361,53.0228109606475));
#32644=CARTESIAN_POINT('',(82.9129498948689,255.,53.0228109606356));
#32645=CARTESIAN_POINT('Ctrl Pts',(82.9001557306105,290.278332223638,53.022601611389));
#32646=CARTESIAN_POINT('Ctrl Pts',(82.9013200738902,290.382440285244,51.7218986273144));
#32647=CARTESIAN_POINT('Ctrl Pts',(82.5989606688327,290.48654834685,50.4214083906554));
#32648=CARTESIAN_POINT('Ctrl Pts',(81.9908803767954,290.590656408457,49.2833762609638));
#32649=CARTESIAN_POINT('Ctrl Pts',(80.7517074803303,290.802812418009,46.9642440856787));
#32650=CARTESIAN_POINT('Ctrl Pts',(78.2429341375652,291.014968427562,45.3197693966668));
#32651=CARTESIAN_POINT('Ctrl Pts',(75.6241153631151,291.227124437114,45.1094150329749));
#32652=CARTESIAN_POINT('Ctrl Pts',(73.005296588665,291.439280446666,44.8990606692829));
#32653=CARTESIAN_POINT('Ctrl Pts',(70.27643238253,291.651436456218,46.1228266309109));
#32654=CARTESIAN_POINT('Ctrl Pts',(68.6773734189062,291.86359246577,48.2120689184108));
#32655=CARTESIAN_POINT('Ctrl Pts',(67.8778439370942,291.969670470547,49.2566900621608));
#32656=CARTESIAN_POINT('Ctrl Pts',(67.3607657659101,292.075748475323,50.5176802873789));
#32657=CARTESIAN_POINT('Ctrl Pts',(67.1607345872029,292.181826480099,51.8271035041599));
#32658=CARTESIAN_POINT('Ctrl Pts',(66.9607034084957,292.287904484875,53.1365267209409));
#32659=CARTESIAN_POINT('Ctrl Pts',(67.0777192222654,292.393982489651,54.4943829292848));
#32660=CARTESIAN_POINT('Ctrl Pts',(67.528902926771,292.500060494428,55.7300665421262));
#32661=CARTESIAN_POINT('Ctrl Pts',(68.431270335782,292.71221650398,58.2014337678088));
#32662=CARTESIAN_POINT('Ctrl Pts',(70.6703093077364,292.924372513532,60.1841106114811));
#32663=CARTESIAN_POINT('Ctrl Pts',(73.2324904412851,293.136528523085,60.7652203865009));
#32664=CARTESIAN_POINT('Ctrl Pts',(75.7946715748338,293.348684532637,61.3463301615208));
#32665=CARTESIAN_POINT('Ctrl Pts',(78.6799948699769,293.560840542189,60.5258728678884));
#32666=CARTESIAN_POINT('Ctrl Pts',(80.5550470473972,293.772996551741,58.6824784863933));
#32667=CARTESIAN_POINT('Ctrl Pts',(82.0437797240675,293.941441775707,57.2188811077338));
#32668=CARTESIAN_POINT('Ctrl Pts',(82.8956513862547,294.109886999672,55.1104382612587));
#32669=CARTESIAN_POINT('Ctrl Pts',(82.9143689269116,294.278332223638,53.0158045639297));
#32670=CARTESIAN_POINT('Ctrl Pts',(82.9232745335521,295.721667776361,53.0227066122654));
#32671=CARTESIAN_POINT('Ctrl Pts',(82.9232694623053,295.716959378853,53.0810993899503));
#32672=CARTESIAN_POINT('Ctrl Pts',(82.9225698221323,295.712250981346,53.1394887156031));
#32673=CARTESIAN_POINT('Ctrl Pts',(82.921169415458,295.707542583838,53.1978609362051));
#32674=CARTESIAN_POINT('Ctrl Pts',(82.8580683940824,295.495386574286,55.8280588690849));
#32675=CARTESIAN_POINT('Ctrl Pts',(81.372187322062,295.283230564733,58.4235280798784));
#32676=CARTESIAN_POINT('Ctrl Pts',(79.1311979724809,295.071074555181,59.794814872202));
#32677=CARTESIAN_POINT('Ctrl Pts',(76.8902086228999,294.858918545629,61.1661016645256));
#32678=CARTESIAN_POINT('Ctrl Pts',(73.8941109957582,294.646762536076,61.3132060383795));
#32679=CARTESIAN_POINT('Ctrl Pts',(71.5273403904603,294.434606526524,60.1676404943475));
#32680=CARTESIAN_POINT('Ctrl Pts',(69.1605697851623,294.222450516972,59.0220749503154));
#32681=CARTESIAN_POINT('Ctrl Pts',(67.4231262017078,294.010294507419,56.5838394883976));
#32682=CARTESIAN_POINT('Ctrl Pts',(67.1081058109006,293.798138497867,53.9739161089098));
#32683=CARTESIAN_POINT('Ctrl Pts',(66.7930854200933,293.585982488315,51.363992729422));
#32684=CARTESIAN_POINT('Ctrl Pts',(67.9004882219333,293.373826478763,48.5823814323644));
#32685=CARTESIAN_POINT('Ctrl Pts',(69.9267165549782,293.16167046921,46.9065764746971));
#32686=CARTESIAN_POINT('Ctrl Pts',(71.952944888023,292.949514459658,45.2307715170298));
#32687=CARTESIAN_POINT('Ctrl Pts',(74.8979987522728,292.737358450105,44.6607728987527));
#32688=CARTESIAN_POINT('Ctrl Pts',(77.4009069250342,292.525202440553,45.4594664635574));
#32689=CARTESIAN_POINT('Ctrl Pts',(79.9038150977957,292.313046431001,46.2581600283622));
#32690=CARTESIAN_POINT('Ctrl Pts',(81.9645775790689,292.100890421449,48.4255457762487));
#32691=CARTESIAN_POINT('Ctrl Pts',(82.6516841256833,291.888734411896,50.9651928971345));
#32692=CARTESIAN_POINT('Ctrl Pts',(82.8320428771505,291.833045533384,51.6318254392738));
#32693=CARTESIAN_POINT('Ctrl Pts',(82.9177551992494,291.777356654873,52.324107206126));
#32694=CARTESIAN_POINT('Ctrl Pts',(82.9134059933203,291.721667776361,53.0176571633937));
#32695=CARTESIAN_POINT('Origin',(74.9879498948689,255.,53.0228109606356));
#32696=CARTESIAN_POINT('',(82.9129498948689,286.278332223638,53.0228109606342));
#32697=CARTESIAN_POINT('',(82.9078622521729,287.721667776361,53.0229211557408));
#32698=CARTESIAN_POINT('',(82.9129498948689,255.,53.0228109606356));
#32699=CARTESIAN_POINT('Ctrl Pts',(82.9129498948689,286.278332223638,53.0228109606342));
#32700=CARTESIAN_POINT('Ctrl Pts',(82.9129498948685,286.455428795637,50.8182135007243));
#32701=CARTESIAN_POINT('Ctrl Pts',(81.9432795991099,286.632525367635,48.6308565362883));
#32702=CARTESIAN_POINT('Ctrl Pts',(80.3096882702532,286.809621939634,47.1504412801776));
#32703=CARTESIAN_POINT('Ctrl Pts',(78.6760969413965,286.986718511633,45.670026024067));
#32704=CARTESIAN_POINT('Ctrl Pts',(76.4041347530431,287.163815083632,44.9197069006028));
#32705=CARTESIAN_POINT('Ctrl Pts',(74.2101800112206,287.34091165563,45.1360689838691));
#32706=CARTESIAN_POINT('Ctrl Pts',(72.0162252693981,287.518008227629,45.3524310671354));
#32707=CARTESIAN_POINT('Ctrl Pts',(69.9345925076968,287.695104799628,46.5320903475022));
#32708=CARTESIAN_POINT('Ctrl Pts',(68.6216467656599,287.872201371626,48.3030853894795));
#32709=CARTESIAN_POINT('Ctrl Pts',(67.3087010236231,288.049297943625,50.0740804314568));
#32710=CARTESIAN_POINT('Ctrl Pts',(66.7849774198238,288.226394515624,52.4087119996421));
#32711=CARTESIAN_POINT('Ctrl Pts',(67.2156126057608,288.403491087623,54.5708413428762));
#32712=CARTESIAN_POINT('Ctrl Pts',(67.6462477916978,288.580587659621,56.7329706861103));
#32713=CARTESIAN_POINT('Ctrl Pts',(69.0245064207976,288.75768423162,58.6887810357239));
#32714=CARTESIAN_POINT('Ctrl Pts',(70.9158061804476,288.934780803619,59.8215807441404));
#32715=CARTESIAN_POINT('Ctrl Pts',(72.8071059400976,289.111877375618,60.954380452557));
#32716=CARTESIAN_POINT('Ctrl Pts',(75.1818659698113,289.288973947616,61.2464519739654));
#32717=CARTESIAN_POINT('Ctrl Pts',(77.2912945088678,289.466070519615,60.6057014773951));
#32718=CARTESIAN_POINT('Ctrl Pts',(79.4007230479243,289.643167091614,59.9649509808249));
#32719=CARTESIAN_POINT('Ctrl Pts',(81.2118275942084,289.820263663613,58.4014001198766));
#32720=CARTESIAN_POINT('Ctrl Pts',(82.1535440633104,289.997360235611,56.4080561826538));
#32721=CARTESIAN_POINT('Ctrl Pts',(82.6515697929914,290.091017564953,55.3538784110924));
#32722=CARTESIAN_POINT('Ctrl Pts',(82.9129498948691,290.184674894296,54.1887099277315));
#32723=CARTESIAN_POINT('Ctrl Pts',(82.9129498948689,290.278332223638,53.0228109606343));
#32724=CARTESIAN_POINT('Ctrl Pts',(82.9129498948689,291.721667776361,53.0228109606475));
#32725=CARTESIAN_POINT('Ctrl Pts',(82.9129498948656,291.544571204362,55.2274084205573));
#32726=CARTESIAN_POINT('Ctrl Pts',(81.9432795991041,291.367474632363,57.4147653849921));
#32727=CARTESIAN_POINT('Ctrl Pts',(80.3096882702454,291.190378060365,58.8951806411006));
#32728=CARTESIAN_POINT('Ctrl Pts',(78.6760969413868,291.013281488366,60.3755958972091));
#32729=CARTESIAN_POINT('Ctrl Pts',(76.4041347530324,290.836184916367,61.1259150206702));
#32730=CARTESIAN_POINT('Ctrl Pts',(74.2101800112101,290.659088344368,60.909552937401));
#32731=CARTESIAN_POINT('Ctrl Pts',(72.0162252693879,290.48199177237,60.6931908541318));
#32732=CARTESIAN_POINT('Ctrl Pts',(69.9345925076882,290.304895200371,59.5135315737622));
#32733=CARTESIAN_POINT('Ctrl Pts',(68.6216467656537,290.127798628372,57.7425365317832));
#32734=CARTESIAN_POINT('Ctrl Pts',(67.3087010236192,289.950702056373,55.9715414898041));
#32735=CARTESIAN_POINT('Ctrl Pts',(66.784977419823,289.773605484375,53.6369099216182));
#32736=CARTESIAN_POINT('Ctrl Pts',(67.2156126057629,289.596508912376,51.4747805783847));
#32737=CARTESIAN_POINT('Ctrl Pts',(67.6462477917027,289.419412340377,49.3126512351511));
#32738=CARTESIAN_POINT('Ctrl Pts',(69.0245064208051,289.242315768378,47.3568408855393));
#32739=CARTESIAN_POINT('Ctrl Pts',(70.9158061804566,289.06521919638,46.2240411771253));
#32740=CARTESIAN_POINT('Ctrl Pts',(72.8071059401081,288.888122624381,45.0912414687113));
#32741=CARTESIAN_POINT('Ctrl Pts',(75.1818659698222,288.711026052382,44.799169947306));
#32742=CARTESIAN_POINT('Ctrl Pts',(77.2912945088778,288.533929480384,45.439920443879));
#32743=CARTESIAN_POINT('Ctrl Pts',(79.4007230479335,288.356832908385,46.080670940452));
#32744=CARTESIAN_POINT('Ctrl Pts',(81.2118275942156,288.179736336386,47.6442218014028));
#32745=CARTESIAN_POINT('Ctrl Pts',(82.1535440633149,288.002639764387,49.6375657386269));
#32746=CARTESIAN_POINT('Ctrl Pts',(82.6515697929945,287.908982435045,50.691743510189));
#32747=CARTESIAN_POINT('Ctrl Pts',(82.9129498948707,287.815325105703,51.8569119935502));
#32748=CARTESIAN_POINT('Ctrl Pts',(82.9129498948689,287.721667776361,53.0228109606475));
#32749=CARTESIAN_POINT('Origin',(74.9879498948689,255.,53.0228109606356));
#32750=CARTESIAN_POINT('',(82.9192650697738,282.278332223638,53.0203619272188));
#32751=CARTESIAN_POINT('',(82.9146235913291,283.721667776361,53.0253669122659));
#32752=CARTESIAN_POINT('',(82.9129498948689,255.,53.0228109606356));
#32753=CARTESIAN_POINT('Ctrl Pts',(82.9129498948689,282.278332223638,53.022810960634));
#32754=CARTESIAN_POINT('Ctrl Pts',(82.9129498948684,282.455428795637,50.8182135007241));
#32755=CARTESIAN_POINT('Ctrl Pts',(81.9432795991097,282.632525367635,48.630856536288));
#32756=CARTESIAN_POINT('Ctrl Pts',(80.3096882702529,282.809621939634,47.1504412801773));
#32757=CARTESIAN_POINT('Ctrl Pts',(78.6760969413961,282.986718511633,45.6700260240667));
#32758=CARTESIAN_POINT('Ctrl Pts',(76.4041347530426,283.163815083632,44.9197069006027));
#32759=CARTESIAN_POINT('Ctrl Pts',(74.21018001122,283.34091165563,45.1360689838692));
#32760=CARTESIAN_POINT('Ctrl Pts',(72.0162252693974,283.518008227629,45.3524310671357));
#32761=CARTESIAN_POINT('Ctrl Pts',(69.9345925076962,283.695104799628,46.5320903475027));
#32762=CARTESIAN_POINT('Ctrl Pts',(68.6216467656594,283.872201371627,48.3030853894802));
#32763=CARTESIAN_POINT('Ctrl Pts',(67.3087010236227,284.049297943625,50.0740804314577));
#32764=CARTESIAN_POINT('Ctrl Pts',(66.7849774198237,284.226394515624,52.4087119996431));
#32765=CARTESIAN_POINT('Ctrl Pts',(67.215612605761,284.403491087623,54.5708413428772));
#32766=CARTESIAN_POINT('Ctrl Pts',(67.6462477916984,284.580587659622,56.7329706861113));
#32767=CARTESIAN_POINT('Ctrl Pts',(69.0245064207984,284.75768423162,58.6887810357248));
#32768=CARTESIAN_POINT('Ctrl Pts',(70.9158061804487,284.934780803619,59.8215807441411));
#32769=CARTESIAN_POINT('Ctrl Pts',(72.807105940099,285.111877375618,60.9543804525574));
#32770=CARTESIAN_POINT('Ctrl Pts',(75.1818659698128,285.288973947616,61.2464519739653));
#32771=CARTESIAN_POINT('Ctrl Pts',(77.2912945088692,285.466070519615,60.6057014773947));
#32772=CARTESIAN_POINT('Ctrl Pts',(79.4007230479257,285.643167091614,59.9649509808241));
#32773=CARTESIAN_POINT('Ctrl Pts',(81.2118275942096,285.820263663613,58.4014001198753));
#32774=CARTESIAN_POINT('Ctrl Pts',(82.1535440633112,285.997360235611,56.4080561826522));
#32775=CARTESIAN_POINT('Ctrl Pts',(82.6515697929917,286.091017564954,55.3538784110912));
#32776=CARTESIAN_POINT('Ctrl Pts',(82.9129498948691,286.184674894296,54.1887099277309));
#32777=CARTESIAN_POINT('Ctrl Pts',(82.9129498948689,286.278332223638,53.0228109606342));
#32778=CARTESIAN_POINT('Ctrl Pts',(82.8973468488884,287.721667776361,53.0231489126204));
#32779=CARTESIAN_POINT('Ctrl Pts',(82.8989520065444,287.62559792134,54.2230004198988));
#32780=CARTESIAN_POINT('Ctrl Pts',(82.6424763919888,287.529528066319,55.4223533881397));
#32781=CARTESIAN_POINT('Ctrl Pts',(82.1232866064541,287.433458211298,56.49463821269));
#32782=CARTESIAN_POINT('Ctrl Pts',(81.5500098326146,287.327380206522,57.6786291192565));
#32783=CARTESIAN_POINT('Ctrl Pts',(80.6564308644769,287.221302201745,58.7076980240982));
#32784=CARTESIAN_POINT('Ctrl Pts',(79.5769703194514,287.115224196969,59.4754001569812));
#32785=CARTESIAN_POINT('Ctrl Pts',(78.497509774426,287.009146192193,60.2431022898643));
#32786=CARTESIAN_POINT('Ctrl Pts',(77.2321676525127,286.903068187417,60.7494376507887));
#32787=CARTESIAN_POINT('Ctrl Pts',(75.9256098672663,286.796990182641,60.9023673080429));
#32788=CARTESIAN_POINT('Ctrl Pts',(73.3124942967733,286.584834173088,61.2082266225512));
#32789=CARTESIAN_POINT('Ctrl Pts',(70.5345160729474,286.372678163536,60.1004631223783));
#32790=CARTESIAN_POINT('Ctrl Pts',(68.8629096503185,286.160522153984,58.0735954159003));
#32791=CARTESIAN_POINT('Ctrl Pts',(67.1913032276897,285.948366144431,56.0467277094226));
#32792=CARTESIAN_POINT('Ctrl Pts',(66.6260686062576,285.736210134879,53.10075579664));
#32793=CARTESIAN_POINT('Ctrl Pts',(67.4288976409122,285.524054125327,50.5968809884894));
#32794=CARTESIAN_POINT('Ctrl Pts',(68.2317266755669,285.311898115775,48.0930061803387));
#32795=CARTESIAN_POINT('Ctrl Pts',(70.4026193663083,285.099742106222,46.0312284768201));
#32796=CARTESIAN_POINT('Ctrl Pts',(72.9427072516828,284.88758609667,45.3538132216075));
#32797=CARTESIAN_POINT('Ctrl Pts',(75.4827951370574,284.675430087118,44.6763979663949));
#32798=CARTESIAN_POINT('Ctrl Pts',(78.3920782170651,284.463274077565,45.3833451594885));
#32799=CARTESIAN_POINT('Ctrl Pts',(80.335126355604,284.251118068013,47.1549228306892));
#32800=CARTESIAN_POINT('Ctrl Pts',(81.9514642662677,284.074634637462,48.6286218579301));
#32801=CARTESIAN_POINT('Ctrl Pts',(82.8991812941406,283.898151206912,50.8390300845257));
#32802=CARTESIAN_POINT('Ctrl Pts',(82.9187310422535,283.721667776361,53.0316395226755));
#32803=CARTESIAN_POINT('Origin',(74.9879498948689,255.,53.0228109606356));
#32804=CARTESIAN_POINT('',(82.909752682909,278.278332223638,53.0216597493918));
#32805=CARTESIAN_POINT('',(82.9157046094419,279.721667776361,53.0210340633603));
#32806=CARTESIAN_POINT('',(82.9129498948689,255.,53.0228109606356));
#32807=CARTESIAN_POINT('Ctrl Pts',(82.9009419360392,278.278332223638,53.0184872882153));
#32808=CARTESIAN_POINT('Ctrl Pts',(82.9066125316817,278.35147610375,52.1059266595105));
#32809=CARTESIAN_POINT('Ctrl Pts',(82.7609970955639,278.424619983862,51.1948597659628));
#32810=CARTESIAN_POINT('Ctrl Pts',(82.4560394698546,278.497763863975,50.340600574444));
#32811=CARTESIAN_POINT('Ctrl Pts',(82.0137701176292,278.603841868751,49.1016984207862));
#32812=CARTESIAN_POINT('Ctrl Pts',(81.2363613746537,278.709919873527,47.9822781111815));
#32813=CARTESIAN_POINT('Ctrl Pts',(80.2459726342748,278.815997878304,47.1026578658311));
#32814=CARTESIAN_POINT('Ctrl Pts',(79.2555838938957,278.92207588308,46.2230376204805));
#32815=CARTESIAN_POINT('Ctrl Pts',(78.0522151561131,279.028153887856,45.5832174393843));
#32816=CARTESIAN_POINT('Ctrl Pts',(76.7697647029933,279.134231892632,45.2902984035587));
#32817=CARTESIAN_POINT('Ctrl Pts',(74.204863796754,279.346387902184,44.7044603319075));
#32818=CARTESIAN_POINT('Ctrl Pts',(71.3236360291661,279.558543911736,45.5062268413383));
#32819=CARTESIAN_POINT('Ctrl Pts',(69.4432262686172,279.770699921289,47.3410346961746));
#32820=CARTESIAN_POINT('Ctrl Pts',(67.5628165080682,279.982855930841,49.1758425510109));
#32821=CARTESIAN_POINT('Ctrl Pts',(66.6832247545584,280.195011940393,52.0436917512528));
#32822=CARTESIAN_POINT('Ctrl Pts',(67.2113901299962,280.407167949946,54.6195343027231));
#32823=CARTESIAN_POINT('Ctrl Pts',(67.739555505434,280.619323959498,57.1953768541933));
#32824=CARTESIAN_POINT('Ctrl Pts',(69.6754780098195,280.83147996905,59.4792127568922));
#32825=CARTESIAN_POINT('Ctrl Pts',(72.1277135814771,281.043635978603,60.4265662255183));
#32826=CARTESIAN_POINT('Ctrl Pts',(74.5799491531347,281.255791988155,61.3739196941445));
#32827=CARTESIAN_POINT('Ctrl Pts',(77.5484977920643,281.467947997707,60.9847907286983));
#32828=CARTESIAN_POINT('Ctrl Pts',(79.6712397802176,281.68010400726,59.4330530042401));
#32829=CARTESIAN_POINT('Ctrl Pts',(81.6664447178233,281.879513412719,57.9745456646827));
#32830=CARTESIAN_POINT('Ctrl Pts',(82.9144241339818,282.078922818178,55.4889348666762));
#32831=CARTESIAN_POINT('Ctrl Pts',(82.9255991990642,282.278332223638,53.0179055432671));
#32832=CARTESIAN_POINT('Ctrl Pts',(82.9129498948689,283.721667776361,53.0228109606471));
#32833=CARTESIAN_POINT('Ctrl Pts',(82.9129498948657,283.544571204362,55.227408420557));
#32834=CARTESIAN_POINT('Ctrl Pts',(81.9432795991042,283.367474632363,57.414765384992));
#32835=CARTESIAN_POINT('Ctrl Pts',(80.3096882702455,283.190378060365,58.8951806411005));
#32836=CARTESIAN_POINT('Ctrl Pts',(78.6760969413868,283.013281488366,60.3755958972091));
#32837=CARTESIAN_POINT('Ctrl Pts',(76.4041347530324,282.836184916367,61.1259150206702));
#32838=CARTESIAN_POINT('Ctrl Pts',(74.21018001121,282.659088344368,60.909552937401));
#32839=CARTESIAN_POINT('Ctrl Pts',(72.0162252693877,282.48199177237,60.6931908541317));
#32840=CARTESIAN_POINT('Ctrl Pts',(69.934592507688,282.304895200371,59.513531573762));
#32841=CARTESIAN_POINT('Ctrl Pts',(68.6216467656535,282.127798628372,57.7425365317829));
#32842=CARTESIAN_POINT('Ctrl Pts',(67.308701023619,281.950702056373,55.9715414898037));
#32843=CARTESIAN_POINT('Ctrl Pts',(66.7849774198229,281.773605484375,53.6369099216177));
#32844=CARTESIAN_POINT('Ctrl Pts',(67.215612605763,281.596508912376,51.4747805783841));
#32845=CARTESIAN_POINT('Ctrl Pts',(67.646247791703,281.419412340377,49.3126512351505));
#32846=CARTESIAN_POINT('Ctrl Pts',(69.0245064208056,281.242315768378,47.3568408855388));
#32847=CARTESIAN_POINT('Ctrl Pts',(70.9158061804573,281.06521919638,46.2240411771249));
#32848=CARTESIAN_POINT('Ctrl Pts',(72.807105940109,280.888122624381,45.091241468711));
#32849=CARTESIAN_POINT('Ctrl Pts',(75.1818659698232,280.711026052382,44.799169947306));
#32850=CARTESIAN_POINT('Ctrl Pts',(77.2912945088788,280.533929480384,45.4399204438793));
#32851=CARTESIAN_POINT('Ctrl Pts',(79.4007230479344,280.356832908385,46.0806709404526));
#32852=CARTESIAN_POINT('Ctrl Pts',(81.2118275942164,280.179736336386,47.6442218014037));
#32853=CARTESIAN_POINT('Ctrl Pts',(82.1535440633154,280.002639764387,49.637565738628));
#32854=CARTESIAN_POINT('Ctrl Pts',(82.6515697929947,279.908982435045,50.6917435101897));
#32855=CARTESIAN_POINT('Ctrl Pts',(82.9129498948706,279.815325105703,51.8569119935504));
#32856=CARTESIAN_POINT('Ctrl Pts',(82.9129498948689,279.721667776361,53.0228109606472));
#32857=CARTESIAN_POINT('Origin',(74.9879498948689,255.,53.0228109606356));
#32858=CARTESIAN_POINT('',(82.9129498948689,274.278332223638,53.0228109606336));
#32859=CARTESIAN_POINT('',(82.9018331595289,275.721667776361,53.0187249907903));
#32860=CARTESIAN_POINT('',(82.9129498948689,255.,53.0228109606356));
#32861=CARTESIAN_POINT('Ctrl Pts',(82.9129498948689,274.278332223638,53.0228109606334));
#32862=CARTESIAN_POINT('Ctrl Pts',(82.9129498948683,274.455428795637,50.8182135007235));
#32863=CARTESIAN_POINT('Ctrl Pts',(81.9432795991094,274.632525367635,48.6308565362875));
#32864=CARTESIAN_POINT('Ctrl Pts',(80.3096882702525,274.809621939634,47.150441280177));
#32865=CARTESIAN_POINT('Ctrl Pts',(78.6760969413956,274.986718511633,45.6700260240665));
#32866=CARTESIAN_POINT('Ctrl Pts',(76.404134753042,275.163815083632,44.9197069006026));
#32867=CARTESIAN_POINT('Ctrl Pts',(74.2101800112194,275.34091165563,45.1360689838693));
#32868=CARTESIAN_POINT('Ctrl Pts',(72.0162252693968,275.518008227629,45.3524310671359));
#32869=CARTESIAN_POINT('Ctrl Pts',(69.9345925076957,275.695104799628,46.5320903475031));
#32870=CARTESIAN_POINT('Ctrl Pts',(68.6216467656591,275.872201371627,48.3030853894807));
#32871=CARTESIAN_POINT('Ctrl Pts',(67.3087010236225,276.049297943625,50.0740804314583));
#32872=CARTESIAN_POINT('Ctrl Pts',(66.7849774198237,276.226394515624,52.4087119996437));
#32873=CARTESIAN_POINT('Ctrl Pts',(67.2156126057612,276.403491087623,54.5708413428778));
#32874=CARTESIAN_POINT('Ctrl Pts',(67.6462477916986,276.580587659622,56.7329706861119));
#32875=CARTESIAN_POINT('Ctrl Pts',(69.0245064207988,276.75768423162,58.6887810357253));
#32876=CARTESIAN_POINT('Ctrl Pts',(70.9158061804492,276.934780803619,59.8215807441414));
#32877=CARTESIAN_POINT('Ctrl Pts',(72.8071059400995,277.111877375618,60.9543804525575));
#32878=CARTESIAN_POINT('Ctrl Pts',(75.1818659698134,277.288973947617,61.2464519739653));
#32879=CARTESIAN_POINT('Ctrl Pts',(77.2912945088698,277.466070519615,60.6057014773945));
#32880=CARTESIAN_POINT('Ctrl Pts',(79.4007230479262,277.643167091614,59.9649509808237));
#32881=CARTESIAN_POINT('Ctrl Pts',(81.21182759421,277.820263663613,58.4014001198748));
#32882=CARTESIAN_POINT('Ctrl Pts',(82.1535440633114,277.997360235611,56.4080561826517));
#32883=CARTESIAN_POINT('Ctrl Pts',(82.6515697929918,278.091017564954,55.3538784110907));
#32884=CARTESIAN_POINT('Ctrl Pts',(82.9129498948692,278.184674894296,54.1887099277304));
#32885=CARTESIAN_POINT('Ctrl Pts',(82.9129498948689,278.278332223638,53.0228109606338));
#32886=CARTESIAN_POINT('Ctrl Pts',(82.9221926362458,279.721667776361,53.01684903544));
#32887=CARTESIAN_POINT('Ctrl Pts',(82.9041921061136,279.534236463826,55.343761083048));
#32888=CARTESIAN_POINT('Ctrl Pts',(81.8191527316485,279.346805151292,57.6866115007869));
#32889=CARTESIAN_POINT('Ctrl Pts',(80.0249961549487,279.159373838757,59.1591540560566));
#32890=CARTESIAN_POINT('Ctrl Pts',(77.9941663289309,278.947217829205,60.825944669629));
#32891=CARTESIAN_POINT('Ctrl Pts',(75.0547957671856,278.735061819653,61.3776725782135));
#32892=CARTESIAN_POINT('Ctrl Pts',(72.5495833248604,278.5229058101,60.574034896268));
#32893=CARTESIAN_POINT('Ctrl Pts',(71.2969771036978,278.416827805324,60.1722160552952));
#32894=CARTESIAN_POINT('Ctrl Pts',(70.1529104123901,278.310749800548,59.43155581669));
#32895=CARTESIAN_POINT('Ctrl Pts',(69.2416036151328,278.204671795772,58.4702434042181));
#32896=CARTESIAN_POINT('Ctrl Pts',(68.3302968178754,278.098593790996,57.5089309917462));
#32897=CARTESIAN_POINT('Ctrl Pts',(67.6517499146684,277.99251578622,56.3269664054077));
#32898=CARTESIAN_POINT('Ctrl Pts',(67.3173541659037,277.886437781444,55.0547006275673));
#32899=CARTESIAN_POINT('Ctrl Pts',(66.6485626683742,277.674281771891,52.5101690718864));
#32900=CARTESIAN_POINT('Ctrl Pts',(67.3563757886142,277.462125762339,49.6044327501977));
#32901=CARTESIAN_POINT('Ctrl Pts',(69.1291745043439,277.249969752787,47.6654522332136));
#32902=CARTESIAN_POINT('Ctrl Pts',(70.9019732200736,277.037813743234,45.7264717162295));
#32903=CARTESIAN_POINT('Ctrl Pts',(73.7397575312933,276.825657733682,44.75424700395));
#32904=CARTESIAN_POINT('Ctrl Pts',(76.3313879059252,276.613501724129,45.1985166462418));
#32905=CARTESIAN_POINT('Ctrl Pts',(78.9230182805569,276.401345714577,45.6427862885337));
#32906=CARTESIAN_POINT('Ctrl Pts',(81.2684947186008,276.189189705025,47.5035502853966));
#32907=CARTESIAN_POINT('Ctrl Pts',(82.2949537237807,275.977033695473,49.9237403201058));
#32908=CARTESIAN_POINT('Ctrl Pts',(82.7067931807312,275.891911722436,50.8947773947302));
#32909=CARTESIAN_POINT('Ctrl Pts',(82.9062968379203,275.806789749398,51.9558710313029));
#32910=CARTESIAN_POINT('Ctrl Pts',(82.9018331595289,275.721667776361,53.0187249907903));
#32911=CARTESIAN_POINT('Origin',(74.9879498948689,255.,53.0228109606356));
#32912=CARTESIAN_POINT('',(82.913981855057,270.278332223638,53.0234548561531));
#32913=CARTESIAN_POINT('',(82.9063872485843,271.721667776361,53.029301811537));
#32914=CARTESIAN_POINT('',(82.9129498948689,255.,53.0228109606356));
#32915=CARTESIAN_POINT('Ctrl Pts',(82.9196569564088,270.278332223638,53.0269958574522));
#32916=CARTESIAN_POINT('Ctrl Pts',(82.9025226301854,270.472270655789,50.6202397052844));
#32917=CARTESIAN_POINT('Ctrl Pts',(81.7386913771929,270.66620908794,48.2041551979614));
#32918=CARTESIAN_POINT('Ctrl Pts',(79.8372404750172,270.860147520091,46.7370395298412));
#32919=CARTESIAN_POINT('Ctrl Pts',(77.7571770688595,271.072303529644,45.1321105725038));
#32920=CARTESIAN_POINT('Ctrl Pts',(74.7944090565747,271.284459539196,44.6628064136153));
#32921=CARTESIAN_POINT('Ctrl Pts',(72.3179154280297,271.496615548749,45.5464934744867));
#32922=CARTESIAN_POINT('Ctrl Pts',(69.8414217994845,271.708771558301,46.4301805353582));
#32923=CARTESIAN_POINT('Ctrl Pts',(67.8512025546794,271.920927567853,48.6668588159898));
#32924=CARTESIAN_POINT('Ctrl Pts',(67.2566010192954,272.133083577405,51.2275983395534));
#32925=CARTESIAN_POINT('Ctrl Pts',(66.6619994839114,272.345239586957,53.7883378631168));
#32926=CARTESIAN_POINT('Ctrl Pts',(67.4630156579487,272.55739559651,56.6731386296124));
#32927=CARTESIAN_POINT('Ctrl Pts',(69.296735155505,272.769551606062,58.5576535056635));
#32928=CARTESIAN_POINT('Ctrl Pts',(71.1304546530613,272.981707615615,60.4421683817145));
#32929=CARTESIAN_POINT('Ctrl Pts',(73.9968774741368,273.193863625167,61.3263973673213));
#32930=CARTESIAN_POINT('Ctrl Pts',(76.5713131144536,273.406019634719,60.8022391225105));
#32931=CARTESIAN_POINT('Ctrl Pts',(79.1457487547705,273.618175644271,60.2780808776997));
#32932=CARTESIAN_POINT('Ctrl Pts',(81.4281972143287,273.830331653824,58.3455354024713));
#32933=CARTESIAN_POINT('Ctrl Pts',(82.3851379460284,274.042487663376,55.8947829994249));
#32934=CARTESIAN_POINT('Ctrl Pts',(82.7397343372101,274.121102516797,54.986651566607));
#32935=CARTESIAN_POINT('Ctrl Pts',(82.9123267816282,274.199717370217,54.0073657345194));
#32936=CARTESIAN_POINT('Ctrl Pts',(82.9083427687154,274.278332223638,53.0265063581188));
#32937=CARTESIAN_POINT('Ctrl Pts',(82.9018331595289,275.721667776361,53.0187249907903));
#32938=CARTESIAN_POINT('Ctrl Pts',(82.8951716705674,275.594633739846,54.6049033168082));
#32939=CARTESIAN_POINT('Ctrl Pts',(82.4342366264749,275.467599703331,56.1950022124917));
#32940=CARTESIAN_POINT('Ctrl Pts',(81.5468431519361,275.340565666816,57.4955423912273));
#32941=CARTESIAN_POINT('Ctrl Pts',(80.0648320025961,275.128409657263,59.6675383550835));
#32942=CARTESIAN_POINT('Ctrl Pts',(77.3933681316007,274.916253647711,61.0319142102403));
#32943=CARTESIAN_POINT('Ctrl Pts',(74.7671359794171,274.704097638159,60.9586652199859));
#32944=CARTESIAN_POINT('Ctrl Pts',(72.1409038272333,274.491941628607,60.8854162297315));
#32945=CARTESIAN_POINT('Ctrl Pts',(69.5599033938615,274.279785619055,59.3745423940656));
#32946=CARTESIAN_POINT('Ctrl Pts',(68.1954420945736,274.067629609502,57.1250606164622));
#32947=CARTESIAN_POINT('Ctrl Pts',(67.5132114449297,273.961551604726,56.0003197276606));
#32948=CARTESIAN_POINT('Ctrl Pts',(67.1351155788067,273.855473599949,54.6909268533747));
#32949=CARTESIAN_POINT('Ctrl Pts',(67.0774405885565,273.749395595173,53.3675692945118));
#32950=CARTESIAN_POINT('Ctrl Pts',(67.0197655983062,273.643317590397,52.0442117356488));
#32951=CARTESIAN_POINT('Ctrl Pts',(67.2825114839288,273.537239585621,50.7068894922089));
#32952=CARTESIAN_POINT('Ctrl Pts',(67.8643035947425,273.431161580845,49.5270595612226));
#32953=CARTESIAN_POINT('Ctrl Pts',(69.0278878163698,273.219005571293,47.1673996992501));
#32954=CARTESIAN_POINT('Ctrl Pts',(71.4676569387615,273.00684956174,45.437709087092));
#32955=CARTESIAN_POINT('Ctrl Pts',(74.0775587598043,272.794693552188,45.1362572397698));
#32956=CARTESIAN_POINT('Ctrl Pts',(76.687460580847,272.582537542635,44.8348053924476));
#32957=CARTESIAN_POINT('Ctrl Pts',(79.4674951005409,272.370381533084,45.9615923099614));
#32958=CARTESIAN_POINT('Ctrl Pts',(81.1328493245277,272.158225523531,47.9964187945602));
#32959=CARTESIAN_POINT('Ctrl Pts',(82.2751271068042,272.012706274475,49.3921201118334));
#32960=CARTESIAN_POINT('Ctrl Pts',(82.8929833295828,271.867187025418,51.2150251104585));
#32961=CARTESIAN_POINT('Ctrl Pts',(82.9063872485843,271.721667776361,53.029301811537));
#32962=CARTESIAN_POINT('Origin',(74.9879498948689,255.,53.0228109606356));
#32963=CARTESIAN_POINT('',(82.9129498948689,266.278332223638,53.0228109606333));
#32964=CARTESIAN_POINT('',(82.918336458848,267.721667776361,53.0238104703768));
#32965=CARTESIAN_POINT('',(82.9129498948689,255.,53.0228109606356));
#32966=CARTESIAN_POINT('Ctrl Pts',(82.9129498948689,266.278332223638,53.0228109606331));
#32967=CARTESIAN_POINT('Ctrl Pts',(82.9129498948682,266.455428795637,50.8182135007232));
#32968=CARTESIAN_POINT('Ctrl Pts',(81.9432795991092,266.632525367635,48.6308565362872));
#32969=CARTESIAN_POINT('Ctrl Pts',(80.3096882702523,266.809621939634,47.1504412801767));
#32970=CARTESIAN_POINT('Ctrl Pts',(78.6760969413953,266.986718511633,45.6700260240663));
#32971=CARTESIAN_POINT('Ctrl Pts',(76.4041347530416,267.163815083632,44.9197069006026));
#32972=CARTESIAN_POINT('Ctrl Pts',(74.2101800112191,267.34091165563,45.1360689838693));
#32973=CARTESIAN_POINT('Ctrl Pts',(72.0162252693965,267.518008227629,45.352431067136));
#32974=CARTESIAN_POINT('Ctrl Pts',(69.9345925076954,267.695104799628,46.5320903475033));
#32975=CARTESIAN_POINT('Ctrl Pts',(68.6216467656589,267.872201371627,48.303085389481));
#32976=CARTESIAN_POINT('Ctrl Pts',(67.3087010236224,268.049297943625,50.0740804314586));
#32977=CARTESIAN_POINT('Ctrl Pts',(66.7849774198236,268.226394515624,52.4087119996441));
#32978=CARTESIAN_POINT('Ctrl Pts',(67.2156126057612,268.403491087623,54.5708413428781));
#32979=CARTESIAN_POINT('Ctrl Pts',(67.6462477916988,268.580587659622,56.7329706861122));
#32980=CARTESIAN_POINT('Ctrl Pts',(69.0245064207991,268.75768423162,58.6887810357255));
#32981=CARTESIAN_POINT('Ctrl Pts',(70.9158061804495,268.934780803619,59.8215807441416));
#32982=CARTESIAN_POINT('Ctrl Pts',(72.8071059400999,269.111877375618,60.9543804525576));
#32983=CARTESIAN_POINT('Ctrl Pts',(75.1818659698138,269.288973947617,61.2464519739653));
#32984=CARTESIAN_POINT('Ctrl Pts',(77.2912945088701,269.466070519615,60.6057014773944));
#32985=CARTESIAN_POINT('Ctrl Pts',(79.4007230479265,269.643167091614,59.9649509808236));
#32986=CARTESIAN_POINT('Ctrl Pts',(81.2118275942102,269.820263663613,58.4014001198745));
#32987=CARTESIAN_POINT('Ctrl Pts',(82.1535440633116,269.997360235611,56.4080561826513));
#32988=CARTESIAN_POINT('Ctrl Pts',(82.6515697929919,270.091017564954,55.3538784110904));
#32989=CARTESIAN_POINT('Ctrl Pts',(82.9129498948692,270.184674894296,54.1887099277301));
#32990=CARTESIAN_POINT('Ctrl Pts',(82.9129498948689,270.278332223638,53.0228109606335));
#32991=CARTESIAN_POINT('Ctrl Pts',(82.9063872485843,271.721667776361,53.029301811537));
#32992=CARTESIAN_POINT('Ctrl Pts',(82.9125252251475,271.655031015865,53.8601027041073));
#32993=CARTESIAN_POINT('Ctrl Pts',(82.7919129299211,271.588394255369,54.6890942908775));
#32994=CARTESIAN_POINT('Ctrl Pts',(82.5368654818679,271.521757494874,55.4744261937191));
#32995=CARTESIAN_POINT('Ctrl Pts',(81.7248534869414,271.309601485321,57.9747410565947));
#32996=CARTESIAN_POINT('Ctrl Pts',(79.5501555688087,271.097445475769,60.0325047306618));
#32997=CARTESIAN_POINT('Ctrl Pts',(77.0070028977421,270.885289466217,60.7005601216458));
#32998=CARTESIAN_POINT('Ctrl Pts',(74.4638502266754,270.673133456665,61.3686155126298));
#32999=CARTESIAN_POINT('Ctrl Pts',(71.5522428026749,270.460977447112,60.6469626205306));
#33000=CARTESIAN_POINT('Ctrl Pts',(69.6174757739374,270.24882143756,58.8695664136463));
#33001=CARTESIAN_POINT('Ctrl Pts',(67.6827087451997,270.036665428008,57.092170206762));
#33002=CARTESIAN_POINT('Ctrl Pts',(66.7247821117251,269.824509418456,54.2590306850926));
#33003=CARTESIAN_POINT('Ctrl Pts',(67.1696651073972,269.612353408903,51.6659626132545));
#33004=CARTESIAN_POINT('Ctrl Pts',(67.3921066052332,269.506275404127,50.3694285773356));
#33005=CARTESIAN_POINT('Ctrl Pts',(67.9652505103558,269.400197399351,49.1329124038745));
#33006=CARTESIAN_POINT('Ctrl Pts',(68.7894683730937,269.294119394575,48.0959618033907));
#33007=CARTESIAN_POINT('Ctrl Pts',(69.6136862358316,269.188041389799,47.0590112029069));
#33008=CARTESIAN_POINT('Ctrl Pts',(70.6889780561849,269.081963385022,46.2216261754004));
#33009=CARTESIAN_POINT('Ctrl Pts',(71.9018768584006,268.975885380246,45.7123549099239));
#33010=CARTESIAN_POINT('Ctrl Pts',(74.3276744628317,268.763729370694,44.693812378971));
#33011=CARTESIAN_POINT('Ctrl Pts',(77.3038999947122,268.551573361142,44.9877248961376));
#33012=CARTESIAN_POINT('Ctrl Pts',(79.4720394188731,268.339417351589,46.4715146956494));
#33013=CARTESIAN_POINT('Ctrl Pts',(81.5764141054351,268.133500826513,47.9116664033652));
#33014=CARTESIAN_POINT('Ctrl Pts',(82.9195351808777,267.927584301437,50.4727362525033));
#33015=CARTESIAN_POINT('Ctrl Pts',(82.9263548363187,267.721667776361,53.0252983291183));
#33016=CARTESIAN_POINT('Origin',(74.9879498948689,255.,53.0228109606356));
#33017=CARTESIAN_POINT('',(82.9129498948689,262.278332223638,53.0228109606331));
#33018=CARTESIAN_POINT('',(82.9129498948689,263.721667776361,53.0228109606465));
#33019=CARTESIAN_POINT('',(82.9129498948689,255.,53.0228109606356));
#33020=CARTESIAN_POINT('Ctrl Pts',(82.9129498948689,262.278332223638,53.0228109606331));
#33021=CARTESIAN_POINT('Ctrl Pts',(82.9129498948682,262.455428795637,50.8182135007233));
#33022=CARTESIAN_POINT('Ctrl Pts',(81.9432795991093,262.632525367635,48.6308565362874));
#33023=CARTESIAN_POINT('Ctrl Pts',(80.3096882702525,262.809621939634,47.1504412801769));
#33024=CARTESIAN_POINT('Ctrl Pts',(78.6760969413956,262.986718511633,45.6700260240665));
#33025=CARTESIAN_POINT('Ctrl Pts',(76.4041347530421,263.163815083632,44.9197069006027));
#33026=CARTESIAN_POINT('Ctrl Pts',(74.2101800112196,263.34091165563,45.1360689838692));
#33027=CARTESIAN_POINT('Ctrl Pts',(72.0162252693971,263.518008227629,45.3524310671358));
#33028=CARTESIAN_POINT('Ctrl Pts',(69.934592507696,263.695104799628,46.5320903475029));
#33029=CARTESIAN_POINT('Ctrl Pts',(68.6216467656593,263.872201371627,48.3030853894804));
#33030=CARTESIAN_POINT('Ctrl Pts',(67.3087010236227,264.049297943625,50.0740804314578));
#33031=CARTESIAN_POINT('Ctrl Pts',(66.7849774198237,264.226394515624,52.4087119996432));
#33032=CARTESIAN_POINT('Ctrl Pts',(67.215612605761,264.403491087623,54.5708413428772));
#33033=CARTESIAN_POINT('Ctrl Pts',(67.6462477916983,264.580587659622,56.7329706861112));
#33034=CARTESIAN_POINT('Ctrl Pts',(69.0245064207983,264.75768423162,58.6887810357247));
#33035=CARTESIAN_POINT('Ctrl Pts',(70.9158061804485,264.934780803619,59.821580744141));
#33036=CARTESIAN_POINT('Ctrl Pts',(72.8071059400987,265.111877375618,60.9543804525573));
#33037=CARTESIAN_POINT('Ctrl Pts',(75.1818659698124,265.288973947616,61.2464519739653));
#33038=CARTESIAN_POINT('Ctrl Pts',(77.2912945088688,265.466070519615,60.6057014773948));
#33039=CARTESIAN_POINT('Ctrl Pts',(79.4007230479252,265.643167091614,59.9649509808244));
#33040=CARTESIAN_POINT('Ctrl Pts',(81.2118275942092,265.820263663613,58.4014001198758));
#33041=CARTESIAN_POINT('Ctrl Pts',(82.1535440633109,265.997360235611,56.4080561826528));
#33042=CARTESIAN_POINT('Ctrl Pts',(82.6515697929918,266.091017564954,55.3538784110913));
#33043=CARTESIAN_POINT('Ctrl Pts',(82.9129498948693,266.184674894296,54.1887099277304));
#33044=CARTESIAN_POINT('Ctrl Pts',(82.9129498948689,266.278332223638,53.0228109606331));
#33045=CARTESIAN_POINT('Ctrl Pts',(82.9129498948689,267.721667776361,53.0228109606465));
#33046=CARTESIAN_POINT('Ctrl Pts',(82.9129498948659,267.544571204362,55.2274084205561));
#33047=CARTESIAN_POINT('Ctrl Pts',(81.9432795991048,267.367474632363,57.4147653849909));
#33048=CARTESIAN_POINT('Ctrl Pts',(80.3096882702465,267.190378060365,58.8951806410996));
#33049=CARTESIAN_POINT('Ctrl Pts',(78.6760969413883,267.013281488366,60.3755958972083));
#33050=CARTESIAN_POINT('Ctrl Pts',(76.4041347530342,266.836184916367,61.1259150206698));
#33051=CARTESIAN_POINT('Ctrl Pts',(74.2101800112121,266.659088344368,60.9095529374012));
#33052=CARTESIAN_POINT('Ctrl Pts',(72.0162252693899,266.48199177237,60.6931908541325));
#33053=CARTESIAN_POINT('Ctrl Pts',(69.9345925076901,266.304895200371,59.5135315737636));
#33054=CARTESIAN_POINT('Ctrl Pts',(68.6216467656551,266.127798628372,57.7425365317851));
#33055=CARTESIAN_POINT('Ctrl Pts',(67.3087010236202,265.950702056374,55.9715414898065));
#33056=CARTESIAN_POINT('Ctrl Pts',(66.7849774198232,265.773605484375,53.6369099216209));
#33057=CARTESIAN_POINT('Ctrl Pts',(67.2156126057623,265.596508912376,51.4747805783874));
#33058=CARTESIAN_POINT('Ctrl Pts',(67.6462477917014,265.419412340377,49.3126512351539));
#33059=CARTESIAN_POINT('Ctrl Pts',(69.0245064208028,265.242315768379,47.3568408855417));
#33060=CARTESIAN_POINT('Ctrl Pts',(70.9158061804538,265.06521919638,46.224041177127));
#33061=CARTESIAN_POINT('Ctrl Pts',(72.8071059401047,264.888122624381,45.0912414687123));
#33062=CARTESIAN_POINT('Ctrl Pts',(75.1818659698185,264.711026052383,44.799169947306));
#33063=CARTESIAN_POINT('Ctrl Pts',(77.2912945088743,264.533929480384,45.439920443878));
#33064=CARTESIAN_POINT('Ctrl Pts',(79.40072304793,264.356832908385,46.0806709404499));
#33065=CARTESIAN_POINT('Ctrl Pts',(81.2118275942128,264.179736336386,47.6442218013997));
#33066=CARTESIAN_POINT('Ctrl Pts',(82.1535440633131,264.002639764388,49.6375657386231));
#33067=CARTESIAN_POINT('Ctrl Pts',(82.6515697929937,263.908982435045,50.6917435101858));
#33068=CARTESIAN_POINT('Ctrl Pts',(82.9129498948705,263.815325105703,51.856911993548));
#33069=CARTESIAN_POINT('Ctrl Pts',(82.9129498948689,263.721667776361,53.0228109606463));
#33070=CARTESIAN_POINT('Origin',(74.9879498948689,255.,53.0228109606356));
#33071=CARTESIAN_POINT('',(82.9129854222471,258.278332223638,53.0230546176887));
#33072=CARTESIAN_POINT('',(82.9072183307991,259.721667776361,53.024065690185));
#33073=CARTESIAN_POINT('',(82.9129498948689,255.,53.0228109606356));
#33074=CARTESIAN_POINT('Ctrl Pts',(82.9129498948689,258.278332223638,53.0228109606327));
#33075=CARTESIAN_POINT('Ctrl Pts',(82.9129498948681,258.455428795637,50.8182135007229));
#33076=CARTESIAN_POINT('Ctrl Pts',(81.9432795991091,258.632525367635,48.630856536287));
#33077=CARTESIAN_POINT('Ctrl Pts',(80.3096882702522,258.809621939634,47.1504412801767));
#33078=CARTESIAN_POINT('Ctrl Pts',(78.6760969413952,258.986718511633,45.6700260240663));
#33079=CARTESIAN_POINT('Ctrl Pts',(76.4041347530417,259.163815083632,44.9197069006026));
#33080=CARTESIAN_POINT('Ctrl Pts',(74.2101800112192,259.34091165563,45.1360689838693));
#33081=CARTESIAN_POINT('Ctrl Pts',(72.0162252693967,259.518008227629,45.352431067136));
#33082=CARTESIAN_POINT('Ctrl Pts',(69.9345925076956,259.695104799628,46.5320903475032));
#33083=CARTESIAN_POINT('Ctrl Pts',(68.6216467656591,259.872201371627,48.3030853894807));
#33084=CARTESIAN_POINT('Ctrl Pts',(67.3087010236226,260.049297943625,50.0740804314582));
#33085=CARTESIAN_POINT('Ctrl Pts',(66.7849774198237,260.226394515624,52.4087119996436));
#33086=CARTESIAN_POINT('Ctrl Pts',(67.2156126057611,260.403491087623,54.5708413428776));
#33087=CARTESIAN_POINT('Ctrl Pts',(67.6462477916985,260.580587659622,56.7329706861116));
#33088=CARTESIAN_POINT('Ctrl Pts',(69.0245064207986,260.75768423162,58.688781035725));
#33089=CARTESIAN_POINT('Ctrl Pts',(70.9158061804488,260.934780803619,59.8215807441412));
#33090=CARTESIAN_POINT('Ctrl Pts',(72.807105940099,261.111877375618,60.9543804525574));
#33091=CARTESIAN_POINT('Ctrl Pts',(75.1818659698128,261.288973947616,61.2464519739653));
#33092=CARTESIAN_POINT('Ctrl Pts',(77.2912945088691,261.466070519615,60.6057014773947));
#33093=CARTESIAN_POINT('Ctrl Pts',(79.4007230479255,261.643167091614,59.9649509808241));
#33094=CARTESIAN_POINT('Ctrl Pts',(81.2118275942094,261.820263663613,58.4014001198754));
#33095=CARTESIAN_POINT('Ctrl Pts',(82.153544063311,261.997360235611,56.4080561826525));
#33096=CARTESIAN_POINT('Ctrl Pts',(82.6515697929918,262.091017564954,55.3538784110911));
#33097=CARTESIAN_POINT('Ctrl Pts',(82.9129498948693,262.184674894296,54.1887099277303));
#33098=CARTESIAN_POINT('Ctrl Pts',(82.9129498948689,262.278332223638,53.0228109606331));
#33099=CARTESIAN_POINT('Ctrl Pts',(82.9129498948689,263.721667776361,53.0228109606463));
#33100=CARTESIAN_POINT('Ctrl Pts',(82.9129498948659,263.544571204362,55.2274084205561));
#33101=CARTESIAN_POINT('Ctrl Pts',(81.9432795991047,263.367474632363,57.4147653849911));
#33102=CARTESIAN_POINT('Ctrl Pts',(80.3096882702463,263.190378060365,58.8951806410998));
#33103=CARTESIAN_POINT('Ctrl Pts',(78.6760969413879,263.013281488366,60.3755958972085));
#33104=CARTESIAN_POINT('Ctrl Pts',(76.4041347530336,262.836184916367,61.12591502067));
#33105=CARTESIAN_POINT('Ctrl Pts',(74.2101800112113,262.659088344368,60.9095529374011));
#33106=CARTESIAN_POINT('Ctrl Pts',(72.0162252693891,262.48199177237,60.6931908541322));
#33107=CARTESIAN_POINT('Ctrl Pts',(69.9345925076892,262.304895200371,59.513531573763));
#33108=CARTESIAN_POINT('Ctrl Pts',(68.6216467656544,262.127798628372,57.7425365317841));
#33109=CARTESIAN_POINT('Ctrl Pts',(67.3087010236196,261.950702056374,55.9715414898053));
#33110=CARTESIAN_POINT('Ctrl Pts',(66.7849774198231,261.773605484375,53.6369099216194));
#33111=CARTESIAN_POINT('Ctrl Pts',(67.2156126057626,261.596508912376,51.4747805783858));
#33112=CARTESIAN_POINT('Ctrl Pts',(67.6462477917022,261.419412340377,49.3126512351523));
#33113=CARTESIAN_POINT('Ctrl Pts',(69.0245064208042,261.242315768379,47.3568408855402));
#33114=CARTESIAN_POINT('Ctrl Pts',(70.9158061804556,261.06521919638,46.2240411771259));
#33115=CARTESIAN_POINT('Ctrl Pts',(72.8071059401069,260.888122624381,45.0912414687116));
#33116=CARTESIAN_POINT('Ctrl Pts',(75.181865969821,260.711026052382,44.799169947306));
#33117=CARTESIAN_POINT('Ctrl Pts',(77.2912945088767,260.533929480384,45.4399204438787));
#33118=CARTESIAN_POINT('Ctrl Pts',(79.4007230479324,260.356832908385,46.0806709404514));
#33119=CARTESIAN_POINT('Ctrl Pts',(81.2118275942148,260.179736336386,47.6442218014019));
#33120=CARTESIAN_POINT('Ctrl Pts',(82.1535440633144,260.002639764387,49.6375657386258));
#33121=CARTESIAN_POINT('Ctrl Pts',(82.6515697929941,259.908982435045,50.6917435101877));
#33122=CARTESIAN_POINT('Ctrl Pts',(82.9129498948705,259.815325105703,51.8569119935489));
#33123=CARTESIAN_POINT('Ctrl Pts',(82.9129498948689,259.721667776361,53.0228109606461));
#33124=CARTESIAN_POINT('Origin',(74.9879498948689,255.,53.0228109606356));
#33125=CARTESIAN_POINT('',(82.9240197340883,254.278332223638,53.020308991551));
#33126=CARTESIAN_POINT('',(82.9135245211875,255.721667776361,53.0233051945254));
#33127=CARTESIAN_POINT('',(82.9129498948689,255.,53.0228109606356));
#33128=CARTESIAN_POINT('Ctrl Pts',(82.9240197340883,254.278332223638,53.020308991551));
#33129=CARTESIAN_POINT('Ctrl Pts',(82.9245880973683,254.289547740762,52.8812896590367));
#33130=CARTESIAN_POINT('Ctrl Pts',(82.9212449384694,254.300763257887,52.7422985421507));
#33131=CARTESIAN_POINT('Ctrl Pts',(82.9139033389865,254.311978775011,52.6035189473502));
#33132=CARTESIAN_POINT('Ctrl Pts',(82.7750274911087,254.524134784563,49.9783234513351));
#33133=CARTESIAN_POINT('Ctrl Pts',(81.2054050595906,254.736290794115,47.4288160879574));
#33134=CARTESIAN_POINT('Ctrl Pts',(78.9209890990964,254.948446803668,46.1267534038997));
#33135=CARTESIAN_POINT('Ctrl Pts',(76.6365731386022,255.16060281322,44.8246907198419));
#33136=CARTESIAN_POINT('Ctrl Pts',(73.6373636491319,255.372758822773,44.7700727151041));
#33137=CARTESIAN_POINT('Ctrl Pts',(71.3092683796031,255.584914832325,45.9876248280484));
#33138=CARTESIAN_POINT('Ctrl Pts',(68.9811731100745,255.797070841877,47.2051769409925));
#33139=CARTESIAN_POINT('Ctrl Pts',(67.3241920604874,256.009226851429,49.6948991716185));
#33140=CARTESIAN_POINT('Ctrl Pts',(67.0844388701906,256.221382860982,52.3149070557222));
#33141=CARTESIAN_POINT('Ctrl Pts',(66.9645622750422,256.327460865758,53.6249109977741));
#33142=CARTESIAN_POINT('Ctrl Pts',(67.1989926447164,256.433538870534,54.9674863531954));
#33143=CARTESIAN_POINT('Ctrl Pts',(67.7275122687358,256.53961687531,56.182092725699));
#33144=CARTESIAN_POINT('Ctrl Pts',(68.2560318927553,256.645694880087,57.3966990982028));
#33145=CARTESIAN_POINT('Ctrl Pts',(69.0786407711201,256.751772884863,58.4833364877888));
#33146=CARTESIAN_POINT('Ctrl Pts',(70.118911778983,256.857850889639,59.2885178067825));
#33147=CARTESIAN_POINT('Ctrl Pts',(72.1994537947081,257.070006899191,60.8988804447697));
#33148=CARTESIAN_POINT('Ctrl Pts',(75.1506443284247,257.282162908743,61.3834188003888));
#33149=CARTESIAN_POINT('Ctrl Pts',(77.6283867922959,257.494318918295,60.5097752721314));
#33150=CARTESIAN_POINT('Ctrl Pts',(80.1061292561671,257.706474927848,59.636131743874));
#33151=CARTESIAN_POINT('Ctrl Pts',(82.1104236501927,257.918630937401,57.4043063317401));
#33152=CARTESIAN_POINT('Ctrl Pts',(82.7147281367444,258.130786946953,54.8452558044333));
#33153=CARTESIAN_POINT('Ctrl Pts',(82.8548172985812,258.179968705848,54.2520196934219));
#33154=CARTESIAN_POINT('Ctrl Pts',(82.9196710418623,258.229150464743,53.6411985138535));
#33155=CARTESIAN_POINT('Ctrl Pts',(82.913891463064,258.278332223638,53.0292685081989));
#33156=CARTESIAN_POINT('Ctrl Pts',(82.8980640920389,259.721667776361,53.0260696970247));
#33157=CARTESIAN_POINT('Ctrl Pts',(82.9017487919349,259.624066834371,54.2447780477463));
#33158=CARTESIAN_POINT('Ctrl Pts',(82.6388455870243,259.526465892382,55.462052251796));
#33159=CARTESIAN_POINT('Ctrl Pts',(82.1026481438308,259.428864950392,56.5452547766708));
#33160=CARTESIAN_POINT('Ctrl Pts',(80.9371111360811,259.21670894084,58.8998214491826));
#33161=CARTESIAN_POINT('Ctrl Pts',(78.4802563401325,259.004552931287,60.6208982051109));
#33162=CARTESIAN_POINT('Ctrl Pts',(75.867072311377,258.792396921735,60.9127761687082));
#33163=CARTESIAN_POINT('Ctrl Pts',(73.2538882826217,258.580240912183,61.2046541323055));
#33164=CARTESIAN_POINT('Ctrl Pts',(70.4843750210593,258.368084902631,60.0673333035724));
#33165=CARTESIAN_POINT('Ctrl Pts',(68.8270002240545,258.155928893078,58.026733716276));
#33166=CARTESIAN_POINT('Ctrl Pts',(67.1696254270496,257.943772883526,55.9861341289796));
#33167=CARTESIAN_POINT('Ctrl Pts',(66.6243890946025,257.731616873974,53.0422557831199));
#33168=CARTESIAN_POINT('Ctrl Pts',(67.445923452996,257.519460864421,50.5444557887738));
#33169=CARTESIAN_POINT('Ctrl Pts',(68.2674578113894,257.307304854869,48.0466557944278));
#33170=CARTESIAN_POINT('Ctrl Pts',(70.4557628606232,257.095148845317,45.9949341515953));
#33171=CARTESIAN_POINT('Ctrl Pts',(72.9992984648703,256.882992835764,45.3369923899906));
#33172=CARTESIAN_POINT('Ctrl Pts',(75.5428340691175,256.670836826212,44.6790506283859));
#33173=CARTESIAN_POINT('Ctrl Pts',(78.4416002283781,256.45868081666,45.4148887480092));
#33174=CARTESIAN_POINT('Ctrl Pts',(80.3763781282835,256.246524807107,47.197739662433));
#33175=CARTESIAN_POINT('Ctrl Pts',(81.3437670782363,256.140446802331,48.089165119645));
#33176=CARTESIAN_POINT('Ctrl Pts',(82.0701589633502,256.034368797555,49.2423437755571));
#33177=CARTESIAN_POINT('Ctrl Pts',(82.4925707755548,255.928290792779,50.4977998257677));
#33178=CARTESIAN_POINT('Ctrl Pts',(82.7668343642302,255.859416453973,51.3129424704724));
#33179=CARTESIAN_POINT('Ctrl Pts',(82.9129506957147,255.790542115167,52.1712016505031));
#33180=CARTESIAN_POINT('Ctrl Pts',(82.9182664199887,255.721667776361,53.0273836833877));
#33181=CARTESIAN_POINT('Origin',(74.9879498948689,255.,53.0228109606356));
#33182=CARTESIAN_POINT('',(82.9108136270844,250.278332223638,53.0211339884677));
#33183=CARTESIAN_POINT('',(82.9145920656403,251.721667776361,53.0222231462556));
#33184=CARTESIAN_POINT('',(82.9129498948689,255.,53.0228109606356));
#33185=CARTESIAN_POINT('Ctrl Pts',(82.905956915151,250.278332223638,53.0173214651763));
#33186=CARTESIAN_POINT('Ctrl Pts',(82.9125926517432,250.349945016782,52.124131973143));
#33187=CARTESIAN_POINT('Ctrl Pts',(82.7733011338671,250.421557809925,51.2327677033672));
#33188=CARTESIAN_POINT('Ctrl Pts',(82.4793208338808,250.493170603069,50.3953085987083));
#33189=CARTESIAN_POINT('Ctrl Pts',(81.6083914287547,250.705326612622,47.9142996335767));
#33190=CARTESIAN_POINT('Ctrl Pts',(79.379810627856,250.917482622174,45.9063981663636));
#33191=CARTESIAN_POINT('Ctrl Pts',(76.823722010962,251.129638631726,45.299050066571));
#33192=CARTESIAN_POINT('Ctrl Pts',(74.2676333940679,251.341794641279,44.6917019667784));
#33193=CARTESIAN_POINT('Ctrl Pts',(71.3840369611785,251.553950650831,45.4849072344063));
#33194=CARTESIAN_POINT('Ctrl Pts',(69.4850119429622,251.766106660383,47.3057935255329));
#33195=CARTESIAN_POINT('Ctrl Pts',(68.5354994338542,251.872184665159,48.2162366710961));
#33196=CARTESIAN_POINT('Ctrl Pts',(67.8321297784144,251.978262669935,49.383600072534));
#33197=CARTESIAN_POINT('Ctrl Pts',(67.4347095618133,252.084340674712,50.6471897229097));
#33198=CARTESIAN_POINT('Ctrl Pts',(67.0372893452122,252.190418679488,51.9107793732854));
#33199=CARTESIAN_POINT('Ctrl Pts',(66.9458185674498,252.296496684264,53.2705952725989));
#33200=CARTESIAN_POINT('Ctrl Pts',(67.2032406976284,252.40257468904,54.5606396800323));
#33201=CARTESIAN_POINT('Ctrl Pts',(67.7180849579855,252.614730698593,57.1407284948992));
#33202=CARTESIAN_POINT('Ctrl Pts',(69.6285008501065,252.826886708145,59.4417313422457));
#33203=CARTESIAN_POINT('Ctrl Pts',(72.0720622916857,253.039042717697,60.4068573510985));
#33204=CARTESIAN_POINT('Ctrl Pts',(74.515623733265,253.251198727249,61.3719833599513));
#33205=CARTESIAN_POINT('Ctrl Pts',(77.4923307243023,253.463354736802,61.0012325303105));
#33206=CARTESIAN_POINT('Ctrl Pts',(79.6266195877023,253.675510746354,59.4654153011639));
#33207=CARTESIAN_POINT('Ctrl Pts',(81.6480803801642,253.876451238782,58.0107882512143));
#33208=CARTESIAN_POINT('Ctrl Pts',(82.9138367709577,254.07739173121,55.5110201039194));
#33209=CARTESIAN_POINT('Ctrl Pts',(82.9240197340883,254.278332223638,53.020308991551));
#33210=CARTESIAN_POINT('Ctrl Pts',(82.9129498948689,255.721667776361,53.0228109606459));
#33211=CARTESIAN_POINT('Ctrl Pts',(82.912949894866,255.544571204362,55.2274084205558));
#33212=CARTESIAN_POINT('Ctrl Pts',(81.9432795991048,255.367474632363,57.4147653849909));
#33213=CARTESIAN_POINT('Ctrl Pts',(80.3096882702464,255.190378060365,58.8951806410997));
#33214=CARTESIAN_POINT('Ctrl Pts',(78.676096941388,255.013281488366,60.3755958972085));
#33215=CARTESIAN_POINT('Ctrl Pts',(76.4041347530336,254.836184916367,61.12591502067));
#33216=CARTESIAN_POINT('Ctrl Pts',(74.2101800112112,254.659088344368,60.9095529374011));
#33217=CARTESIAN_POINT('Ctrl Pts',(72.0162252693889,254.48199177237,60.6931908541322));
#33218=CARTESIAN_POINT('Ctrl Pts',(69.9345925076889,254.304895200371,59.5135315737628));
#33219=CARTESIAN_POINT('Ctrl Pts',(68.6216467656542,254.127798628372,57.7425365317838));
#33220=CARTESIAN_POINT('Ctrl Pts',(67.3087010236195,253.950702056374,55.9715414898049));
#33221=CARTESIAN_POINT('Ctrl Pts',(66.784977419823,253.773605484375,53.6369099216189));
#33222=CARTESIAN_POINT('Ctrl Pts',(67.2156126057627,253.596508912376,51.4747805783853));
#33223=CARTESIAN_POINT('Ctrl Pts',(67.6462477917025,253.419412340377,49.3126512351517));
#33224=CARTESIAN_POINT('Ctrl Pts',(69.0245064208047,253.242315768379,47.3568408855397));
#33225=CARTESIAN_POINT('Ctrl Pts',(70.9158061804562,253.06521919638,46.2240411771255));
#33226=CARTESIAN_POINT('Ctrl Pts',(72.8071059401077,252.888122624381,45.0912414687114));
#33227=CARTESIAN_POINT('Ctrl Pts',(75.1818659698218,252.711026052382,44.799169947306));
#33228=CARTESIAN_POINT('Ctrl Pts',(77.2912945088774,252.533929480384,45.4399204438789));
#33229=CARTESIAN_POINT('Ctrl Pts',(79.4007230479332,252.356832908385,46.0806709404519));
#33230=CARTESIAN_POINT('Ctrl Pts',(81.2118275942155,252.179736336386,47.6442218014027));
#33231=CARTESIAN_POINT('Ctrl Pts',(82.1535440633149,252.002639764387,49.6375657386269));
#33232=CARTESIAN_POINT('Ctrl Pts',(82.6515697929943,251.908982435045,50.6917435101885));
#33233=CARTESIAN_POINT('Ctrl Pts',(82.9129498948704,251.815325105703,51.8569119935492));
#33234=CARTESIAN_POINT('Ctrl Pts',(82.9129498948689,251.721667776361,53.022810960646));
#33235=CARTESIAN_POINT('Origin',(74.9879498948689,255.,53.0228109606356));
#33236=CARTESIAN_POINT('',(82.9094889824334,246.278332223638,53.0243238363652));
#33237=CARTESIAN_POINT('',(82.9070612414929,247.721667776361,53.0201181858126));
#33238=CARTESIAN_POINT('',(82.9129498948689,255.,53.0228109606356));
#33239=CARTESIAN_POINT('Ctrl Pts',(82.9129498948689,246.278332223638,53.0228109606324));
#33240=CARTESIAN_POINT('Ctrl Pts',(82.912949894868,246.455428795637,50.8182135007226));
#33241=CARTESIAN_POINT('Ctrl Pts',(81.9432795991089,246.632525367636,48.6308565362867));
#33242=CARTESIAN_POINT('Ctrl Pts',(80.3096882702519,246.809621939634,47.1504412801765));
#33243=CARTESIAN_POINT('Ctrl Pts',(78.676096941395,246.986718511633,45.6700260240662));
#33244=CARTESIAN_POINT('Ctrl Pts',(76.4041347530414,247.163815083632,44.9197069006025));
#33245=CARTESIAN_POINT('Ctrl Pts',(74.2101800112189,247.34091165563,45.1360689838693));
#33246=CARTESIAN_POINT('Ctrl Pts',(72.0162252693964,247.518008227629,45.3524310671361));
#33247=CARTESIAN_POINT('Ctrl Pts',(69.9345925076954,247.695104799628,46.5320903475033));
#33248=CARTESIAN_POINT('Ctrl Pts',(68.6216467656589,247.872201371627,48.3030853894809));
#33249=CARTESIAN_POINT('Ctrl Pts',(67.3087010236224,248.049297943625,50.0740804314585));
#33250=CARTESIAN_POINT('Ctrl Pts',(66.7849774198237,248.226394515624,52.4087119996439));
#33251=CARTESIAN_POINT('Ctrl Pts',(67.2156126057612,248.403491087623,54.5708413428779));
#33252=CARTESIAN_POINT('Ctrl Pts',(67.6462477916987,248.580587659622,56.7329706861118));
#33253=CARTESIAN_POINT('Ctrl Pts',(69.0245064207988,248.75768423162,58.6887810357252));
#33254=CARTESIAN_POINT('Ctrl Pts',(70.9158061804491,248.934780803619,59.8215807441413));
#33255=CARTESIAN_POINT('Ctrl Pts',(72.8071059400993,249.111877375618,60.9543804525574));
#33256=CARTESIAN_POINT('Ctrl Pts',(75.1818659698131,249.288973947616,61.2464519739653));
#33257=CARTESIAN_POINT('Ctrl Pts',(77.2912945088694,249.466070519615,60.6057014773946));
#33258=CARTESIAN_POINT('Ctrl Pts',(79.4007230479258,249.643167091614,59.964950980824));
#33259=CARTESIAN_POINT('Ctrl Pts',(81.2118275942096,249.820263663613,58.4014001198752));
#33260=CARTESIAN_POINT('Ctrl Pts',(82.1535440633112,249.997360235611,56.4080561826522));
#33261=CARTESIAN_POINT('Ctrl Pts',(82.6515697929919,250.091017564954,55.3538784110907));
#33262=CARTESIAN_POINT('Ctrl Pts',(82.9129498948693,250.184674894296,54.1887099277298));
#33263=CARTESIAN_POINT('Ctrl Pts',(82.9129498948689,250.278332223638,53.0228109606326));
#33264=CARTESIAN_POINT('Ctrl Pts',(82.9214093282576,251.721667776361,53.0197829096366));
#33265=CARTESIAN_POINT('Ctrl Pts',(82.916679486065,251.638783381634,54.048787391814));
#33266=CARTESIAN_POINT('Ctrl Pts',(82.7036892742198,251.555898986907,55.0803795699231));
#33267=CARTESIAN_POINT('Ctrl Pts',(82.3096390686196,251.47301459218,56.0374226167223));
#33268=CARTESIAN_POINT('Ctrl Pts',(81.8053214617955,251.366936587404,57.26227582611));
#33269=CARTESIAN_POINT('Ctrl Pts',(81.0044335625822,251.260858582628,58.3650200195222));
#33270=CARTESIAN_POINT('Ctrl Pts',(79.9803422437528,251.154780577852,59.1906819945182));
#33271=CARTESIAN_POINT('Ctrl Pts',(77.9321596060941,250.9426245683,60.8420059445101));
#33272=CARTESIAN_POINT('Ctrl Pts',(74.9911632899713,250.730468558747,61.3850010208379));
#33273=CARTESIAN_POINT('Ctrl Pts',(72.496575305283,250.518312549195,60.5606882656381));
#33274=CARTESIAN_POINT('Ctrl Pts',(70.0019873205946,250.306156539643,59.7363755104383));
#33275=CARTESIAN_POINT('Ctrl Pts',(67.9538076673407,250.09400053009,57.5447549237108));
#33276=CARTESIAN_POINT('Ctrl Pts',(67.2988501551073,249.881844520538,54.998197606283));
#33277=CARTESIAN_POINT('Ctrl Pts',(66.6438926428738,249.669688510986,52.4516402888551));
#33278=CARTESIAN_POINT('Ctrl Pts',(67.3821572716608,249.457532501433,49.5501462407268));
#33279=CARTESIAN_POINT('Ctrl Pts',(69.1705455751325,249.245376491881,47.623334062691));
#33280=CARTESIAN_POINT('Ctrl Pts',(70.9589338786041,249.033220482329,45.6965218846554));
#33281=CARTESIAN_POINT('Ctrl Pts',(73.7974458567604,248.821064472776,44.7443915767121));
#33282=CARTESIAN_POINT('Ctrl Pts',(76.3856808148585,248.608908463224,45.2080329418362));
#33283=CARTESIAN_POINT('Ctrl Pts',(78.9739157729569,248.396752453672,45.6716743069604));
#33284=CARTESIAN_POINT('Ctrl Pts',(81.311873710997,248.184596444119,47.5510873451521));
#33285=CARTESIAN_POINT('Ctrl Pts',(82.3195339490888,247.972440434567,49.97741823279));
#33286=CARTESIAN_POINT('Ctrl Pts',(82.7165588193061,247.888849548498,50.9334088230239));
#33287=CARTESIAN_POINT('Ctrl Pts',(82.9070665877906,247.80525866243,51.9743036336875));
#33288=CARTESIAN_POINT('Ctrl Pts',(82.9007584226264,247.721667776361,53.0172360205809));
#33289=CARTESIAN_POINT('Origin',(74.9879498948689,255.,53.0228109606356));
#33290=CARTESIAN_POINT('',(82.9161917637328,242.278332223638,53.0237563384547));
#33291=CARTESIAN_POINT('',(82.9098680058837,243.721667776361,53.0268864946943));
#33292=CARTESIAN_POINT('',(82.9129498948689,255.,53.0228109606356));
#33293=CARTESIAN_POINT('Ctrl Pts',(82.9238601319149,242.278332223638,53.0259925502159));
#33294=CARTESIAN_POINT('Ctrl Pts',(82.907066140212,242.470739568821,50.6417088931013));
#33295=CARTESIAN_POINT('Ctrl Pts',(81.7542886292362,242.663146914003,48.2474956051494));
#33296=CARTESIAN_POINT('Ctrl Pts',(79.8779861178407,242.855554259186,46.773478180744));
#33297=CARTESIAN_POINT('Ctrl Pts',(78.8435431417868,242.961632263962,45.9608229921502));
#33298=CARTESIAN_POINT('Ctrl Pts',(77.5891820870839,243.067710268738,45.4278647126812));
#33299=CARTESIAN_POINT('Ctrl Pts',(76.2823888503532,243.173788273514,45.2113166359524));
#33300=CARTESIAN_POINT('Ctrl Pts',(74.9755956136225,243.279866278291,44.9947685592237));
#33301=CARTESIAN_POINT('Ctrl Pts',(73.616370194864,243.385944283067,45.0946306852353));
#33302=CARTESIAN_POINT('Ctrl Pts',(72.375088412559,243.492022287843,45.5301766221626));
#33303=CARTESIAN_POINT('Ctrl Pts',(69.8925248479489,243.704178297395,46.4012684960171));
#33304=CARTESIAN_POINT('Ctrl Pts',(67.8817358291529,243.916334306947,48.615095613534));
#33305=CARTESIAN_POINT('Ctrl Pts',(67.2683221486002,244.1284903165,51.1697353901461));
#33306=CARTESIAN_POINT('Ctrl Pts',(66.6549084680477,244.340646326052,53.7243751667579));
#33307=CARTESIAN_POINT('Ctrl Pts',(67.4388701257386,244.552802335605,56.6198276024647));
#33308=CARTESIAN_POINT('Ctrl Pts',(69.2584430647217,244.764958345157,58.5180051056228));
#33309=CARTESIAN_POINT('Ctrl Pts',(71.078016003705,244.977114354709,60.4161826087811));
#33310=CARTESIAN_POINT('Ctrl Pts',(73.9332002239807,245.189270364261,61.3170851793908));
#33311=CARTESIAN_POINT('Ctrl Pts',(76.5130773837582,245.401426373813,60.8119399192136));
#33312=CARTESIAN_POINT('Ctrl Pts',(79.0929545435357,245.613582383366,60.3067946590365));
#33313=CARTESIAN_POINT('Ctrl Pts',(81.3975246428152,245.825738392919,58.3956015680724));
#33314=CARTESIAN_POINT('Ctrl Pts',(82.3668417432141,246.037894402471,55.9513536525265));
#33315=CARTESIAN_POINT('Ctrl Pts',(82.7330195889922,246.11804034286,55.0279928288149));
#33316=CARTESIAN_POINT('Ctrl Pts',(82.9086443675112,246.198186283249,54.0285601056758));
#33317=CARTESIAN_POINT('Ctrl Pts',(82.9028596079635,246.278332223638,53.0272217483888));
#33318=CARTESIAN_POINT('Ctrl Pts',(82.9129498948689,247.721667776361,53.0228109606458));
#33319=CARTESIAN_POINT('Ctrl Pts',(82.912949894866,247.544571204362,55.2274084205557));
#33320=CARTESIAN_POINT('Ctrl Pts',(81.943279599105,247.367474632363,57.4147653849906));
#33321=CARTESIAN_POINT('Ctrl Pts',(80.3096882702467,247.190378060365,58.8951806410995));
#33322=CARTESIAN_POINT('Ctrl Pts',(78.6760969413883,247.013281488366,60.3755958972083));
#33323=CARTESIAN_POINT('Ctrl Pts',(76.4041347530341,246.836184916367,61.1259150206699));
#33324=CARTESIAN_POINT('Ctrl Pts',(74.2101800112118,246.659088344368,60.9095529374011));
#33325=CARTESIAN_POINT('Ctrl Pts',(72.0162252693895,246.48199177237,60.6931908541324));
#33326=CARTESIAN_POINT('Ctrl Pts',(69.9345925076895,246.304895200371,59.5135315737633));
#33327=CARTESIAN_POINT('Ctrl Pts',(68.6216467656547,246.127798628372,57.7425365317845));
#33328=CARTESIAN_POINT('Ctrl Pts',(67.3087010236198,245.950702056374,55.9715414898057));
#33329=CARTESIAN_POINT('Ctrl Pts',(66.7849774198231,245.773605484375,53.6369099216199));
#33330=CARTESIAN_POINT('Ctrl Pts',(67.2156126057625,245.596508912376,51.4747805783863));
#33331=CARTESIAN_POINT('Ctrl Pts',(67.646247791702,245.419412340377,49.3126512351527));
#33332=CARTESIAN_POINT('Ctrl Pts',(69.0245064208039,245.242315768379,47.3568408855406));
#33333=CARTESIAN_POINT('Ctrl Pts',(70.9158061804552,245.06521919638,46.2240411771262));
#33334=CARTESIAN_POINT('Ctrl Pts',(72.8071059401065,244.888122624381,45.0912414687117));
#33335=CARTESIAN_POINT('Ctrl Pts',(75.1818659698205,244.711026052382,44.799169947306));
#33336=CARTESIAN_POINT('Ctrl Pts',(77.2912945088762,244.533929480384,45.4399204438786));
#33337=CARTESIAN_POINT('Ctrl Pts',(79.400723047932,244.356832908385,46.0806709404511));
#33338=CARTESIAN_POINT('Ctrl Pts',(81.2118275942144,244.179736336386,47.6442218014015));
#33339=CARTESIAN_POINT('Ctrl Pts',(82.1535440633142,244.002639764388,49.6375657386254));
#33340=CARTESIAN_POINT('Ctrl Pts',(82.6515697929939,243.908982435045,50.6917435101872));
#33341=CARTESIAN_POINT('Ctrl Pts',(82.9129498948703,243.815325105703,51.8569119935481));
#33342=CARTESIAN_POINT('Ctrl Pts',(82.9129498948689,243.721667776361,53.0228109606452));
#33343=CARTESIAN_POINT('Origin',(74.9879498948689,255.,53.0228109606356));
#33344=CARTESIAN_POINT('',(82.9128050499553,238.278332223638,53.0219540812206));
#33345=CARTESIAN_POINT('',(82.926321989507,239.721667776361,53.0235034425041));
#33346=CARTESIAN_POINT('',(82.9129498948689,255.,53.0228109606356));
#33347=CARTESIAN_POINT('Ctrl Pts',(82.9129498948689,238.278332223638,53.0228109606321));
#33348=CARTESIAN_POINT('Ctrl Pts',(82.9129498948679,238.455428795637,50.8182135007223));
#33349=CARTESIAN_POINT('Ctrl Pts',(81.9432795991088,238.632525367636,48.6308565362865));
#33350=CARTESIAN_POINT('Ctrl Pts',(80.3096882702517,238.809621939634,47.1504412801762));
#33351=CARTESIAN_POINT('Ctrl Pts',(78.6760969413946,238.986718511633,45.670026024066));
#33352=CARTESIAN_POINT('Ctrl Pts',(76.404134753041,239.163815083632,44.9197069006025));
#33353=CARTESIAN_POINT('Ctrl Pts',(74.2101800112185,239.34091165563,45.1360689838693));
#33354=CARTESIAN_POINT('Ctrl Pts',(72.0162252693961,239.518008227629,45.3524310671362));
#33355=CARTESIAN_POINT('Ctrl Pts',(69.9345925076951,239.695104799628,46.5320903475036));
#33356=CARTESIAN_POINT('Ctrl Pts',(68.6216467656587,239.872201371627,48.3030853894812));
#33357=CARTESIAN_POINT('Ctrl Pts',(67.3087010236223,240.049297943625,50.0740804314588));
#33358=CARTESIAN_POINT('Ctrl Pts',(66.7849774198236,240.226394515624,52.4087119996442));
#33359=CARTESIAN_POINT('Ctrl Pts',(67.2156126057612,240.403491087623,54.5708413428782));
#33360=CARTESIAN_POINT('Ctrl Pts',(67.6462477916988,240.580587659622,56.7329706861122));
#33361=CARTESIAN_POINT('Ctrl Pts',(69.024506420799,240.75768423162,58.6887810357255));
#33362=CARTESIAN_POINT('Ctrl Pts',(70.9158061804494,240.934780803619,59.8215807441415));
#33363=CARTESIAN_POINT('Ctrl Pts',(72.8071059400997,241.111877375618,60.9543804525575));
#33364=CARTESIAN_POINT('Ctrl Pts',(75.1818659698135,241.288973947617,61.2464519739653));
#33365=CARTESIAN_POINT('Ctrl Pts',(77.2912945088698,241.466070519615,60.6057014773945));
#33366=CARTESIAN_POINT('Ctrl Pts',(79.400723047926,241.643167091614,59.9649509808238));
#33367=CARTESIAN_POINT('Ctrl Pts',(81.2118275942098,241.820263663613,58.401400119875));
#33368=CARTESIAN_POINT('Ctrl Pts',(82.1535440633113,241.997360235611,56.4080561826519));
#33369=CARTESIAN_POINT('Ctrl Pts',(82.6515697929921,242.091017564954,55.3538784110903));
#33370=CARTESIAN_POINT('Ctrl Pts',(82.9129498948695,242.184674894296,54.1887099277292));
#33371=CARTESIAN_POINT('Ctrl Pts',(82.9129498948689,242.278332223638,53.0228109606318));
#33372=CARTESIAN_POINT('Ctrl Pts',(82.9065114310396,243.721667776361,53.0313252772196));
#33373=CARTESIAN_POINT('Ctrl Pts',(82.9130325787133,243.653499928897,53.8818329308789));
#33374=CARTESIAN_POINT('Ctrl Pts',(82.7869871502048,243.585332081433,54.7301656950663));
#33375=CARTESIAN_POINT('Ctrl Pts',(82.5202253887267,243.517164233968,55.5310708147046));
#33376=CARTESIAN_POINT('Ctrl Pts',(81.6899936457324,243.305008224416,58.0236951314963));
#33377=CARTESIAN_POINT('Ctrl Pts',(79.4967613740554,243.092852214864,60.0569278252234));
#33378=CARTESIAN_POINT('Ctrl Pts',(76.9486412513389,242.880696205312,60.711913890137));
#33379=CARTESIAN_POINT('Ctrl Pts',(75.6745811899807,242.774618200535,61.0394069225938));
#33380=CARTESIAN_POINT('Ctrl Pts',(74.3117991658626,242.668540195759,61.0223382978473));
#33381=CARTESIAN_POINT('Ctrl Pts',(73.0283905058894,242.562462190983,60.6945215127286));
#33382=CARTESIAN_POINT('Ctrl Pts',(71.7449818459162,242.456384186207,60.3667047276099));
#33383=CARTESIAN_POINT('Ctrl Pts',(70.5409465500878,242.350306181431,59.728139782119));
#33384=CARTESIAN_POINT('Ctrl Pts',(69.5800050974343,242.244228176655,58.8297677818719));
#33385=CARTESIAN_POINT('Ctrl Pts',(67.6581221921272,242.032072167102,57.0330237813775));
#33386=CARTESIAN_POINT('Ctrl Pts',(66.7086146595198,241.81991615755,54.1970515618584));
#33387=CARTESIAN_POINT('Ctrl Pts',(67.1754568585284,241.607760147998,51.6116078682225));
#33388=CARTESIAN_POINT('Ctrl Pts',(67.6422990575369,241.395604138445,49.0261641745868));
#33389=CARTESIAN_POINT('Ctrl Pts',(69.5254909881617,241.183448128893,46.6912490068345));
#33390=CARTESIAN_POINT('Ctrl Pts',(71.9552317322733,240.971292119341,45.6861204428294));
#33391=CARTESIAN_POINT('Ctrl Pts',(74.3849724763853,240.759136109789,44.6809918788241));
#33392=CARTESIAN_POINT('Ctrl Pts',(77.3612620339845,240.546980100236,45.0056499185663));
#33393=CARTESIAN_POINT('Ctrl Pts',(79.519536230537,240.334824090684,46.5065797590045));
#33394=CARTESIAN_POINT('Ctrl Pts',(81.5987599968093,240.130438652576,47.9525355141774));
#33395=CARTESIAN_POINT('Ctrl Pts',(82.9187934056723,239.926053214469,50.4901751805651));
#33396=CARTESIAN_POINT('Ctrl Pts',(82.926321989507,239.721667776361,53.0235034425041));
#33397=CARTESIAN_POINT('Origin',(74.9879498948689,255.,53.0228109606356));
#33398=CARTESIAN_POINT('',(82.91116743,234.278332223638,53.0226183020154));
#33399=CARTESIAN_POINT('',(82.9111139440083,235.721667776361,53.0156317204369));
#33400=CARTESIAN_POINT('',(82.9129498948689,255.,53.0228109606356));
#33401=CARTESIAN_POINT('Ctrl Pts',(82.9060478678828,234.278332223638,53.0220649515909));
#33402=CARTESIAN_POINT('Ctrl Pts',(82.9069987852815,234.379378111307,51.7603229420665));
#33403=CARTESIAN_POINT('Ctrl Pts',(82.6172193617369,234.480423998977,50.4990581479779));
#33404=CARTESIAN_POINT('Ctrl Pts',(82.0408377393029,234.581469886646,49.386413360037));
#33405=CARTESIAN_POINT('Ctrl Pts',(80.8306665209031,234.793625896198,47.0503036607335));
#33406=CARTESIAN_POINT('Ctrl Pts',(78.3570602913277,235.00578190575,45.3693589247679));
#33407=CARTESIAN_POINT('Ctrl Pts',(75.74169133811,235.217937915302,45.1197472858543));
#33408=CARTESIAN_POINT('Ctrl Pts',(73.1263223848922,235.430093924855,44.8701356469406));
#33409=CARTESIAN_POINT('Ctrl Pts',(70.3691907080321,235.642249934407,46.0518571050791));
#33410=CARTESIAN_POINT('Ctrl Pts',(68.7445355694784,235.85440594396,48.1193239596012));
#33411=CARTESIAN_POINT('Ctrl Pts',(67.1198804309247,236.066561953512,50.1867908141234));
#33412=CARTESIAN_POINT('Ctrl Pts',(66.6277018306775,236.278717963064,53.1400030650291));
#33413=CARTESIAN_POINT('Ctrl Pts',(67.489160642071,236.490873972616,55.6237153288983));
#33414=CARTESIAN_POINT('Ctrl Pts',(68.3506194534644,236.703029982169,58.1074275927673));
#33415=CARTESIAN_POINT('Ctrl Pts',(70.5657156764983,236.915185991721,60.1216398695997));
#33416=CARTESIAN_POINT('Ctrl Pts',(73.1216220916204,237.127342001274,60.7391072055076));
#33417=CARTESIAN_POINT('Ctrl Pts',(75.6775285067427,237.339498010826,61.3565745414155));
#33418=CARTESIAN_POINT('Ctrl Pts',(78.5742451139533,237.551654020378,60.5772969363989));
#33419=CARTESIAN_POINT('Ctrl Pts',(80.4733674854168,237.76381002993,58.7618644948182));
#33420=CARTESIAN_POINT('Ctrl Pts',(82.0086223052805,237.935317427833,57.2942648035324));
#33421=CARTESIAN_POINT('Ctrl Pts',(82.8919351099652,238.106824825735,55.1495231962438));
#33422=CARTESIAN_POINT('Ctrl Pts',(82.9118918566993,238.278332223638,53.0165517755375));
#33423=CARTESIAN_POINT('Ctrl Pts',(82.926321989507,239.721667776361,53.0235034425041));
#33424=CARTESIAN_POINT('Ctrl Pts',(82.9266082202634,239.713897204916,53.1198185637504));
#33425=CARTESIAN_POINT('Ctrl Pts',(82.9249972780706,239.706126633472,53.216127453035));
#33426=CARTESIAN_POINT('Ctrl Pts',(82.921458755405,239.698356062027,53.3123698796841));
#33427=CARTESIAN_POINT('Ctrl Pts',(82.8248482482147,239.486200052475,55.9400285187916));
#33428=CARTESIAN_POINT('Ctrl Pts',(81.2913683983285,239.274044042922,58.5181441558727));
#33429=CARTESIAN_POINT('Ctrl Pts',(79.0300625577341,239.06188803337,59.8556629882746));
#33430=CARTESIAN_POINT('Ctrl Pts',(76.7687567171396,238.849732023818,61.1931818206766));
#33431=CARTESIAN_POINT('Ctrl Pts',(73.779624885837,238.637576014265,61.2901038483994));
#33432=CARTESIAN_POINT('Ctrl Pts',(71.4263082709551,238.425420004713,60.1137434380047));
#33433=CARTESIAN_POINT('Ctrl Pts',(70.2496499635141,238.319341999937,59.5255632328073));
#33434=CARTESIAN_POINT('Ctrl Pts',(69.2319454601783,238.213263995161,58.6190624180804));
#33435=CARTESIAN_POINT('Ctrl Pts',(68.4779338448622,238.107185990385,57.5299948733117));
#33436=CARTESIAN_POINT('Ctrl Pts',(67.7239222295461,238.001107985608,56.440927328543));
#33437=CARTESIAN_POINT('Ctrl Pts',(67.2336035022498,237.895029980832,55.1692930537326));
#33438=CARTESIAN_POINT('Ctrl Pts',(67.0971826990598,237.788951976056,53.8609085190056));
#33439=CARTESIAN_POINT('Ctrl Pts',(66.8243410926796,237.576795966504,51.2441394495514));
#33440=CARTESIAN_POINT('Ctrl Pts',(67.9670911827251,237.364639956951,48.4803693404307));
#33441=CARTESIAN_POINT('Ctrl Pts',(70.0149031101221,237.152483947399,46.834487497239));
#33442=CARTESIAN_POINT('Ctrl Pts',(72.0627150375189,236.940327937847,45.1886056540473));
#33443=CARTESIAN_POINT('Ctrl Pts',(75.0155888022669,236.728171928295,44.6606120767842));
#33444=CARTESIAN_POINT('Ctrl Pts',(77.5091274627469,236.516015918742,45.4949911647695));
#33445=CARTESIAN_POINT('Ctrl Pts',(80.0026661232272,236.30385990919,46.3293702527549));
#33446=CARTESIAN_POINT('Ctrl Pts',(82.0368696794392,236.091703899637,48.5261220059891));
#33447=CARTESIAN_POINT('Ctrl Pts',(82.6821596603463,235.879547890085,51.0745604953318));
#33448=CARTESIAN_POINT('Ctrl Pts',(82.8422281178079,235.82692118551,51.7067175564894));
#33449=CARTESIAN_POINT('Ctrl Pts',(82.9168338184225,235.774294480936,52.3605146379828));
#33450=CARTESIAN_POINT('Ctrl Pts',(82.9111139440083,235.721667776361,53.0156317204369));
#33451=CARTESIAN_POINT('Origin',(74.9879498948689,255.,53.0228109606356));
#33452=CARTESIAN_POINT('',(82.9129498948689,230.278332223638,53.0228109606318));
#33453=CARTESIAN_POINT('',(82.9064065954961,231.721667776361,53.0236012027229));
#33454=CARTESIAN_POINT('',(82.9129498948689,255.,53.0228109606356));
#33455=CARTESIAN_POINT('Ctrl Pts',(82.9129498948689,230.278332223638,53.0228109606318));
#33456=CARTESIAN_POINT('Ctrl Pts',(82.9129498948678,230.455428795637,50.8182135007218));
#33457=CARTESIAN_POINT('Ctrl Pts',(81.9432795991084,230.632525367636,48.6308565362859));
#33458=CARTESIAN_POINT('Ctrl Pts',(80.3096882702511,230.809621939634,47.1504412801757));
#33459=CARTESIAN_POINT('Ctrl Pts',(78.6760969413938,230.986718511633,45.6700260240655));
#33460=CARTESIAN_POINT('Ctrl Pts',(76.4041347530399,231.163815083632,44.9197069006022));
#33461=CARTESIAN_POINT('Ctrl Pts',(74.2101800112173,231.340911655631,45.1360689838695));
#33462=CARTESIAN_POINT('Ctrl Pts',(72.0162252693947,231.518008227629,45.3524310671367));
#33463=CARTESIAN_POINT('Ctrl Pts',(69.9345925076938,231.695104799628,46.5320903475045));
#33464=CARTESIAN_POINT('Ctrl Pts',(68.6216467656577,231.872201371627,48.3030853894826));
#33465=CARTESIAN_POINT('Ctrl Pts',(67.3087010236216,232.049297943626,50.0740804314606));
#33466=CARTESIAN_POINT('Ctrl Pts',(66.7849774198234,232.226394515624,52.4087119996463));
#33467=CARTESIAN_POINT('Ctrl Pts',(67.2156126057616,232.403491087623,54.5708413428803));
#33468=CARTESIAN_POINT('Ctrl Pts',(67.6462477916998,232.580587659622,56.7329706861143));
#33469=CARTESIAN_POINT('Ctrl Pts',(69.0245064208007,232.757684231621,58.6887810357273));
#33470=CARTESIAN_POINT('Ctrl Pts',(70.9158061804516,232.934780803619,59.8215807441428));
#33471=CARTESIAN_POINT('Ctrl Pts',(72.8071059401024,233.111877375618,60.9543804525583));
#33472=CARTESIAN_POINT('Ctrl Pts',(75.1818659698165,233.288973947617,61.2464519739653));
#33473=CARTESIAN_POINT('Ctrl Pts',(77.2912945088727,233.466070519615,60.6057014773937));
#33474=CARTESIAN_POINT('Ctrl Pts',(79.4007230479289,233.643167091614,59.9649509808221));
#33475=CARTESIAN_POINT('Ctrl Pts',(81.2118275942122,233.820263663613,58.4014001198723));
#33476=CARTESIAN_POINT('Ctrl Pts',(82.1535440633128,233.997360235612,56.4080561826487));
#33477=CARTESIAN_POINT('Ctrl Pts',(82.6515697929926,234.091017564954,55.353878411088));
#33478=CARTESIAN_POINT('Ctrl Pts',(82.9129498948694,234.184674894296,54.1887099277281));
#33479=CARTESIAN_POINT('Ctrl Pts',(82.9129498948689,234.278332223638,53.0228109606319));
#33480=CARTESIAN_POINT('Ctrl Pts',(82.9111139440083,235.721667776361,53.0156317204369));
#33481=CARTESIAN_POINT('Ctrl Pts',(82.8937750739949,235.562138471383,55.0015127230071));
#33482=CARTESIAN_POINT('Ctrl Pts',(82.1383239120666,235.402609166406,56.9995232239856));
#33483=CARTESIAN_POINT('Ctrl Pts',(80.7878565684763,235.243079861428,58.4436494368539));
#33484=CARTESIAN_POINT('Ctrl Pts',(78.9918870900964,235.030923851876,60.3641746635835));
#33485=CARTESIAN_POINT('Ctrl Pts',(76.1435717277343,234.818767842324,61.3050998915916));
#33486=CARTESIAN_POINT('Ctrl Pts',(73.5592434434874,234.606611832771,60.8321220369526));
#33487=CARTESIAN_POINT('Ctrl Pts',(70.9749151592408,234.394455823219,60.3591441823135));
#33488=CARTESIAN_POINT('Ctrl Pts',(68.6545739531097,234.182299813667,58.4722632450275));
#33489=CARTESIAN_POINT('Ctrl Pts',(67.6491982592205,233.970143804114,56.0409790947974));
#33490=CARTESIAN_POINT('Ctrl Pts',(67.1465104122758,233.864065799338,54.8253370196822));
#33491=CARTESIAN_POINT('Ctrl Pts',(66.9725639433917,233.757987794562,53.4735941413305));
#33492=CARTESIAN_POINT('Ctrl Pts',(67.1174189961907,233.651909789786,52.156924613021));
#33493=CARTESIAN_POINT('Ctrl Pts',(67.2622740489897,233.54583178501,50.8402550847114));
#33494=CARTESIAN_POINT('Ctrl Pts',(67.7259306234716,233.439753780233,49.5586589064437));
#33495=CARTESIAN_POINT('Ctrl Pts',(68.4808773747036,233.333675775457,48.4813770821003));
#33496=CARTESIAN_POINT('Ctrl Pts',(69.9907708771672,233.121519765905,46.3268134334138));
#33497=CARTESIAN_POINT('Ctrl Pts',(72.66582508663,232.909363756353,44.9895072004247));
#33498=CARTESIAN_POINT('Ctrl Pts',(75.291168219243,232.697207746801,45.0896778936393));
#33499=CARTESIAN_POINT('Ctrl Pts',(77.9165113518563,232.485051737248,45.1898485868539));
#33500=CARTESIAN_POINT('Ctrl Pts',(80.4921434076196,232.272895727696,46.7274962062725));
#33501=CARTESIAN_POINT('Ctrl Pts',(81.8276330377482,232.060739718143,48.9925328420896));
#33502=CARTESIAN_POINT('Ctrl Pts',(82.5391017081758,231.947715737549,50.1992083320366));
#33503=CARTESIAN_POINT('Ctrl Pts',(82.8986032654198,231.834691756955,51.6123254426967));
#33504=CARTESIAN_POINT('Ctrl Pts',(82.9002267075262,231.721667776361,53.0243475551716));
#33505=CARTESIAN_POINT('Origin',(74.9879498948689,255.,53.0228109606356));
#33506=CARTESIAN_POINT('',(82.9129498948689,226.278332223638,53.0228109606316));
#33507=CARTESIAN_POINT('',(82.9129498948689,227.721667776361,53.022810960645));
#33508=CARTESIAN_POINT('',(82.9129498948689,255.,53.0228109606356));
#33509=CARTESIAN_POINT('Ctrl Pts',(82.9129498948689,226.278332223638,53.0228109606311));
#33510=CARTESIAN_POINT('Ctrl Pts',(82.9129498948677,226.455428795637,50.8182135007215));
#33511=CARTESIAN_POINT('Ctrl Pts',(81.9432795991084,226.632525367636,48.6308565362859));
#33512=CARTESIAN_POINT('Ctrl Pts',(80.3096882702513,226.809621939634,47.1504412801759));
#33513=CARTESIAN_POINT('Ctrl Pts',(78.6760969413943,226.986718511633,45.6700260240659));
#33514=CARTESIAN_POINT('Ctrl Pts',(76.4041347530408,227.163815083632,44.9197069006025));
#33515=CARTESIAN_POINT('Ctrl Pts',(74.2101800112185,227.34091165563,45.1360689838694));
#33516=CARTESIAN_POINT('Ctrl Pts',(72.0162252693962,227.518008227629,45.3524310671362));
#33517=CARTESIAN_POINT('Ctrl Pts',(69.9345925076953,227.695104799628,46.5320903475034));
#33518=CARTESIAN_POINT('Ctrl Pts',(68.621646765659,227.872201371627,48.3030853894809));
#33519=CARTESIAN_POINT('Ctrl Pts',(67.3087010236226,228.049297943625,50.0740804314583));
#33520=CARTESIAN_POINT('Ctrl Pts',(66.7849774198237,228.226394515624,52.4087119996435));
#33521=CARTESIAN_POINT('Ctrl Pts',(67.2156126057611,228.403491087623,54.5708413428774));
#33522=CARTESIAN_POINT('Ctrl Pts',(67.6462477916984,228.580587659622,56.7329706861112));
#33523=CARTESIAN_POINT('Ctrl Pts',(69.0245064207982,228.75768423162,58.6887810357246));
#33524=CARTESIAN_POINT('Ctrl Pts',(70.9158061804482,228.934780803619,59.8215807441408));
#33525=CARTESIAN_POINT('Ctrl Pts',(72.8071059400983,229.111877375618,60.9543804525571));
#33526=CARTESIAN_POINT('Ctrl Pts',(75.1818659698118,229.288973947616,61.2464519739653));
#33527=CARTESIAN_POINT('Ctrl Pts',(77.2912945088681,229.466070519615,60.6057014773951));
#33528=CARTESIAN_POINT('Ctrl Pts',(79.4007230479244,229.643167091614,59.9649509808248));
#33529=CARTESIAN_POINT('Ctrl Pts',(81.2118275942084,229.820263663613,58.4014001198765));
#33530=CARTESIAN_POINT('Ctrl Pts',(82.1535440633104,229.997360235611,56.4080561826539));
#33531=CARTESIAN_POINT('Ctrl Pts',(82.6515697929918,230.091017564954,55.3538784110917));
#33532=CARTESIAN_POINT('Ctrl Pts',(82.9129498948695,230.184674894296,54.1887099277299));
#33533=CARTESIAN_POINT('Ctrl Pts',(82.9129498948689,230.278332223638,53.0228109606318));
#33534=CARTESIAN_POINT('Ctrl Pts',(82.9129498948689,231.721667776361,53.0228109606451));
#33535=CARTESIAN_POINT('Ctrl Pts',(82.9129498948662,231.544571204362,55.227408420555));
#33536=CARTESIAN_POINT('Ctrl Pts',(81.9432795991054,231.367474632363,57.4147653849901));
#33537=CARTESIAN_POINT('Ctrl Pts',(80.3096882702472,231.190378060365,58.895180641099));
#33538=CARTESIAN_POINT('Ctrl Pts',(78.676096941389,231.013281488366,60.375595897208));
#33539=CARTESIAN_POINT('Ctrl Pts',(76.4041347530348,230.836184916367,61.1259150206698));
#33540=CARTESIAN_POINT('Ctrl Pts',(74.2101800112125,230.659088344369,60.9095529374012));
#33541=CARTESIAN_POINT('Ctrl Pts',(72.0162252693902,230.48199177237,60.6931908541326));
#33542=CARTESIAN_POINT('Ctrl Pts',(69.9345925076901,230.304895200371,59.5135315737637));
#33543=CARTESIAN_POINT('Ctrl Pts',(68.6216467656551,230.127798628372,57.742536531785));
#33544=CARTESIAN_POINT('Ctrl Pts',(67.30870102362,229.950702056374,55.9715414898064));
#33545=CARTESIAN_POINT('Ctrl Pts',(66.7849774198232,229.773605484375,53.6369099216206));
#33546=CARTESIAN_POINT('Ctrl Pts',(67.2156126057624,229.596508912376,51.474780578387));
#33547=CARTESIAN_POINT('Ctrl Pts',(67.6462477917017,229.419412340377,49.3126512351533));
#33548=CARTESIAN_POINT('Ctrl Pts',(69.0245064208034,229.242315768379,47.3568408855411));
#33549=CARTESIAN_POINT('Ctrl Pts',(70.9158061804546,229.06521919638,46.2240411771265));
#33550=CARTESIAN_POINT('Ctrl Pts',(72.8071059401058,228.888122624381,45.0912414687119));
#33551=CARTESIAN_POINT('Ctrl Pts',(75.1818659698198,228.711026052382,44.799169947306));
#33552=CARTESIAN_POINT('Ctrl Pts',(77.2912945088756,228.533929480384,45.4399204438784));
#33553=CARTESIAN_POINT('Ctrl Pts',(79.4007230479314,228.356832908385,46.0806709404508));
#33554=CARTESIAN_POINT('Ctrl Pts',(81.211827594214,228.179736336386,47.644221801401));
#33555=CARTESIAN_POINT('Ctrl Pts',(82.1535440633139,228.002639764388,49.6375657386248));
#33556=CARTESIAN_POINT('Ctrl Pts',(82.6515697929938,227.908982435045,50.6917435101865));
#33557=CARTESIAN_POINT('Ctrl Pts',(82.9129498948702,227.815325105703,51.8569119935475));
#33558=CARTESIAN_POINT('Ctrl Pts',(82.9129498948689,227.721667776361,53.0228109606445));
#33559=CARTESIAN_POINT('Origin',(74.9879498948689,255.,53.0228109606356));
#33560=CARTESIAN_POINT('',(82.9129498948689,222.278332223638,53.0228109606314));
#33561=CARTESIAN_POINT('',(82.9158285778574,223.721667776361,53.0209513109217));
#33562=CARTESIAN_POINT('',(82.9129498948689,255.,53.0228109606356));
#33563=CARTESIAN_POINT('Ctrl Pts',(82.9129498948689,222.278332223638,53.022810960631));
#33564=CARTESIAN_POINT('Ctrl Pts',(82.9129498948676,222.455428795637,50.8182135007211));
#33565=CARTESIAN_POINT('Ctrl Pts',(81.9432795991081,222.632525367636,48.6308565362855));
#33566=CARTESIAN_POINT('Ctrl Pts',(80.3096882702508,222.809621939634,47.1504412801755));
#33567=CARTESIAN_POINT('Ctrl Pts',(78.6760969413936,222.986718511633,45.6700260240655));
#33568=CARTESIAN_POINT('Ctrl Pts',(76.4041347530399,223.163815083632,44.9197069006023));
#33569=CARTESIAN_POINT('Ctrl Pts',(74.2101800112174,223.340911655631,45.1360689838695));
#33570=CARTESIAN_POINT('Ctrl Pts',(72.016225269395,223.518008227629,45.3524310671366));
#33571=CARTESIAN_POINT('Ctrl Pts',(69.9345925076942,223.695104799628,46.5320903475043));
#33572=CARTESIAN_POINT('Ctrl Pts',(68.621646765658,223.872201371627,48.3030853894821));
#33573=CARTESIAN_POINT('Ctrl Pts',(67.3087010236219,224.049297943625,50.0740804314599));
#33574=CARTESIAN_POINT('Ctrl Pts',(66.7849774198236,224.226394515624,52.4087119996454));
#33575=CARTESIAN_POINT('Ctrl Pts',(67.2156126057615,224.403491087623,54.5708413428793));
#33576=CARTESIAN_POINT('Ctrl Pts',(67.6462477916993,224.580587659622,56.7329706861132));
#33577=CARTESIAN_POINT('Ctrl Pts',(69.0245064207998,224.75768423162,58.6887810357263));
#33578=CARTESIAN_POINT('Ctrl Pts',(70.9158061804503,224.934780803619,59.8215807441421));
#33579=CARTESIAN_POINT('Ctrl Pts',(72.8071059401008,225.111877375618,60.9543804525578));
#33580=CARTESIAN_POINT('Ctrl Pts',(75.1818659698146,225.288973947617,61.2464519739653));
#33581=CARTESIAN_POINT('Ctrl Pts',(77.2912945088708,225.466070519615,60.6057014773942));
#33582=CARTESIAN_POINT('Ctrl Pts',(79.400723047927,225.643167091614,59.9649509808232));
#33583=CARTESIAN_POINT('Ctrl Pts',(81.2118275942106,225.820263663613,58.4014001198741));
#33584=CARTESIAN_POINT('Ctrl Pts',(82.1535440633118,225.997360235611,56.4080561826509));
#33585=CARTESIAN_POINT('Ctrl Pts',(82.6515697929923,226.091017564954,55.3538784110893));
#33586=CARTESIAN_POINT('Ctrl Pts',(82.9129498948696,226.184674894296,54.1887099277284));
#33587=CARTESIAN_POINT('Ctrl Pts',(82.9129498948689,226.278332223638,53.0228109606311));
#33588=CARTESIAN_POINT('Ctrl Pts',(82.9129498948689,227.721667776361,53.0228109606445));
#33589=CARTESIAN_POINT('Ctrl Pts',(82.9129498948664,227.544571204362,55.2274084205545));
#33590=CARTESIAN_POINT('Ctrl Pts',(81.9432795991056,227.367474632363,57.4147653849898));
#33591=CARTESIAN_POINT('Ctrl Pts',(80.3096882702473,227.190378060365,58.8951806410989));
#33592=CARTESIAN_POINT('Ctrl Pts',(78.676096941389,227.013281488366,60.375595897208));
#33593=CARTESIAN_POINT('Ctrl Pts',(76.4041347530346,226.836184916367,61.1259150206698));
#33594=CARTESIAN_POINT('Ctrl Pts',(74.2101800112122,226.659088344369,60.9095529374012));
#33595=CARTESIAN_POINT('Ctrl Pts',(72.0162252693897,226.48199177237,60.6931908541325));
#33596=CARTESIAN_POINT('Ctrl Pts',(69.9345925076896,226.304895200371,59.5135315737633));
#33597=CARTESIAN_POINT('Ctrl Pts',(68.6216467656546,226.127798628372,57.7425365317845));
#33598=CARTESIAN_POINT('Ctrl Pts',(67.3087010236197,225.950702056374,55.9715414898056));
#33599=CARTESIAN_POINT('Ctrl Pts',(66.7849774198231,225.773605484375,53.6369099216195));
#33600=CARTESIAN_POINT('Ctrl Pts',(67.2156126057626,225.596508912376,51.4747805783858));
#33601=CARTESIAN_POINT('Ctrl Pts',(67.6462477917023,225.419412340377,49.3126512351521));
#33602=CARTESIAN_POINT('Ctrl Pts',(69.0245064208044,225.242315768379,47.3568408855399));
#33603=CARTESIAN_POINT('Ctrl Pts',(70.915806180456,225.06521919638,46.2240411771257));
#33604=CARTESIAN_POINT('Ctrl Pts',(72.8071059401075,224.888122624381,45.0912414687114));
#33605=CARTESIAN_POINT('Ctrl Pts',(75.1818659698218,224.711026052382,44.799169947306));
#33606=CARTESIAN_POINT('Ctrl Pts',(77.2912945088776,224.533929480384,45.439920443879));
#33607=CARTESIAN_POINT('Ctrl Pts',(79.4007230479334,224.356832908385,46.080670940452));
#33608=CARTESIAN_POINT('Ctrl Pts',(81.2118275942156,224.179736336386,47.6442218014028));
#33609=CARTESIAN_POINT('Ctrl Pts',(82.153544063315,224.002639764387,49.6375657386271));
#33610=CARTESIAN_POINT('Ctrl Pts',(82.6515697929941,223.908982435045,50.6917435101881));
#33611=CARTESIAN_POINT('Ctrl Pts',(82.9129498948702,223.815325105703,51.8569119935482));
#33612=CARTESIAN_POINT('Ctrl Pts',(82.9129498948689,223.721667776361,53.0228109606443));
#33613=CARTESIAN_POINT('Origin',(74.9879498948689,255.,53.0228109606356));
#33614=CARTESIAN_POINT('',(82.9088343949514,218.278332223638,53.0245926135986));
#33615=CARTESIAN_POINT('',(82.9093646881469,219.721667776361,53.0220566607781));
#33616=CARTESIAN_POINT('',(82.9129498948689,255.,53.0228109606356));
#33617=CARTESIAN_POINT('Ctrl Pts',(82.9129498948689,218.278332223638,53.0228109606313));
#33618=CARTESIAN_POINT('Ctrl Pts',(82.9129498948677,218.455428795637,50.8182135007216));
#33619=CARTESIAN_POINT('Ctrl Pts',(81.9432795991084,218.632525367636,48.630856536286));
#33620=CARTESIAN_POINT('Ctrl Pts',(80.3096882702514,218.809621939634,47.150441280176));
#33621=CARTESIAN_POINT('Ctrl Pts',(78.6760969413944,218.986718511633,45.6700260240659));
#33622=CARTESIAN_POINT('Ctrl Pts',(76.4041347530409,219.163815083632,44.9197069006025));
#33623=CARTESIAN_POINT('Ctrl Pts',(74.2101800112186,219.34091165563,45.1360689838693));
#33624=CARTESIAN_POINT('Ctrl Pts',(72.0162252693963,219.518008227629,45.3524310671362));
#33625=CARTESIAN_POINT('Ctrl Pts',(69.9345925076954,219.695104799628,46.5320903475034));
#33626=CARTESIAN_POINT('Ctrl Pts',(68.621646765659,219.872201371627,48.3030853894808));
#33627=CARTESIAN_POINT('Ctrl Pts',(67.3087010236226,220.049297943625,50.0740804314582));
#33628=CARTESIAN_POINT('Ctrl Pts',(66.7849774198237,220.226394515624,52.4087119996434));
#33629=CARTESIAN_POINT('Ctrl Pts',(67.215612605761,220.403491087623,54.5708413428773));
#33630=CARTESIAN_POINT('Ctrl Pts',(67.6462477916983,220.580587659622,56.7329706861111));
#33631=CARTESIAN_POINT('Ctrl Pts',(69.0245064207981,220.75768423162,58.6887810357245));
#33632=CARTESIAN_POINT('Ctrl Pts',(70.9158061804481,220.934780803619,59.8215807441408));
#33633=CARTESIAN_POINT('Ctrl Pts',(72.8071059400982,221.111877375618,60.9543804525571));
#33634=CARTESIAN_POINT('Ctrl Pts',(75.1818659698117,221.288973947616,61.2464519739653));
#33635=CARTESIAN_POINT('Ctrl Pts',(77.291294508868,221.466070519615,60.6057014773951));
#33636=CARTESIAN_POINT('Ctrl Pts',(79.4007230479243,221.643167091614,59.9649509808249));
#33637=CARTESIAN_POINT('Ctrl Pts',(81.2118275942083,221.820263663612,58.4014001198766));
#33638=CARTESIAN_POINT('Ctrl Pts',(82.1535440633103,221.997360235611,56.408056182654));
#33639=CARTESIAN_POINT('Ctrl Pts',(82.6515697929919,222.091017564954,55.3538784110915));
#33640=CARTESIAN_POINT('Ctrl Pts',(82.9129498948696,222.184674894296,54.1887099277294));
#33641=CARTESIAN_POINT('Ctrl Pts',(82.9129498948689,222.278332223638,53.022810960631));
#33642=CARTESIAN_POINT('Ctrl Pts',(82.9234447883723,223.721667776361,53.0160311846121));
#33643=CARTESIAN_POINT('Ctrl Pts',(82.907270754594,223.531174289889,55.3785973853056));
#33644=CARTESIAN_POINT('Ctrl Pts',(81.7821471756311,223.340680803418,57.758561145984));
#33645=CARTESIAN_POINT('Ctrl Pts',(79.9363556092803,223.150187316946,59.230684047091));
#33646=CARTESIAN_POINT('Ctrl Pts',(77.8806644650022,222.938031307394,60.8702137026943));
#33647=CARTESIAN_POINT('Ctrl Pts',(74.9310800947544,222.725875297841,61.3836869650193));
#33648=CARTESIAN_POINT('Ctrl Pts',(72.4412170677322,222.513719288289,60.5401705955808));
#33649=CARTESIAN_POINT('Ctrl Pts',(69.9513540407098,222.301563278737,59.6966542261423));
#33650=CARTESIAN_POINT('Ctrl Pts',(67.9212123569129,222.089407269185,57.4961482249402));
#33651=CARTESIAN_POINT('Ctrl Pts',(67.285320134102,221.877251259632,54.944763374811));
#33652=CARTESIAN_POINT('Ctrl Pts',(66.6494279112911,221.66509525008,52.3933785246817));
#33653=CARTESIAN_POINT('Ctrl Pts',(67.407785149466,221.452939240528,49.4911148256255));
#33654=CARTESIAN_POINT('Ctrl Pts',(69.2094682792691,221.240783230975,47.5789435076261));
#33655=CARTESIAN_POINT('Ctrl Pts',(71.0111514090722,221.028627221423,45.6667721896267));
#33656=CARTESIAN_POINT('Ctrl Pts',(73.8561604305038,220.816471211871,44.7446932526844));
#33657=CARTESIAN_POINT('Ctrl Pts',(76.4434042330216,220.604315202319,45.2222810130445));
#33658=CARTESIAN_POINT('Ctrl Pts',(77.7370261342805,220.498237197542,45.4610748932245));
#33659=CARTESIAN_POINT('Ctrl Pts',(78.9662067308111,220.392159192766,46.0497854477303));
#33660=CARTESIAN_POINT('Ctrl Pts',(79.992668284066,220.28608118799,46.8870301906149));
#33661=CARTESIAN_POINT('Ctrl Pts',(81.0191298373208,220.180003183214,47.7242749334995));
#33662=CARTESIAN_POINT('Ctrl Pts',(81.8428723473001,220.073925178438,48.8100538647629));
#33663=CARTESIAN_POINT('Ctrl Pts',(82.336788967223,219.967847173662,50.0292860659892));
#33664=CARTESIAN_POINT('Ctrl Pts',(82.7188728750852,219.885787374561,50.9724594382655));
#33665=CARTESIAN_POINT('Ctrl Pts',(82.9035805041128,219.803727575461,51.995494672869));
#33666=CARTESIAN_POINT('Ctrl Pts',(82.8989973990194,219.721667776361,53.0198754630378));
#33667=CARTESIAN_POINT('Origin',(74.9879498948689,255.,53.0228109606356));
#33668=CARTESIAN_POINT('',(82.9155886507495,214.278332223638,53.0240128735546));
#33669=CARTESIAN_POINT('',(82.9129498948689,215.721667776361,53.0228109606445));
#33670=CARTESIAN_POINT('',(82.9129498948689,255.,53.0228109606356));
#33671=CARTESIAN_POINT('Ctrl Pts',(82.9225333537804,214.278332223638,53.0271760795405));
#33672=CARTESIAN_POINT('Ctrl Pts',(82.906990815689,214.469208481852,50.6594335019644));
#33673=CARTESIAN_POINT('Ctrl Pts',(81.7792862151741,214.660084740066,48.278630556164));
#33674=CARTESIAN_POINT('Ctrl Pts',(79.9265027100333,214.85096099828,46.8074088927466));
#33675=CARTESIAN_POINT('Ctrl Pts',(77.8671624930109,215.063117007833,45.1721687628427));
#33676=CARTESIAN_POINT('Ctrl Pts',(74.912061336723,215.275273017385,44.6606234179444));
#33677=CARTESIAN_POINT('Ctrl Pts',(72.4256081920683,215.487429026937,45.5088026735112));
#33678=CARTESIAN_POINT('Ctrl Pts',(69.9391550474136,215.69958503649,46.3569819290781));
#33679=CARTESIAN_POINT('Ctrl Pts',(67.9213499143921,215.911741046042,48.5648857851099));
#33680=CARTESIAN_POINT('Ctrl Pts',(67.2847849840505,216.123897055594,51.1176627810452));
#33681=CARTESIAN_POINT('Ctrl Pts',(66.9665025188798,216.22997506037,52.3940512790129));
#33682=CARTESIAN_POINT('Ctrl Pts',(66.993530104379,216.336053065147,53.7566580619564));
#33683=CARTESIAN_POINT('Ctrl Pts',(67.3306293105148,216.442131069923,55.0376640357496));
#33684=CARTESIAN_POINT('Ctrl Pts',(67.6677285166505,216.548209074699,56.318670009543));
#33685=CARTESIAN_POINT('Ctrl Pts',(68.3148993434228,216.654287079475,57.5180751741862));
#33686=CARTESIAN_POINT('Ctrl Pts',(69.2201496857532,216.760365084251,58.4725139703031));
#33687=CARTESIAN_POINT('Ctrl Pts',(71.0306503704139,216.972521093803,60.3813915625367));
#33688=CARTESIAN_POINT('Ctrl Pts',(73.8734691173067,217.184677103356,61.3104036806656));
#33689=CARTESIAN_POINT('Ctrl Pts',(76.4554961749134,217.396833112908,60.8249171391498));
#33690=CARTESIAN_POINT('Ctrl Pts',(79.0375232325201,217.60898912246,60.3394305976341));
#33691=CARTESIAN_POINT('Ctrl Pts',(81.3587586008407,217.821145132013,58.4394453964739));
#33692=CARTESIAN_POINT('Ctrl Pts',(82.3463226381038,218.033301141565,56.0025168924015));
#33693=CARTESIAN_POINT('Ctrl Pts',(82.7265206586982,218.114978168923,55.0643342950013));
#33694=CARTESIAN_POINT('Ctrl Pts',(82.9090499430764,218.19665519628,54.0465691935503));
#33695=CARTESIAN_POINT('Ctrl Pts',(82.9032295534682,218.278332223638,53.0270190217289));
#33696=CARTESIAN_POINT('Ctrl Pts',(82.9129498948689,219.721667776361,53.0228109606442));
#33697=CARTESIAN_POINT('Ctrl Pts',(82.9129498948665,219.544571204362,55.2274084205539));
#33698=CARTESIAN_POINT('Ctrl Pts',(81.943279599106,219.367474632364,57.4147653849889));
#33699=CARTESIAN_POINT('Ctrl Pts',(80.3096882702482,219.190378060365,58.8951806410981));
#33700=CARTESIAN_POINT('Ctrl Pts',(78.6760969413904,219.013281488366,60.3755958972072));
#33701=CARTESIAN_POINT('Ctrl Pts',(76.4041347530365,218.836184916367,61.1259150206694));
#33702=CARTESIAN_POINT('Ctrl Pts',(74.2101800112143,218.659088344369,60.9095529374014));
#33703=CARTESIAN_POINT('Ctrl Pts',(72.0162252693921,218.48199177237,60.6931908541333));
#33704=CARTESIAN_POINT('Ctrl Pts',(69.9345925076919,218.304895200371,59.513531573765));
#33705=CARTESIAN_POINT('Ctrl Pts',(68.6216467656565,218.127798628373,57.7425365317869));
#33706=CARTESIAN_POINT('Ctrl Pts',(67.308701023621,217.950702056374,55.9715414898088));
#33707=CARTESIAN_POINT('Ctrl Pts',(66.7849774198234,217.773605484375,53.6369099216233));
#33708=CARTESIAN_POINT('Ctrl Pts',(67.2156126057619,217.596508912376,51.4747805783897));
#33709=CARTESIAN_POINT('Ctrl Pts',(67.6462477917003,217.419412340378,49.312651235156));
#33710=CARTESIAN_POINT('Ctrl Pts',(69.0245064208012,217.242315768379,47.3568408855434));
#33711=CARTESIAN_POINT('Ctrl Pts',(70.9158061804518,217.06521919638,46.2240411771282));
#33712=CARTESIAN_POINT('Ctrl Pts',(72.8071059401024,216.888122624381,45.0912414687129));
#33713=CARTESIAN_POINT('Ctrl Pts',(75.1818659698161,216.711026052383,44.7991699473059));
#33714=CARTESIAN_POINT('Ctrl Pts',(77.2912945088721,216.533929480384,45.4399204438773));
#33715=CARTESIAN_POINT('Ctrl Pts',(79.4007230479281,216.356832908385,46.0806709404487));
#33716=CARTESIAN_POINT('Ctrl Pts',(81.2118275942113,216.179736336387,47.6442218013979));
#33717=CARTESIAN_POINT('Ctrl Pts',(82.1535440633122,216.002639764388,49.637565738621));
#33718=CARTESIAN_POINT('Ctrl Pts',(82.6515697929931,215.908982435046,50.6917435101838));
#33719=CARTESIAN_POINT('Ctrl Pts',(82.9129498948702,215.815325105703,51.856911993546));
#33720=CARTESIAN_POINT('Ctrl Pts',(82.9129498948689,215.721667776361,53.0228109606445));
#33721=CARTESIAN_POINT('Origin',(74.9879498948689,255.,53.0228109606356));
#33722=CARTESIAN_POINT('',(82.9128963053489,210.278332223638,53.0220763034151));
#33723=CARTESIAN_POINT('',(82.9259067049454,211.721667776361,53.0240434941313));
#33724=CARTESIAN_POINT('',(82.9129498948689,255.,53.0228109606356));
#33725=CARTESIAN_POINT('Ctrl Pts',(82.9129498948689,210.278332223638,53.0228109606305));
#33726=CARTESIAN_POINT('Ctrl Pts',(82.9129498948675,210.455428795637,50.8182135007206));
#33727=CARTESIAN_POINT('Ctrl Pts',(81.9432795991078,210.632525367636,48.630856536285));
#33728=CARTESIAN_POINT('Ctrl Pts',(80.3096882702505,210.809621939634,47.1504412801751));
#33729=CARTESIAN_POINT('Ctrl Pts',(78.6760969413931,210.986718511633,45.6700260240652));
#33730=CARTESIAN_POINT('Ctrl Pts',(76.4041347530393,211.163815083632,44.9197069006022));
#33731=CARTESIAN_POINT('Ctrl Pts',(74.2101800112169,211.340911655631,45.1360689838695));
#33732=CARTESIAN_POINT('Ctrl Pts',(72.0162252693945,211.518008227629,45.3524310671368));
#33733=CARTESIAN_POINT('Ctrl Pts',(69.9345925076938,211.695104799628,46.5320903475046));
#33734=CARTESIAN_POINT('Ctrl Pts',(68.6216467656577,211.872201371627,48.3030853894825));
#33735=CARTESIAN_POINT('Ctrl Pts',(67.3087010236217,212.049297943626,50.0740804314604));
#33736=CARTESIAN_POINT('Ctrl Pts',(66.7849774198235,212.226394515624,52.4087119996459));
#33737=CARTESIAN_POINT('Ctrl Pts',(67.2156126057615,212.403491087623,54.5708413428798));
#33738=CARTESIAN_POINT('Ctrl Pts',(67.6462477916996,212.580587659622,56.7329706861137));
#33739=CARTESIAN_POINT('Ctrl Pts',(69.0245064208002,212.75768423162,58.6887810357267));
#33740=CARTESIAN_POINT('Ctrl Pts',(70.9158061804508,212.934780803619,59.8215807441423));
#33741=CARTESIAN_POINT('Ctrl Pts',(72.8071059401013,213.111877375618,60.954380452558));
#33742=CARTESIAN_POINT('Ctrl Pts',(75.1818659698152,213.288973947617,61.2464519739653));
#33743=CARTESIAN_POINT('Ctrl Pts',(77.2912945088713,213.466070519615,60.6057014773941));
#33744=CARTESIAN_POINT('Ctrl Pts',(79.4007230479275,213.643167091614,59.9649509808229));
#33745=CARTESIAN_POINT('Ctrl Pts',(81.2118275942109,213.820263663613,58.4014001198737));
#33746=CARTESIAN_POINT('Ctrl Pts',(82.153544063312,213.997360235612,56.4080561826504));
#33747=CARTESIAN_POINT('Ctrl Pts',(82.6515697929924,214.091017564954,55.3538784110889));
#33748=CARTESIAN_POINT('Ctrl Pts',(82.9129498948696,214.184674894296,54.1887099277282));
#33749=CARTESIAN_POINT('Ctrl Pts',(82.9129498948689,214.278332223638,53.0228109606311));
#33750=CARTESIAN_POINT('Ctrl Pts',(82.9100628360345,215.721667776361,53.0273218344214));
#33751=CARTESIAN_POINT('Ctrl Pts',(82.9145791607339,215.651968841928,53.8964065984667));
#33752=CARTESIAN_POINT('Ctrl Pts',(82.7796363005651,215.582269907496,54.7639078768016));
#33753=CARTESIAN_POINT('Ctrl Pts',(82.4993576186766,215.512570973063,55.581539792728));
#33754=CARTESIAN_POINT('Ctrl Pts',(81.6462196590214,215.300414963511,58.0703228132649));
#33755=CARTESIAN_POINT('Ctrl Pts',(79.4465050799532,215.088258953958,60.097052386485));
#33756=CARTESIAN_POINT('Ctrl Pts',(76.8964746196261,214.876102944406,60.7288766829011));
#33757=CARTESIAN_POINT('Ctrl Pts',(74.346444159299,214.663946934854,61.3607009793171));
#33758=CARTESIAN_POINT('Ctrl Pts',(71.446097817713,214.451790925301,60.597619998929));
#33759=CARTESIAN_POINT('Ctrl Pts',(69.5345770260846,214.239634915749,58.7918014379804));
#33760=CARTESIAN_POINT('Ctrl Pts',(67.6230562344562,214.027478906197,56.9859828770317));
#33761=CARTESIAN_POINT('Ctrl Pts',(66.7003609927855,213.815322896644,54.1374267355225));
#33762=CARTESIAN_POINT('Ctrl Pts',(67.1874014817734,213.603166887092,51.5539497122178));
#33763=CARTESIAN_POINT('Ctrl Pts',(67.6744419707613,213.39101087754,48.9704726889132));
#33764=CARTESIAN_POINT('Ctrl Pts',(69.5712181904076,213.178854867988,46.6520747838132));
#33765=CARTESIAN_POINT('Ctrl Pts',(72.0073869599948,212.966698858435,45.6651863848547));
#33766=CARTESIAN_POINT('Ctrl Pts',(74.4435557295822,212.754542848883,44.6782979858962));
#33767=CARTESIAN_POINT('Ctrl Pts',(77.4191170491105,212.54238683933,45.0229190930795));
#33768=CARTESIAN_POINT('Ctrl Pts',(79.5668964072261,212.330230829778,46.5390344569979));
#33769=CARTESIAN_POINT('Ctrl Pts',(81.6205096374134,212.127376478639,47.9886780426244));
#33770=CARTESIAN_POINT('Ctrl Pts',(82.9173353903022,211.9245221275,50.5093430137754));
#33771=CARTESIAN_POINT('Ctrl Pts',(82.9259067049454,211.721667776361,53.0240434941313));
#33772=CARTESIAN_POINT('Origin',(74.9879498948689,255.,53.0228109606356));
#33773=CARTESIAN_POINT('',(82.910875927569,206.278332223638,53.0225169327894));
#33774=CARTESIAN_POINT('',(82.9116710970601,207.721667776361,53.0156229854146));
#33775=CARTESIAN_POINT('',(82.9129498948689,255.,53.0228109606356));
#33776=CARTESIAN_POINT('Ctrl Pts',(82.9061037343352,206.278332223638,53.0218403755537));
#33777=CARTESIAN_POINT('Ctrl Pts',(82.9073297587047,206.377847024339,51.7792408097306));
#33778=CARTESIAN_POINT('Ctrl Pts',(82.6266185356372,206.47736182504,50.5372467636587));
#33779=CARTESIAN_POINT('Ctrl Pts',(82.0668914032528,206.57687662574,49.4373940912735));
#33780=CARTESIAN_POINT('Ctrl Pts',(80.8736068464957,206.789032635293,47.0926136925203));
#33781=CARTESIAN_POINT('Ctrl Pts',(78.4121907958689,207.001188644845,45.3938679696944));
#33782=CARTESIAN_POINT('Ctrl Pts',(75.7986914495842,207.213344654397,45.1253922903185));
#33783=CARTESIAN_POINT('Ctrl Pts',(73.1851921032995,207.425500663949,44.8569166109425));
#33784=CARTESIAN_POINT('Ctrl Pts',(70.4196094613566,207.637656673502,46.0187109750167));
#33785=CARTESIAN_POINT('Ctrl Pts',(68.780078490162,207.849812683054,48.0744034917667));
#33786=CARTESIAN_POINT('Ctrl Pts',(67.1405475189675,208.061968692606,50.1300960085167));
#33787=CARTESIAN_POINT('Ctrl Pts',(66.6270682185208,208.274124702159,53.0796866779427));
#33788=CARTESIAN_POINT('Ctrl Pts',(67.4705872150538,208.486280711711,55.5695469642904));
#33789=CARTESIAN_POINT('Ctrl Pts',(68.3141062115868,208.698436721263,58.0594072506382));
#33790=CARTESIAN_POINT('Ctrl Pts',(70.5146235050995,208.910592730815,60.0895371539075));
#33791=CARTESIAN_POINT('Ctrl Pts',(73.0660029762825,209.122748740368,60.7254349882198));
#33792=CARTESIAN_POINT('Ctrl Pts',(75.6173824474655,209.33490474992,61.3613328225322));
#33793=CARTESIAN_POINT('Ctrl Pts',(78.5196240963186,209.547060759473,60.6029985878876));
#33794=CARTESIAN_POINT('Ctrl Pts',(80.4318085557769,209.759216769025,58.8013017484574));
#33795=CARTESIAN_POINT('Ctrl Pts',(81.9914226452245,209.932255253896,57.3318034676876));
#33796=CARTESIAN_POINT('Ctrl Pts',(82.8924165854151,210.105293738767,55.1682244390036));
#33797=CARTESIAN_POINT('Ctrl Pts',(82.9124953745832,210.278332223638,53.0165799548811));
#33798=CARTESIAN_POINT('Ctrl Pts',(82.9259067049454,211.721667776361,53.0240434941313));
#33799=CARTESIAN_POINT('Ctrl Pts',(82.9262997329505,211.712366117948,53.1393522599951));
#33800=CARTESIAN_POINT('Ctrl Pts',(82.9239841054999,211.703064459535,53.2546484850516));
#33801=CARTESIAN_POINT('Ctrl Pts',(82.9189085831446,211.693762801121,53.3698283356355));
#33802=CARTESIAN_POINT('Ctrl Pts',(82.8031440042447,211.481606791569,55.9968972297008));
#33803=CARTESIAN_POINT('Ctrl Pts',(81.2516174497423,211.269450782017,58.563425397178));
#33804=CARTESIAN_POINT('Ctrl Pts',(78.9808078930308,211.057294772464,59.8845163279184));
#33805=CARTESIAN_POINT('Ctrl Pts',(76.7099983363191,210.845138762912,61.205607258659));
#33806=CARTESIAN_POINT('Ctrl Pts',(73.7199057773981,210.63298275336,61.2812609526625));
#33807=CARTESIAN_POINT('Ctrl Pts',(71.3751524852751,210.420826743807,60.0879389925039));
#33808=CARTESIAN_POINT('Ctrl Pts',(70.2027758392138,210.314748739031,59.4912780124247));
#33809=CARTESIAN_POINT('Ctrl Pts',(69.1917340098519,210.208670734255,58.5773731188052));
#33810=CARTESIAN_POINT('Ctrl Pts',(68.4456231577739,210.102592729479,57.4828728784752));
#33811=CARTESIAN_POINT('Ctrl Pts',(67.6995123056957,209.996514724703,56.3883726381449));
#33812=CARTESIAN_POINT('Ctrl Pts',(67.2183324309016,209.890436719926,55.1132770511039));
#33813=CARTESIAN_POINT('Ctrl Pts',(67.0913314365078,209.78435871515,53.8039633586506));
#33814=CARTESIAN_POINT('Ctrl Pts',(66.8373294477203,209.572202705598,51.1853359737447));
#33815=CARTESIAN_POINT('Ctrl Pts',(68.0000429805332,209.360046696046,48.4298361671897));
#33816=CARTESIAN_POINT('Ctrl Pts',(70.05969095471,209.147890686494,46.7987594888346));
#33817=CARTESIAN_POINT('Ctrl Pts',(72.1193389288871,208.935734676941,45.1676828104792));
#33818=CARTESIAN_POINT('Ctrl Pts',(75.0759213444285,208.723578667389,44.6610292603245));
#33819=CARTESIAN_POINT('Ctrl Pts',(77.5633691966018,208.511422657836,45.5133827341697));
#33820=CARTESIAN_POINT('Ctrl Pts',(80.050817048775,208.299266648284,46.3657362080148));
#33821=CARTESIAN_POINT('Ctrl Pts',(82.0691303375802,208.087110638732,48.5770967058599));
#33822=CARTESIAN_POINT('Ctrl Pts',(82.6960193572198,207.87495462918,51.1301221072413));
#33823=CARTESIAN_POINT('Ctrl Pts',(82.84699920312,207.823859011574,51.7449923148922));
#33824=CARTESIAN_POINT('Ctrl Pts',(82.9172711199504,207.772763393967,52.3796803936349));
#33825=CARTESIAN_POINT('Ctrl Pts',(82.9116710970601,207.721667776361,53.0156229854146));
#33826=CARTESIAN_POINT('Origin',(74.9879498948689,255.,53.0228109606356));
#33827=CARTESIAN_POINT('',(82.9129498948689,202.278332223638,53.0228109606306));
#33828=CARTESIAN_POINT('',(82.9084421270908,203.721667776361,53.0232477115732));
#33829=CARTESIAN_POINT('',(82.9129498948689,255.,53.0228109606356));
#33830=CARTESIAN_POINT('Ctrl Pts',(82.9129498948689,202.278332223638,53.0228109606301));
#33831=CARTESIAN_POINT('Ctrl Pts',(82.9129498948674,202.455428795637,50.8182135007201));
#33832=CARTESIAN_POINT('Ctrl Pts',(81.9432795991075,202.632525367636,48.6308565362844));
#33833=CARTESIAN_POINT('Ctrl Pts',(80.3096882702499,202.809621939634,47.1504412801746));
#33834=CARTESIAN_POINT('Ctrl Pts',(78.6760969413923,202.986718511633,45.6700260240648));
#33835=CARTESIAN_POINT('Ctrl Pts',(76.4041347530382,203.163815083632,44.9197069006019));
#33836=CARTESIAN_POINT('Ctrl Pts',(74.2101800112157,203.340911655631,45.1360689838696));
#33837=CARTESIAN_POINT('Ctrl Pts',(72.0162252693931,203.518008227629,45.3524310671373));
#33838=CARTESIAN_POINT('Ctrl Pts',(69.9345925076925,203.695104799628,46.5320903475056));
#33839=CARTESIAN_POINT('Ctrl Pts',(68.6216467656567,203.872201371627,48.3030853894839));
#33840=CARTESIAN_POINT('Ctrl Pts',(67.308701023621,204.049297943626,50.0740804314622));
#33841=CARTESIAN_POINT('Ctrl Pts',(66.7849774198233,204.226394515624,52.408711999648));
#33842=CARTESIAN_POINT('Ctrl Pts',(67.215612605762,204.403491087623,54.5708413428819));
#33843=CARTESIAN_POINT('Ctrl Pts',(67.6462477917006,204.580587659622,56.7329706861158));
#33844=CARTESIAN_POINT('Ctrl Pts',(69.0245064208019,204.757684231621,58.6887810357286));
#33845=CARTESIAN_POINT('Ctrl Pts',(70.915806180453,204.934780803619,59.8215807441437));
#33846=CARTESIAN_POINT('Ctrl Pts',(72.8071059401041,205.111877375618,60.9543804525588));
#33847=CARTESIAN_POINT('Ctrl Pts',(75.1818659698182,205.288973947617,61.2464519739652));
#33848=CARTESIAN_POINT('Ctrl Pts',(77.2912945088742,205.466070519616,60.6057014773932));
#33849=CARTESIAN_POINT('Ctrl Pts',(79.4007230479303,205.643167091614,59.9649509808211));
#33850=CARTESIAN_POINT('Ctrl Pts',(81.2118275942133,205.820263663613,58.4014001198711));
#33851=CARTESIAN_POINT('Ctrl Pts',(82.1535440633135,205.997360235612,56.4080561826472));
#33852=CARTESIAN_POINT('Ctrl Pts',(82.6515697929931,206.091017564954,55.3538784110864));
#33853=CARTESIAN_POINT('Ctrl Pts',(82.9129498948697,206.184674894296,54.1887099277265));
#33854=CARTESIAN_POINT('Ctrl Pts',(82.9129498948689,206.278332223638,53.0228109606303));
#33855=CARTESIAN_POINT('Ctrl Pts',(82.9116710970601,207.721667776361,53.0156229854146));
#33856=CARTESIAN_POINT('Ctrl Pts',(82.8940190571418,207.560607384415,55.0202012229607));
#33857=CARTESIAN_POINT('Ctrl Pts',(82.1225058291152,207.399546992469,57.0372442622787));
#33858=CARTESIAN_POINT('Ctrl Pts',(80.7485923473629,207.238486600523,58.4853563737063));
#33859=CARTESIAN_POINT('Ctrl Pts',(78.938811567392,207.02633059097,60.3928749338722));
#33860=CARTESIAN_POINT('Ctrl Pts',(76.0837852569762,206.814174581418,61.3132217492859));
#33861=CARTESIAN_POINT('Ctrl Pts',(73.5029374125956,206.602018571866,60.8216096790478));
#33862=CARTESIAN_POINT('Ctrl Pts',(70.9220895682152,206.389862562313,60.3299976088097));
#33863=CARTESIAN_POINT('Ctrl Pts',(68.6154201898701,206.177706552761,58.4264266529199));
#33864=CARTESIAN_POINT('Ctrl Pts',(67.6276125205348,205.965550543209,55.9879518918911));
#33865=CARTESIAN_POINT('Ctrl Pts',(67.1337086858671,205.859472538433,54.7687145113765));
#33866=CARTESIAN_POINT('Ctrl Pts',(66.969520278452,205.753394533656,53.4157511795768));
#33867=CARTESIAN_POINT('Ctrl Pts',(67.1238715200474,205.64731652888,52.1001609036867));
#33868=CARTESIAN_POINT('Ctrl Pts',(67.2782227616428,205.541238524104,50.7845706277968));
#33869=CARTESIAN_POINT('Ctrl Pts',(67.7511136522486,205.435160519328,49.5063534078162));
#33870=CARTESIAN_POINT('Ctrl Pts',(68.5138131866417,205.329082514552,48.4345467270829));
#33871=CARTESIAN_POINT('Ctrl Pts',(70.039212255428,205.116926504999,46.2909333656162));
#33872=CARTESIAN_POINT('Ctrl Pts',(72.7238458993632,204.904770495447,44.9729621611391));
#33873=CARTESIAN_POINT('Ctrl Pts',(75.3483980678444,204.692614485895,45.0920720453542));
#33874=CARTESIAN_POINT('Ctrl Pts',(77.9729502363255,204.480458476343,45.2111819295692));
#33875=CARTESIAN_POINT('Ctrl Pts',(80.5374209293524,204.26830246679,46.7673729024763));
#33876=CARTESIAN_POINT('Ctrl Pts',(81.8565334837811,204.056146457238,49.0419861973571));
#33877=CARTESIAN_POINT('Ctrl Pts',(82.5497576635792,203.944653563612,50.2373481324761));
#33878=CARTESIAN_POINT('Ctrl Pts',(82.8990455859946,203.833160669987,51.631120048613));
#33879=CARTESIAN_POINT('Ctrl Pts',(82.9001606972016,203.721667776361,53.0240500870242));
#33880=CARTESIAN_POINT('Origin',(74.9879498948689,255.,53.0228109606356));
#33881=CARTESIAN_POINT('',(82.9129498948689,198.278332223638,53.0228109606304));
#33882=CARTESIAN_POINT('',(82.9129498948689,199.721667776361,53.0228109606438));
#33883=CARTESIAN_POINT('',(82.9129498948689,255.,53.0228109606356));
#33884=CARTESIAN_POINT('Ctrl Pts',(82.9129498948689,198.278332223638,53.0228109606304));
#33885=CARTESIAN_POINT('Ctrl Pts',(82.9129498948675,198.455428795637,50.8182135007206));
#33886=CARTESIAN_POINT('Ctrl Pts',(81.9432795991078,198.632525367636,48.630856536285));
#33887=CARTESIAN_POINT('Ctrl Pts',(80.3096882702504,198.809621939634,47.1504412801751));
#33888=CARTESIAN_POINT('Ctrl Pts',(78.676096941393,198.986718511633,45.6700260240652));
#33889=CARTESIAN_POINT('Ctrl Pts',(76.4041347530393,199.163815083632,44.9197069006022));
#33890=CARTESIAN_POINT('Ctrl Pts',(74.2101800112168,199.340911655631,45.1360689838695));
#33891=CARTESIAN_POINT('Ctrl Pts',(72.0162252693944,199.518008227629,45.3524310671369));
#33892=CARTESIAN_POINT('Ctrl Pts',(69.9345925076937,199.695104799628,46.5320903475046));
#33893=CARTESIAN_POINT('Ctrl Pts',(68.6216467656577,199.872201371627,48.3030853894826));
#33894=CARTESIAN_POINT('Ctrl Pts',(67.3087010236217,200.049297943626,50.0740804314605));
#33895=CARTESIAN_POINT('Ctrl Pts',(66.7849774198235,200.226394515624,52.408711999646));
#33896=CARTESIAN_POINT('Ctrl Pts',(67.2156126057616,200.403491087623,54.5708413428799));
#33897=CARTESIAN_POINT('Ctrl Pts',(67.6462477916996,200.580587659622,56.7329706861138));
#33898=CARTESIAN_POINT('Ctrl Pts',(69.0245064208002,200.75768423162,58.6887810357267));
#33899=CARTESIAN_POINT('Ctrl Pts',(70.9158061804508,200.934780803619,59.8215807441424));
#33900=CARTESIAN_POINT('Ctrl Pts',(72.8071059401014,201.111877375618,60.954380452558));
#33901=CARTESIAN_POINT('Ctrl Pts',(75.1818659698152,201.288973947617,61.2464519739653));
#33902=CARTESIAN_POINT('Ctrl Pts',(77.2912945088714,201.466070519615,60.605701477394));
#33903=CARTESIAN_POINT('Ctrl Pts',(79.4007230479275,201.643167091614,59.9649509808228));
#33904=CARTESIAN_POINT('Ctrl Pts',(81.211827594211,201.820263663613,58.4014001198736));
#33905=CARTESIAN_POINT('Ctrl Pts',(82.153544063312,201.997360235612,56.4080561826503));
#33906=CARTESIAN_POINT('Ctrl Pts',(82.6515697929926,202.091017564954,55.3538784110886));
#33907=CARTESIAN_POINT('Ctrl Pts',(82.9129498948697,202.184674894296,54.1887099277275));
#33908=CARTESIAN_POINT('Ctrl Pts',(82.9129498948689,202.278332223638,53.0228109606301));
#33909=CARTESIAN_POINT('Ctrl Pts',(82.9129498948689,203.721667776361,53.0228109606435));
#33910=CARTESIAN_POINT('Ctrl Pts',(82.9129498948667,203.544571204362,55.2274084205535));
#33911=CARTESIAN_POINT('Ctrl Pts',(81.9432795991061,203.367474632364,57.4147653849889));
#33912=CARTESIAN_POINT('Ctrl Pts',(80.3096882702481,203.190378060365,58.8951806410982));
#33913=CARTESIAN_POINT('Ctrl Pts',(78.67609694139,203.013281488366,60.3755958972075));
#33914=CARTESIAN_POINT('Ctrl Pts',(76.4041347530357,202.836184916367,61.1259150206696));
#33915=CARTESIAN_POINT('Ctrl Pts',(74.2101800112132,202.659088344369,60.9095529374013));
#33916=CARTESIAN_POINT('Ctrl Pts',(72.0162252693907,202.48199177237,60.6931908541329));
#33917=CARTESIAN_POINT('Ctrl Pts',(69.9345925076904,202.304895200371,59.513531573764));
#33918=CARTESIAN_POINT('Ctrl Pts',(68.6216467656553,202.127798628372,57.7425365317853));
#33919=CARTESIAN_POINT('Ctrl Pts',(67.3087010236201,201.950702056374,55.9715414898066));
#33920=CARTESIAN_POINT('Ctrl Pts',(66.7849774198231,201.773605484375,53.6369099216206));
#33921=CARTESIAN_POINT('Ctrl Pts',(67.2156126057624,201.596508912376,51.4747805783868));
#33922=CARTESIAN_POINT('Ctrl Pts',(67.6462477917018,201.419412340377,49.312651235153));
#33923=CARTESIAN_POINT('Ctrl Pts',(69.0245064208037,201.242315768379,47.3568408855407));
#33924=CARTESIAN_POINT('Ctrl Pts',(70.9158061804551,201.06521919638,46.2240411771262));
#33925=CARTESIAN_POINT('Ctrl Pts',(72.8071059401065,200.888122624381,45.0912414687117));
#33926=CARTESIAN_POINT('Ctrl Pts',(75.1818659698207,200.711026052382,44.799169947306));
#33927=CARTESIAN_POINT('Ctrl Pts',(77.2912945088766,200.533929480384,45.4399204438787));
#33928=CARTESIAN_POINT('Ctrl Pts',(79.4007230479325,200.356832908385,46.0806709404514));
#33929=CARTESIAN_POINT('Ctrl Pts',(81.2118275942149,200.179736336386,47.644221801402));
#33930=CARTESIAN_POINT('Ctrl Pts',(82.1535440633146,200.002639764387,49.6375657386261));
#33931=CARTESIAN_POINT('Ctrl Pts',(82.6515697929939,199.908982435045,50.6917435101873));
#33932=CARTESIAN_POINT('Ctrl Pts',(82.9129498948701,199.815325105703,51.8569119935475));
#33933=CARTESIAN_POINT('Ctrl Pts',(82.9129498948689,199.721667776361,53.0228109606438));
#33934=CARTESIAN_POINT('Origin',(74.9879498948689,255.,53.0228109606356));
#33935=CARTESIAN_POINT('',(82.9129498948689,194.278332223638,53.0228109606302));
#33936=CARTESIAN_POINT('',(82.9158434391062,195.721667776361,53.0210929467476));
#33937=CARTESIAN_POINT('',(82.9129498948689,255.,53.0228109606356));
#33938=CARTESIAN_POINT('Ctrl Pts',(82.9129498948689,194.278332223638,53.0228109606302));
#33939=CARTESIAN_POINT('Ctrl Pts',(82.9129498948674,194.455428795637,50.8182135007204));
#33940=CARTESIAN_POINT('Ctrl Pts',(81.9432795991077,194.632525367636,48.6308565362848));
#33941=CARTESIAN_POINT('Ctrl Pts',(80.3096882702503,194.809621939634,47.150441280175));
#33942=CARTESIAN_POINT('Ctrl Pts',(78.6760969413929,194.986718511633,45.6700260240651));
#33943=CARTESIAN_POINT('Ctrl Pts',(76.4041347530391,195.163815083632,44.9197069006021));
#33944=CARTESIAN_POINT('Ctrl Pts',(74.2101800112167,195.340911655631,45.1360689838695));
#33945=CARTESIAN_POINT('Ctrl Pts',(72.0162252693943,195.518008227629,45.3524310671369));
#33946=CARTESIAN_POINT('Ctrl Pts',(69.9345925076936,195.695104799628,46.5320903475048));
#33947=CARTESIAN_POINT('Ctrl Pts',(68.6216467656576,195.872201371627,48.3030853894827));
#33948=CARTESIAN_POINT('Ctrl Pts',(67.3087010236216,196.049297943626,50.0740804314607));
#33949=CARTESIAN_POINT('Ctrl Pts',(66.7849774198235,196.226394515624,52.4087119996462));
#33950=CARTESIAN_POINT('Ctrl Pts',(67.2156126057616,196.403491087623,54.57084134288));
#33951=CARTESIAN_POINT('Ctrl Pts',(67.6462477916997,196.580587659622,56.7329706861139));
#33952=CARTESIAN_POINT('Ctrl Pts',(69.0245064208004,196.75768423162,58.6887810357269));
#33953=CARTESIAN_POINT('Ctrl Pts',(70.915806180451,196.934780803619,59.8215807441425));
#33954=CARTESIAN_POINT('Ctrl Pts',(72.8071059401016,197.111877375618,60.954380452558));
#33955=CARTESIAN_POINT('Ctrl Pts',(75.1818659698154,197.288973947617,61.2464519739653));
#33956=CARTESIAN_POINT('Ctrl Pts',(77.2912945088716,197.466070519615,60.605701477394));
#33957=CARTESIAN_POINT('Ctrl Pts',(79.4007230479277,197.643167091614,59.9649509808227));
#33958=CARTESIAN_POINT('Ctrl Pts',(81.2118275942111,197.820263663613,58.4014001198735));
#33959=CARTESIAN_POINT('Ctrl Pts',(82.1535440633121,197.997360235612,56.4080561826502));
#33960=CARTESIAN_POINT('Ctrl Pts',(82.6515697929926,198.091017564954,55.3538784110886));
#33961=CARTESIAN_POINT('Ctrl Pts',(82.9129498948697,198.184674894296,54.1887099277276));
#33962=CARTESIAN_POINT('Ctrl Pts',(82.9129498948689,198.278332223638,53.0228109606304));
#33963=CARTESIAN_POINT('Ctrl Pts',(82.9129498948689,199.721667776361,53.0228109606438));
#33964=CARTESIAN_POINT('Ctrl Pts',(82.9129498948666,199.544571204362,55.2274084205536));
#33965=CARTESIAN_POINT('Ctrl Pts',(81.9432795991061,199.367474632364,57.4147653849889));
#33966=CARTESIAN_POINT('Ctrl Pts',(80.3096882702482,199.190378060365,58.8951806410981));
#33967=CARTESIAN_POINT('Ctrl Pts',(78.6760969413902,199.013281488366,60.3755958972073));
#33968=CARTESIAN_POINT('Ctrl Pts',(76.4041347530362,198.836184916367,61.1259150206695));
#33969=CARTESIAN_POINT('Ctrl Pts',(74.2101800112138,198.659088344369,60.9095529374013));
#33970=CARTESIAN_POINT('Ctrl Pts',(72.0162252693915,198.48199177237,60.6931908541332));
#33971=CARTESIAN_POINT('Ctrl Pts',(69.9345925076912,198.304895200371,59.5135315737646));
#33972=CARTESIAN_POINT('Ctrl Pts',(68.6216467656559,198.127798628372,57.7425365317861));
#33973=CARTESIAN_POINT('Ctrl Pts',(67.3087010236206,197.950702056374,55.9715414898077));
#33974=CARTESIAN_POINT('Ctrl Pts',(66.7849774198233,197.773605484375,53.636909921622));
#33975=CARTESIAN_POINT('Ctrl Pts',(67.2156126057621,197.596508912376,51.4747805783883));
#33976=CARTESIAN_POINT('Ctrl Pts',(67.646247791701,197.419412340378,49.3126512351546));
#33977=CARTESIAN_POINT('Ctrl Pts',(69.0245064208024,197.242315768379,47.3568408855421));
#33978=CARTESIAN_POINT('Ctrl Pts',(70.9158061804534,197.06521919638,46.2240411771272));
#33979=CARTESIAN_POINT('Ctrl Pts',(72.8071059401044,196.888122624381,45.0912414687123));
#33980=CARTESIAN_POINT('Ctrl Pts',(75.1818659698184,196.711026052383,44.7991699473059));
#33981=CARTESIAN_POINT('Ctrl Pts',(77.2912945088743,196.533929480384,45.439920443878));
#33982=CARTESIAN_POINT('Ctrl Pts',(79.4007230479302,196.356832908385,46.08067094045));
#33983=CARTESIAN_POINT('Ctrl Pts',(81.211827594213,196.179736336386,47.6442218013999));
#33984=CARTESIAN_POINT('Ctrl Pts',(82.1535440633133,196.002639764388,49.6375657386235));
#33985=CARTESIAN_POINT('Ctrl Pts',(82.6515697929934,195.908982435045,50.6917435101853));
#33986=CARTESIAN_POINT('Ctrl Pts',(82.9129498948701,195.815325105703,51.8569119935464));
#33987=CARTESIAN_POINT('Ctrl Pts',(82.9129498948689,195.721667776361,53.0228109606436));
#33988=CARTESIAN_POINT('Origin',(74.9879498948689,255.,53.0228109606356));
#33989=CARTESIAN_POINT('',(82.9085809447878,190.278332223638,53.0245374982806));
#33990=CARTESIAN_POINT('',(82.9093019423321,191.721667776361,53.0219586769292));
#33991=CARTESIAN_POINT('',(82.9129498948689,255.,53.0228109606356));
#33992=CARTESIAN_POINT('Ctrl Pts',(82.9129498948689,190.278332223638,53.0228109606296));
#33993=CARTESIAN_POINT('Ctrl Pts',(82.9129498948673,190.455428795637,50.8182135007196));
#33994=CARTESIAN_POINT('Ctrl Pts',(81.9432795991072,190.632525367636,48.630856536284));
#33995=CARTESIAN_POINT('Ctrl Pts',(80.3096882702495,190.809621939634,47.1504412801742));
#33996=CARTESIAN_POINT('Ctrl Pts',(78.6760969413918,190.986718511633,45.6700260240645));
#33997=CARTESIAN_POINT('Ctrl Pts',(76.4041347530377,191.163815083632,44.9197069006019));
#33998=CARTESIAN_POINT('Ctrl Pts',(74.2101800112152,191.340911655631,45.1360689838697));
#33999=CARTESIAN_POINT('Ctrl Pts',(72.0162252693926,191.518008227629,45.3524310671375));
#34000=CARTESIAN_POINT('Ctrl Pts',(69.934592507692,191.695104799628,46.5320903475059));
#34001=CARTESIAN_POINT('Ctrl Pts',(68.6216467656564,191.872201371627,48.3030853894843));
#34002=CARTESIAN_POINT('Ctrl Pts',(67.3087010236208,192.049297943626,50.0740804314627));
#34003=CARTESIAN_POINT('Ctrl Pts',(66.7849774198233,192.226394515624,52.4087119996485));
#34004=CARTESIAN_POINT('Ctrl Pts',(67.2156126057621,192.403491087623,54.5708413428824));
#34005=CARTESIAN_POINT('Ctrl Pts',(67.6462477917009,192.580587659622,56.7329706861163));
#34006=CARTESIAN_POINT('Ctrl Pts',(69.0245064208023,192.757684231621,58.688781035729));
#34007=CARTESIAN_POINT('Ctrl Pts',(70.9158061804534,192.934780803619,59.8215807441439));
#34008=CARTESIAN_POINT('Ctrl Pts',(72.8071059401046,193.111877375618,60.9543804525589));
#34009=CARTESIAN_POINT('Ctrl Pts',(75.1818659698187,193.288973947617,61.2464519739652));
#34010=CARTESIAN_POINT('Ctrl Pts',(77.2912945088747,193.466070519616,60.605701477393));
#34011=CARTESIAN_POINT('Ctrl Pts',(79.4007230479308,193.643167091614,59.9649509808209));
#34012=CARTESIAN_POINT('Ctrl Pts',(81.2118275942136,193.820263663613,58.4014001198706));
#34013=CARTESIAN_POINT('Ctrl Pts',(82.1535440633137,193.997360235612,56.4080561826468));
#34014=CARTESIAN_POINT('Ctrl Pts',(82.6515697929932,194.091017564954,55.353878411086));
#34015=CARTESIAN_POINT('Ctrl Pts',(82.9129498948697,194.184674894296,54.1887099277262));
#34016=CARTESIAN_POINT('Ctrl Pts',(82.9129498948689,194.278332223638,53.0228109606302));
#34017=CARTESIAN_POINT('Ctrl Pts',(82.923873025696,195.721667776361,53.0163254573511));
#34018=CARTESIAN_POINT('Ctrl Pts',(82.9083833277983,195.529643202921,55.3974887847026));
#34019=CARTESIAN_POINT('Ctrl Pts',(81.7627222847989,195.337618629481,57.7957333087917));
#34020=CARTESIAN_POINT('Ctrl Pts',(79.8914368959041,195.145594056041,59.2662252860257));
#34021=CARTESIAN_POINT('Ctrl Pts',(77.8239700413806,194.933438046488,60.8908804245823));
#34022=CARTESIAN_POINT('Ctrl Pts',(74.8707577904796,194.721282036936,61.3830590248267));
#34023=CARTESIAN_POINT('Ctrl Pts',(72.3870455266111,194.509126027384,60.5216002134336));
#34024=CARTESIAN_POINT('Ctrl Pts',(69.9033332627425,194.296970017831,59.6601414020404));
#34025=CARTESIAN_POINT('Ctrl Pts',(67.8891209859066,194.084814008279,57.4450451790096));
#34026=CARTESIAN_POINT('Ctrl Pts',(67.271653649997,193.872657998727,54.8891387638881));
#34027=CARTESIAN_POINT('Ctrl Pts',(66.6541863140874,193.660501989174,52.3332323487668));
#34028=CARTESIAN_POINT('Ctrl Pts',(67.4334639191042,193.448345979622,49.4365157415545));
#34029=CARTESIAN_POINT('Ctrl Pts',(69.248896360684,193.23618997007,47.5373933700901));
#34030=CARTESIAN_POINT('Ctrl Pts',(71.0643288022642,193.024033960517,45.6382709986253));
#34031=CARTESIAN_POINT('Ctrl Pts',(73.9159160804077,192.811877950965,44.7367428629084));
#34032=CARTESIAN_POINT('Ctrl Pts',(76.499647194539,192.599721941413,45.2329851776049));
#34033=CARTESIAN_POINT('Ctrl Pts',(77.7915127516044,192.493643936637,45.4811063349531));
#34034=CARTESIAN_POINT('Ctrl Pts',(79.0164142676668,192.387565931861,46.0786701049046));
#34035=CARTESIAN_POINT('Ctrl Pts',(80.0368081446007,192.281487927084,46.9232989991627));
#34036=CARTESIAN_POINT('Ctrl Pts',(81.0572020215346,192.175409922308,47.7679278934208));
#34037=CARTESIAN_POINT('Ctrl Pts',(81.87308825934,192.069331917532,48.8596219119855));
#34038=CARTESIAN_POINT('Ctrl Pts',(82.3581951748484,191.963253912756,50.0823859966649));
#34039=CARTESIAN_POINT('Ctrl Pts',(82.7264622367569,191.882725200624,51.0106426808646));
#34040=CARTESIAN_POINT('Ctrl Pts',(82.9041002083746,191.802196488493,52.0144354272772));
#34041=CARTESIAN_POINT('Ctrl Pts',(82.89928520713,191.721667776361,53.0196184325889));
#34042=CARTESIAN_POINT('Origin',(74.9879498948689,255.,53.0228109606356));
#34043=CARTESIAN_POINT('',(82.9141190436509,186.278332223638,53.0234646524037));
#34044=CARTESIAN_POINT('',(82.9129498948689,187.721667776361,53.0228109606433));
#34045=CARTESIAN_POINT('',(82.9129498948689,255.,53.0228109606356));
#34046=CARTESIAN_POINT('Ctrl Pts',(82.9213928923929,186.278332223638,53.0275315900476));
#34047=CARTESIAN_POINT('Ctrl Pts',(82.9050897166817,186.467677394884,50.6784741063503));
#34048=CARTESIAN_POINT('Ctrl Pts',(81.7986655277071,186.657022566129,48.3158326354731));
#34049=CARTESIAN_POINT('Ctrl Pts',(79.9715559132873,186.846367737375,46.8431606257875));
#34050=CARTESIAN_POINT('Ctrl Pts',(77.9243302974441,187.058523746927,45.19307250947));
#34051=CARTESIAN_POINT('Ctrl Pts',(74.9723143575872,187.27067975648,44.6603037237834));
#34052=CARTESIAN_POINT('Ctrl Pts',(72.4796900407957,187.482835766032,45.4905354667791));
#34053=CARTESIAN_POINT('Ctrl Pts',(69.9870657240046,187.694991775584,46.3207672097748));
#34054=CARTESIAN_POINT('Ctrl Pts',(67.9538330302788,187.907147785136,48.5139994814526));
#34055=CARTESIAN_POINT('Ctrl Pts',(67.2988469653665,188.119303794689,51.0621196041693));
#34056=CARTESIAN_POINT('Ctrl Pts',(66.9713539329103,188.225381799465,52.3361796655279));
#34057=CARTESIAN_POINT('Ctrl Pts',(66.9884225576576,188.331459804241,53.6989616896462));
#34058=CARTESIAN_POINT('Ctrl Pts',(67.3162393427771,188.437537809017,54.9823703496194));
#34059=CARTESIAN_POINT('Ctrl Pts',(67.6440561278964,188.543615813793,56.2657790095924));
#34060=CARTESIAN_POINT('Ctrl Pts',(68.2826210733879,188.64969381857,57.4698143054203));
#34061=CARTESIAN_POINT('Ctrl Pts',(69.1809930736355,188.755771823346,58.4307557580733));
#34062=CARTESIAN_POINT('Ctrl Pts',(70.9777370741309,188.967927832898,60.3526386633794));
#34063=CARTESIAN_POINT('Ctrl Pts',(73.8137092936511,189.18008384245,61.3021461959855));
#34064=CARTESIAN_POINT('Ctrl Pts',(76.3991529872867,189.392239852003,60.8353039969753));
#34065=CARTESIAN_POINT('Ctrl Pts',(78.9845966809222,189.604395861555,60.3684617979652));
#34066=CARTESIAN_POINT('Ctrl Pts',(81.3195118486733,189.816551871107,58.485269867339));
#34067=CARTESIAN_POINT('Ctrl Pts',(82.3246404126769,190.02870788066,56.0555291232267));
#34068=CARTESIAN_POINT('Ctrl Pts',(82.7188543340392,190.111915994986,55.1025787635085));
#34069=CARTESIAN_POINT('Ctrl Pts',(82.9085167700725,190.195124109312,54.0655567404961));
#34070=CARTESIAN_POINT('Ctrl Pts',(82.9028892198067,190.278332223638,53.0267867749482));
#34071=CARTESIAN_POINT('Ctrl Pts',(82.9129498948689,191.721667776361,53.022810960643));
#34072=CARTESIAN_POINT('Ctrl Pts',(82.9129498948669,191.544571204362,55.2274084205527));
#34073=CARTESIAN_POINT('Ctrl Pts',(81.9432795991067,191.367474632364,57.4147653849879));
#34074=CARTESIAN_POINT('Ctrl Pts',(80.3096882702491,191.190378060365,58.8951806410973));
#34075=CARTESIAN_POINT('Ctrl Pts',(78.6760969413915,191.013281488366,60.3755958972067));
#34076=CARTESIAN_POINT('Ctrl Pts',(76.4041347530378,190.836184916368,61.1259150206692));
#34077=CARTESIAN_POINT('Ctrl Pts',(74.2101800112155,190.659088344369,60.9095529374015));
#34078=CARTESIAN_POINT('Ctrl Pts',(72.0162252693933,190.48199177237,60.6931908541338));
#34079=CARTESIAN_POINT('Ctrl Pts',(69.9345925076929,190.304895200371,59.5135315737658));
#34080=CARTESIAN_POINT('Ctrl Pts',(68.6216467656572,190.127798628373,57.7425365317879));
#34081=CARTESIAN_POINT('Ctrl Pts',(67.3087010236215,189.950702056374,55.9715414898099));
#34082=CARTESIAN_POINT('Ctrl Pts',(66.7849774198235,189.773605484375,53.6369099216246));
#34083=CARTESIAN_POINT('Ctrl Pts',(67.2156126057616,189.596508912376,51.4747805783908));
#34084=CARTESIAN_POINT('Ctrl Pts',(67.6462477916998,189.419412340378,49.3126512351571));
#34085=CARTESIAN_POINT('Ctrl Pts',(69.0245064208004,189.242315768379,47.3568408855443));
#34086=CARTESIAN_POINT('Ctrl Pts',(70.9158061804508,189.06521919638,46.2240411771288));
#34087=CARTESIAN_POINT('Ctrl Pts',(72.8071059401013,188.888122624382,45.0912414687132));
#34088=CARTESIAN_POINT('Ctrl Pts',(75.1818659698149,188.711026052383,44.7991699473059));
#34089=CARTESIAN_POINT('Ctrl Pts',(77.2912945088709,188.533929480384,45.4399204438769));
#34090=CARTESIAN_POINT('Ctrl Pts',(79.400723047927,188.356832908385,46.080670940448));
#34091=CARTESIAN_POINT('Ctrl Pts',(81.2118275942104,188.179736336387,47.6442218013969));
#34092=CARTESIAN_POINT('Ctrl Pts',(82.1535440633116,188.002639764388,49.63756573862));
#34093=CARTESIAN_POINT('Ctrl Pts',(82.6515697929927,187.908982435046,50.6917435101825));
#34094=CARTESIAN_POINT('Ctrl Pts',(82.91294989487,187.815325105703,51.8569119935445));
#34095=CARTESIAN_POINT('Ctrl Pts',(82.9129498948689,187.721667776361,53.0228109606428));
#34096=CARTESIAN_POINT('Origin',(74.9879498948689,255.,53.0228109606356));
#34097=CARTESIAN_POINT('',(82.9129498948689,182.278332223638,53.0228109606297));
#34098=CARTESIAN_POINT('',(82.9148398491843,183.721667776361,53.0234719832117));
#34099=CARTESIAN_POINT('',(82.9129498948689,255.,53.0228109606356));
#34100=CARTESIAN_POINT('Ctrl Pts',(82.9129498948689,182.278332223638,53.0228109606297));
#34101=CARTESIAN_POINT('Ctrl Pts',(82.9129498948673,182.455428795637,50.8182135007202));
#34102=CARTESIAN_POINT('Ctrl Pts',(81.9432795991077,182.632525367636,48.6308565362849));
#34103=CARTESIAN_POINT('Ctrl Pts',(80.3096882702506,182.809621939634,47.1504412801752));
#34104=CARTESIAN_POINT('Ctrl Pts',(78.6760969413935,182.986718511633,45.6700260240655));
#34105=CARTESIAN_POINT('Ctrl Pts',(76.4041347530401,183.163815083632,44.9197069006024));
#34106=CARTESIAN_POINT('Ctrl Pts',(74.210180011218,183.340911655631,45.1360689838694));
#34107=CARTESIAN_POINT('Ctrl Pts',(72.0162252693958,183.518008227629,45.3524310671364));
#34108=CARTESIAN_POINT('Ctrl Pts',(69.9345925076952,183.695104799628,46.5320903475036));
#34109=CARTESIAN_POINT('Ctrl Pts',(68.6216467656589,183.872201371627,48.3030853894809));
#34110=CARTESIAN_POINT('Ctrl Pts',(67.3087010236226,184.049297943625,50.0740804314583));
#34111=CARTESIAN_POINT('Ctrl Pts',(66.7849774198238,184.226394515624,52.4087119996433));
#34112=CARTESIAN_POINT('Ctrl Pts',(67.215612605761,184.403491087623,54.570841342877));
#34113=CARTESIAN_POINT('Ctrl Pts',(67.6462477916982,184.580587659621,56.7329706861107));
#34114=CARTESIAN_POINT('Ctrl Pts',(69.0245064207978,184.75768423162,58.688781035724));
#34115=CARTESIAN_POINT('Ctrl Pts',(70.9158061804475,184.934780803619,59.8215807441404));
#34116=CARTESIAN_POINT('Ctrl Pts',(72.8071059400973,185.111877375618,60.9543804525568));
#34117=CARTESIAN_POINT('Ctrl Pts',(75.1818659698106,185.288973947616,61.2464519739653));
#34118=CARTESIAN_POINT('Ctrl Pts',(77.2912945088669,185.466070519615,60.6057014773954));
#34119=CARTESIAN_POINT('Ctrl Pts',(79.4007230479231,185.643167091614,59.9649509808256));
#34120=CARTESIAN_POINT('Ctrl Pts',(81.2118275942073,185.820263663612,58.4014001198778));
#34121=CARTESIAN_POINT('Ctrl Pts',(82.1535440633096,185.997360235611,56.4080561826554));
#34122=CARTESIAN_POINT('Ctrl Pts',(82.6515697929918,186.091017564953,55.3538784110921));
#34123=CARTESIAN_POINT('Ctrl Pts',(82.9129498948698,186.184674894296,54.1887099277289));
#34124=CARTESIAN_POINT('Ctrl Pts',(82.9129498948689,186.278332223638,53.0228109606294));
#34125=CARTESIAN_POINT('Ctrl Pts',(82.9097357579327,187.721667776361,53.0272021174371));
#34126=CARTESIAN_POINT('Ctrl Pts',(82.9141531006835,187.65043775496,53.9154826081945));
#34127=CARTESIAN_POINT('Ctrl Pts',(82.7730477508649,187.579207733559,54.8021676263194));
#34128=CARTESIAN_POINT('Ctrl Pts',(82.4805842333433,187.507977712157,55.6356724429414));
#34129=CARTESIAN_POINT('Ctrl Pts',(81.6094923594901,187.295821702605,58.1182360075521));
#34130=CARTESIAN_POINT('Ctrl Pts',(79.3956652419737,187.083665693053,60.1290250263497));
#34131=CARTESIAN_POINT('Ctrl Pts',(76.8410254653617,186.8715096835,60.7424387069034));
#34132=CARTESIAN_POINT('Ctrl Pts',(74.2863856887502,186.659353673948,61.3558523874571));
#34133=CARTESIAN_POINT('Ctrl Pts',(71.3909332530432,186.447197664396,60.5718907297675));
#34134=CARTESIAN_POINT('Ctrl Pts',(69.4927557498842,186.235041654843,58.7523177907851));
#34135=CARTESIAN_POINT('Ctrl Pts',(67.5945782467252,186.022885645291,56.9327448518028));
#34136=CARTESIAN_POINT('Ctrl Pts',(66.6936756761142,185.810729635739,54.0775606315278));
#34137=CARTESIAN_POINT('Ctrl Pts',(67.1988209362901,185.598573626187,51.4976834717501));
#34138=CARTESIAN_POINT('Ctrl Pts',(67.703966196466,185.386417616634,48.9178063119723));
#34139=CARTESIAN_POINT('Ctrl Pts',(69.6151592874289,185.174261607082,46.6132362126918));
#34140=CARTESIAN_POINT('Ctrl Pts',(72.0594072029743,184.96210559753,45.6439191122917));
#34141=CARTESIAN_POINT('Ctrl Pts',(74.5036551185198,184.749949587977,44.6746020118916));
#34142=CARTESIAN_POINT('Ctrl Pts',(77.4809578586477,184.537793578425,45.0405379103718));
#34143=CARTESIAN_POINT('Ctrl Pts',(79.6156024351346,184.325637568872,46.5721231230884));
#34144=CARTESIAN_POINT('Ctrl Pts',(81.6412514605336,184.124314304702,48.0255051650586));
#34145=CARTESIAN_POINT('Ctrl Pts',(82.9080981087541,183.922991040532,50.5285387843388));
#34146=CARTESIAN_POINT('Ctrl Pts',(82.9215114273086,183.721667776361,53.0258054066561));
#34147=CARTESIAN_POINT('Origin',(74.9879498948689,255.,53.0228109606356));
#34148=CARTESIAN_POINT('',(82.9129498948689,178.278332223638,53.0228109606295));
#34149=CARTESIAN_POINT('',(82.9129498948689,179.721667776361,53.0228109606429));
#34150=CARTESIAN_POINT('',(82.9129498948689,255.,53.0228109606356));
#34151=CARTESIAN_POINT('Ctrl Pts',(82.9129498948689,178.278332223638,53.0228109606295));
#34152=CARTESIAN_POINT('Ctrl Pts',(82.9129498948672,178.455428795637,50.8182135007197));
#34153=CARTESIAN_POINT('Ctrl Pts',(81.9432795991073,178.632525367636,48.6308565362842));
#34154=CARTESIAN_POINT('Ctrl Pts',(80.3096882702498,178.809621939634,47.1504412801745));
#34155=CARTESIAN_POINT('Ctrl Pts',(78.6760969413923,178.986718511633,45.6700260240648));
#34156=CARTESIAN_POINT('Ctrl Pts',(76.4041347530384,179.163815083632,44.919706900602));
#34157=CARTESIAN_POINT('Ctrl Pts',(74.210180011216,179.340911655631,45.1360689838696));
#34158=CARTESIAN_POINT('Ctrl Pts',(72.0162252693936,179.518008227629,45.3524310671372));
#34159=CARTESIAN_POINT('Ctrl Pts',(69.934592507693,179.695104799628,46.5320903475052));
#34160=CARTESIAN_POINT('Ctrl Pts',(68.6216467656572,179.872201371627,48.3030853894833));
#34161=CARTESIAN_POINT('Ctrl Pts',(67.3087010236214,180.049297943626,50.0740804314613));
#34162=CARTESIAN_POINT('Ctrl Pts',(66.7849774198234,180.226394515624,52.4087119996469));
#34163=CARTESIAN_POINT('Ctrl Pts',(67.2156126057617,180.403491087623,54.5708413428807));
#34164=CARTESIAN_POINT('Ctrl Pts',(67.6462477917,180.580587659622,56.7329706861145));
#34165=CARTESIAN_POINT('Ctrl Pts',(69.0245064208009,180.75768423162,58.6887810357274));
#34166=CARTESIAN_POINT('Ctrl Pts',(70.9158061804516,180.934780803619,59.8215807441428));
#34167=CARTESIAN_POINT('Ctrl Pts',(72.8071059401022,181.111877375618,60.9543804525582));
#34168=CARTESIAN_POINT('Ctrl Pts',(75.1818659698161,181.288973947617,61.2464519739652));
#34169=CARTESIAN_POINT('Ctrl Pts',(77.2912945088722,181.466070519615,60.6057014773938));
#34170=CARTESIAN_POINT('Ctrl Pts',(79.4007230479283,181.643167091614,59.9649509808224));
#34171=CARTESIAN_POINT('Ctrl Pts',(81.2118275942116,181.820263663613,58.4014001198729));
#34172=CARTESIAN_POINT('Ctrl Pts',(82.1535440633124,181.997360235612,56.4080561826496));
#34173=CARTESIAN_POINT('Ctrl Pts',(82.6515697929928,182.091017564954,55.3538784110879));
#34174=CARTESIAN_POINT('Ctrl Pts',(82.9129498948698,182.184674894296,54.1887099277269));
#34175=CARTESIAN_POINT('Ctrl Pts',(82.9129498948689,182.278332223638,53.0228109606297));
#34176=CARTESIAN_POINT('Ctrl Pts',(82.9129498948689,183.721667776361,53.0228109606431));
#34177=CARTESIAN_POINT('Ctrl Pts',(82.9129498948668,183.544571204362,55.2274084205531));
#34178=CARTESIAN_POINT('Ctrl Pts',(81.9432795991064,183.367474632364,57.4147653849885));
#34179=CARTESIAN_POINT('Ctrl Pts',(80.3096882702484,183.190378060365,58.8951806410979));
#34180=CARTESIAN_POINT('Ctrl Pts',(78.6760969413904,183.013281488366,60.3755958972073));
#34181=CARTESIAN_POINT('Ctrl Pts',(76.4041347530361,182.836184916367,61.1259150206696));
#34182=CARTESIAN_POINT('Ctrl Pts',(74.2101800112136,182.659088344369,60.9095529374013));
#34183=CARTESIAN_POINT('Ctrl Pts',(72.0162252693911,182.48199177237,60.6931908541331));
#34184=CARTESIAN_POINT('Ctrl Pts',(69.9345925076908,182.304895200371,59.5135315737643));
#34185=CARTESIAN_POINT('Ctrl Pts',(68.6216467656555,182.127798628372,57.7425365317856));
#34186=CARTESIAN_POINT('Ctrl Pts',(67.3087010236202,181.950702056374,55.9715414898069));
#34187=CARTESIAN_POINT('Ctrl Pts',(66.7849774198232,181.773605484375,53.636909921621));
#34188=CARTESIAN_POINT('Ctrl Pts',(67.2156126057624,181.596508912376,51.4747805783872));
#34189=CARTESIAN_POINT('Ctrl Pts',(67.6462477917016,181.419412340377,49.3126512351534));
#34190=CARTESIAN_POINT('Ctrl Pts',(69.0245064208034,181.242315768379,47.356840885541));
#34191=CARTESIAN_POINT('Ctrl Pts',(70.9158061804548,181.06521919638,46.2240411771264));
#34192=CARTESIAN_POINT('Ctrl Pts',(72.8071059401061,180.888122624381,45.0912414687118));
#34193=CARTESIAN_POINT('Ctrl Pts',(75.1818659698203,180.711026052382,44.7991699473059));
#34194=CARTESIAN_POINT('Ctrl Pts',(77.2912945088762,180.533929480384,45.4399204438786));
#34195=CARTESIAN_POINT('Ctrl Pts',(79.4007230479321,180.356832908385,46.0806709404512));
#34196=CARTESIAN_POINT('Ctrl Pts',(81.2118275942147,180.179736336386,47.6442218014017));
#34197=CARTESIAN_POINT('Ctrl Pts',(82.1535440633144,180.002639764387,49.6375657386258));
#34198=CARTESIAN_POINT('Ctrl Pts',(82.6515697929937,179.908982435045,50.6917435101869));
#34199=CARTESIAN_POINT('Ctrl Pts',(82.9129498948701,179.815325105703,51.8569119935471));
#34200=CARTESIAN_POINT('Ctrl Pts',(82.9129498948689,179.721667776361,53.0228109606434));
#34201=CARTESIAN_POINT('Origin',(74.9879498948689,255.,53.0228109606356));
#34202=CARTESIAN_POINT('',(82.9129498948689,174.278332223638,53.0228109606294));
#34203=CARTESIAN_POINT('',(82.9129498948689,175.721667776361,53.0228109606428));
#34204=CARTESIAN_POINT('',(82.9129498948689,255.,53.0228109606356));
#34205=CARTESIAN_POINT('Ctrl Pts',(82.9129498948689,174.278332223638,53.0228109606289));
#34206=CARTESIAN_POINT('Ctrl Pts',(82.9129498948671,174.455428795637,50.8182135007192));
#34207=CARTESIAN_POINT('Ctrl Pts',(81.9432795991071,174.632525367636,48.630856536284));
#34208=CARTESIAN_POINT('Ctrl Pts',(80.3096882702497,174.809621939634,47.1504412801744));
#34209=CARTESIAN_POINT('Ctrl Pts',(78.6760969413922,174.986718511633,45.6700260240648));
#34210=CARTESIAN_POINT('Ctrl Pts',(76.4041347530385,175.163815083632,44.9197069006021));
#34211=CARTESIAN_POINT('Ctrl Pts',(74.2101800112163,175.340911655631,45.1360689838696));
#34212=CARTESIAN_POINT('Ctrl Pts',(72.016225269394,175.518008227629,45.3524310671371));
#34213=CARTESIAN_POINT('Ctrl Pts',(69.9345925076935,175.695104799628,46.5320903475048));
#34214=CARTESIAN_POINT('Ctrl Pts',(68.6216467656576,175.872201371627,48.3030853894827));
#34215=CARTESIAN_POINT('Ctrl Pts',(67.3087010236217,176.049297943626,50.0740804314605));
#34216=CARTESIAN_POINT('Ctrl Pts',(66.7849774198236,176.226394515624,52.4087119996458));
#34217=CARTESIAN_POINT('Ctrl Pts',(67.2156126057615,176.403491087623,54.5708413428795));
#34218=CARTESIAN_POINT('Ctrl Pts',(67.6462477916994,176.580587659622,56.7329706861133));
#34219=CARTESIAN_POINT('Ctrl Pts',(69.0245064207998,176.75768423162,58.6887810357262));
#34220=CARTESIAN_POINT('Ctrl Pts',(70.9158061804501,176.934780803619,59.821580744142));
#34221=CARTESIAN_POINT('Ctrl Pts',(72.8071059401005,177.111877375618,60.9543804525577));
#34222=CARTESIAN_POINT('Ctrl Pts',(75.1818659698141,177.288973947617,61.2464519739653));
#34223=CARTESIAN_POINT('Ctrl Pts',(77.2912945088702,177.466070519615,60.6057014773944));
#34224=CARTESIAN_POINT('Ctrl Pts',(79.4007230479263,177.643167091614,59.9649509808236));
#34225=CARTESIAN_POINT('Ctrl Pts',(81.2118275942099,177.820263663613,58.4014001198748));
#34226=CARTESIAN_POINT('Ctrl Pts',(82.1535440633113,177.997360235611,56.4080561826519));
#34227=CARTESIAN_POINT('Ctrl Pts',(82.6515697929924,178.091017564954,55.3538784110896));
#34228=CARTESIAN_POINT('Ctrl Pts',(82.9129498948698,178.184674894296,54.1887099277277));
#34229=CARTESIAN_POINT('Ctrl Pts',(82.9129498948689,178.278332223638,53.0228109606295));
#34230=CARTESIAN_POINT('Ctrl Pts',(82.9129498948689,179.721667776361,53.0228109606434));
#34231=CARTESIAN_POINT('Ctrl Pts',(82.9129498948667,179.544571204362,55.2274084205531));
#34232=CARTESIAN_POINT('Ctrl Pts',(81.9432795991065,179.367474632364,57.4147653849882));
#34233=CARTESIAN_POINT('Ctrl Pts',(80.3096882702488,179.190378060365,58.8951806410975));
#34234=CARTESIAN_POINT('Ctrl Pts',(78.6760969413912,179.013281488366,60.3755958972069));
#34235=CARTESIAN_POINT('Ctrl Pts',(76.4041347530373,178.836184916368,61.1259150206693));
#34236=CARTESIAN_POINT('Ctrl Pts',(74.2101800112151,178.659088344369,60.9095529374015));
#34237=CARTESIAN_POINT('Ctrl Pts',(72.0162252693929,178.48199177237,60.6931908541337));
#34238=CARTESIAN_POINT('Ctrl Pts',(69.9345925076926,178.304895200371,59.5135315737656));
#34239=CARTESIAN_POINT('Ctrl Pts',(68.6216467656569,178.127798628373,57.7425365317875));
#34240=CARTESIAN_POINT('Ctrl Pts',(67.3087010236213,177.950702056374,55.9715414898095));
#34241=CARTESIAN_POINT('Ctrl Pts',(66.7849774198235,177.773605484375,53.6369099216241));
#34242=CARTESIAN_POINT('Ctrl Pts',(67.2156126057617,177.596508912376,51.4747805783905));
#34243=CARTESIAN_POINT('Ctrl Pts',(67.6462477917,177.419412340378,49.3126512351568));
#34244=CARTESIAN_POINT('Ctrl Pts',(69.0245064208006,177.242315768379,47.356840885544));
#34245=CARTESIAN_POINT('Ctrl Pts',(70.9158061804511,177.06521919638,46.2240411771286));
#34246=CARTESIAN_POINT('Ctrl Pts',(72.8071059401016,176.888122624382,45.0912414687131));
#34247=CARTESIAN_POINT('Ctrl Pts',(75.1818659698153,176.711026052383,44.7991699473059));
#34248=CARTESIAN_POINT('Ctrl Pts',(77.2912945088713,176.533929480384,45.4399204438771));
#34249=CARTESIAN_POINT('Ctrl Pts',(79.4007230479273,176.356832908385,46.0806709404482));
#34250=CARTESIAN_POINT('Ctrl Pts',(81.2118275942107,176.179736336387,47.6442218013973));
#34251=CARTESIAN_POINT('Ctrl Pts',(82.1535440633118,176.002639764388,49.6375657386203));
#34252=CARTESIAN_POINT('Ctrl Pts',(82.6515697929928,175.908982435046,50.6917435101827));
#34253=CARTESIAN_POINT('Ctrl Pts',(82.91294989487,175.815325105703,51.8569119935446));
#34254=CARTESIAN_POINT('Ctrl Pts',(82.9129498948689,175.721667776361,53.0228109606428));
#34255=CARTESIAN_POINT('Origin',(74.9879498948689,255.,53.0228109606356));
#34256=CARTESIAN_POINT('',(82.9158840595049,170.278332223638,53.0221079210748));
#34257=CARTESIAN_POINT('',(82.9129498948689,171.721667776361,53.0228109606426));
#34258=CARTESIAN_POINT('',(82.9129498948689,255.,53.0228109606356));
#34259=CARTESIAN_POINT('Ctrl Pts',(82.9129498948689,170.278332223638,53.0228109606287));
#34260=CARTESIAN_POINT('Ctrl Pts',(82.912949894867,170.455428795637,50.8182135007189));
#34261=CARTESIAN_POINT('Ctrl Pts',(81.9432795991069,170.632525367636,48.6308565362835));
#34262=CARTESIAN_POINT('Ctrl Pts',(80.3096882702492,170.809621939635,47.150441280174));
#34263=CARTESIAN_POINT('Ctrl Pts',(78.6760969413915,170.986718511633,45.6700260240644));
#34264=CARTESIAN_POINT('Ctrl Pts',(76.4041347530376,171.163815083632,44.9197069006019));
#34265=CARTESIAN_POINT('Ctrl Pts',(74.2101800112152,171.340911655631,45.1360689838697));
#34266=CARTESIAN_POINT('Ctrl Pts',(72.0162252693928,171.518008227629,45.3524310671375));
#34267=CARTESIAN_POINT('Ctrl Pts',(69.9345925076924,171.695104799628,46.5320903475057));
#34268=CARTESIAN_POINT('Ctrl Pts',(68.6216467656567,171.872201371627,48.3030853894839));
#34269=CARTESIAN_POINT('Ctrl Pts',(67.3087010236211,172.049297943626,50.0740804314621));
#34270=CARTESIAN_POINT('Ctrl Pts',(66.7849774198234,172.226394515624,52.4087119996477));
#34271=CARTESIAN_POINT('Ctrl Pts',(67.2156126057619,172.403491087623,54.5708413428815));
#34272=CARTESIAN_POINT('Ctrl Pts',(67.6462477917004,172.580587659622,56.7329706861153));
#34273=CARTESIAN_POINT('Ctrl Pts',(69.0245064208014,172.757684231621,58.688781035728));
#34274=CARTESIAN_POINT('Ctrl Pts',(70.9158061804522,172.934780803619,59.8215807441432));
#34275=CARTESIAN_POINT('Ctrl Pts',(72.807105940103,173.111877375618,60.9543804525585));
#34276=CARTESIAN_POINT('Ctrl Pts',(75.1818659698169,173.288973947617,61.2464519739652));
#34277=CARTESIAN_POINT('Ctrl Pts',(77.291294508873,173.466070519615,60.6057014773936));
#34278=CARTESIAN_POINT('Ctrl Pts',(79.400723047929,173.643167091614,59.9649509808219));
#34279=CARTESIAN_POINT('Ctrl Pts',(81.2118275942121,173.820263663613,58.4014001198723));
#34280=CARTESIAN_POINT('Ctrl Pts',(82.1535440633127,173.997360235612,56.4080561826489));
#34281=CARTESIAN_POINT('Ctrl Pts',(82.651569792993,174.091017564954,55.3538784110872));
#34282=CARTESIAN_POINT('Ctrl Pts',(82.9129498948699,174.184674894296,54.1887099277261));
#34283=CARTESIAN_POINT('Ctrl Pts',(82.9129498948689,174.278332223638,53.0228109606289));
#34284=CARTESIAN_POINT('Ctrl Pts',(82.9129498948689,175.721667776361,53.0228109606428));
#34285=CARTESIAN_POINT('Ctrl Pts',(82.9129498948669,175.544571204362,55.2274084205527));
#34286=CARTESIAN_POINT('Ctrl Pts',(81.9432795991065,175.367474632364,57.4147653849882));
#34287=CARTESIAN_POINT('Ctrl Pts',(80.3096882702486,175.190378060365,58.8951806410977));
#34288=CARTESIAN_POINT('Ctrl Pts',(78.6760969413907,175.013281488366,60.3755958972072));
#34289=CARTESIAN_POINT('Ctrl Pts',(76.4041347530364,174.836184916367,61.1259150206695));
#34290=CARTESIAN_POINT('Ctrl Pts',(74.210180011214,174.659088344369,60.9095529374013));
#34291=CARTESIAN_POINT('Ctrl Pts',(72.0162252693915,174.48199177237,60.6931908541332));
#34292=CARTESIAN_POINT('Ctrl Pts',(69.9345925076911,174.304895200371,59.5135315737645));
#34293=CARTESIAN_POINT('Ctrl Pts',(68.6216467656557,174.127798628372,57.7425365317859));
#34294=CARTESIAN_POINT('Ctrl Pts',(67.3087010236203,173.950702056374,55.9715414898073));
#34295=CARTESIAN_POINT('Ctrl Pts',(66.7849774198232,173.773605484375,53.6369099216214));
#34296=CARTESIAN_POINT('Ctrl Pts',(67.2156126057623,173.596508912376,51.4747805783875));
#34297=CARTESIAN_POINT('Ctrl Pts',(67.6462477917014,173.419412340377,49.3126512351537));
#34298=CARTESIAN_POINT('Ctrl Pts',(69.0245064208031,173.242315768379,47.3568408855413));
#34299=CARTESIAN_POINT('Ctrl Pts',(70.9158061804545,173.06521919638,46.2240411771266));
#34300=CARTESIAN_POINT('Ctrl Pts',(72.8071059401058,172.888122624381,45.0912414687119));
#34301=CARTESIAN_POINT('Ctrl Pts',(75.18186596982,172.711026052382,44.7991699473059));
#34302=CARTESIAN_POINT('Ctrl Pts',(77.2912945088759,172.533929480384,45.4399204438785));
#34303=CARTESIAN_POINT('Ctrl Pts',(79.4007230479318,172.356832908385,46.080670940451));
#34304=CARTESIAN_POINT('Ctrl Pts',(81.2118275942144,172.179736336386,47.6442218014014));
#34305=CARTESIAN_POINT('Ctrl Pts',(82.1535440633142,172.002639764388,49.6375657386255));
#34306=CARTESIAN_POINT('Ctrl Pts',(82.6515697929936,171.908982435045,50.6917435101864));
#34307=CARTESIAN_POINT('Ctrl Pts',(82.9129498948699,171.815325105703,51.8569119935464));
#34308=CARTESIAN_POINT('Ctrl Pts',(82.9129498948689,171.721667776361,53.0228109606426));
#34309=CARTESIAN_POINT('Origin',(74.9879498948689,255.,53.0228109606356));
#34310=CARTESIAN_POINT('',(82.9129498948689,166.278332223638,53.0228109606286));
#34311=CARTESIAN_POINT('',(82.9144547577616,167.721667776361,53.022184232359));
#34312=CARTESIAN_POINT('',(82.9129498948689,255.,53.0228109606356));
#34313=CARTESIAN_POINT('Ctrl Pts',(82.9106451661498,166.278332223638,53.018111936927));
#34314=CARTESIAN_POINT('Ctrl Pts',(82.9151724908915,166.345351755876,52.1826111629703));
#34315=CARTESIAN_POINT('Ctrl Pts',(82.7905111495548,166.412371288115,51.3486593970808));
#34316=CARTESIAN_POINT('Ctrl Pts',(82.5309490101129,166.479390820353,50.5591188525927));
#34317=CARTESIAN_POINT('Ctrl Pts',(81.7092830584731,166.691546829905,48.0597613413635));
#34318=CARTESIAN_POINT('Ctrl Pts',(79.5357860780612,166.903702839457,46.0054454307733));
#34319=CARTESIAN_POINT('Ctrl Pts',(76.9938193710111,167.11585884901,45.341468027555));
#34320=CARTESIAN_POINT('Ctrl Pts',(74.4518526639606,167.328014858562,44.6774906243366));
#34321=CARTESIAN_POINT('Ctrl Pts',(71.5414162302718,167.540170868114,45.4038517284906));
#34322=CARTESIAN_POINT('Ctrl Pts',(69.6075117357223,167.752326877667,47.1854063641216));
#34323=CARTESIAN_POINT('Ctrl Pts',(67.6736072411727,167.964482887219,48.9669609997525));
#34324=CARTESIAN_POINT('Ctrl Pts',(66.7162346857625,168.176638896771,51.8037091668605));
#34325=CARTESIAN_POINT('Ctrl Pts',(67.1700953375757,168.388794906323,54.3931006788104));
#34326=CARTESIAN_POINT('Ctrl Pts',(67.6239559893889,168.600950915876,56.9824921907597));
#34327=CARTESIAN_POINT('Ctrl Pts',(69.4890498484247,168.813106925428,59.3245270475509));
#34328=CARTESIAN_POINT('Ctrl Pts',(71.9135852423216,169.02526293498,60.3421476239523));
#34329=CARTESIAN_POINT('Ctrl Pts',(74.338120636219,169.237418944533,61.3597682003539));
#34330=CARTESIAN_POINT('Ctrl Pts',(77.3220975649777,169.449574954085,61.052974496365));
#34331=CARTESIAN_POINT('Ctrl Pts',(79.4867088649507,169.661730963637,59.5640424456095));
#34332=CARTESIAN_POINT('Ctrl Pts',(81.58375379868,169.867264716971,58.1215860499773));
#34333=CARTESIAN_POINT('Ctrl Pts',(82.9117862805714,170.072798470305,55.569638266714));
#34334=CARTESIAN_POINT('Ctrl Pts',(82.9223099933314,170.278332223639,53.0205682373108));
#34335=CARTESIAN_POINT('Ctrl Pts',(82.9129498948689,171.721667776361,53.0228109606426));
#34336=CARTESIAN_POINT('Ctrl Pts',(82.912949894867,171.544571204362,55.2274084205524));
#34337=CARTESIAN_POINT('Ctrl Pts',(81.9432795991068,171.367474632364,57.4147653849878));
#34338=CARTESIAN_POINT('Ctrl Pts',(80.3096882702491,171.190378060365,58.8951806410973));
#34339=CARTESIAN_POINT('Ctrl Pts',(78.6760969413914,171.013281488366,60.3755958972068));
#34340=CARTESIAN_POINT('Ctrl Pts',(76.4041347530374,170.836184916367,61.1259150206693));
#34341=CARTESIAN_POINT('Ctrl Pts',(74.210180011215,170.659088344369,60.9095529374015));
#34342=CARTESIAN_POINT('Ctrl Pts',(72.0162252693926,170.48199177237,60.6931908541336));
#34343=CARTESIAN_POINT('Ctrl Pts',(69.9345925076922,170.304895200371,59.5135315737653));
#34344=CARTESIAN_POINT('Ctrl Pts',(68.6216467656566,170.127798628373,57.7425365317871));
#34345=CARTESIAN_POINT('Ctrl Pts',(67.308701023621,169.950702056374,55.9715414898089));
#34346=CARTESIAN_POINT('Ctrl Pts',(66.7849774198234,169.773605484375,53.6369099216232));
#34347=CARTESIAN_POINT('Ctrl Pts',(67.2156126057619,169.596508912376,51.4747805783895));
#34348=CARTESIAN_POINT('Ctrl Pts',(67.6462477917005,169.419412340378,49.3126512351557));
#34349=CARTESIAN_POINT('Ctrl Pts',(69.0245064208016,169.242315768379,47.356840885543));
#34350=CARTESIAN_POINT('Ctrl Pts',(70.9158061804524,169.06521919638,46.2240411771278));
#34351=CARTESIAN_POINT('Ctrl Pts',(72.8071059401032,168.888122624381,45.0912414687126));
#34352=CARTESIAN_POINT('Ctrl Pts',(75.1818659698171,168.711026052383,44.7991699473059));
#34353=CARTESIAN_POINT('Ctrl Pts',(77.2912945088732,168.533929480384,45.4399204438776));
#34354=CARTESIAN_POINT('Ctrl Pts',(79.4007230479292,168.356832908385,46.0806709404493));
#34355=CARTESIAN_POINT('Ctrl Pts',(81.2118275942122,168.179736336386,47.644221801399));
#34356=CARTESIAN_POINT('Ctrl Pts',(82.1535440633128,168.002639764388,49.6375657386224));
#34357=CARTESIAN_POINT('Ctrl Pts',(82.6515697929931,167.908982435046,50.6917435101842));
#34358=CARTESIAN_POINT('Ctrl Pts',(82.9129498948699,167.815325105703,51.8569119935452));
#34359=CARTESIAN_POINT('Ctrl Pts',(82.9129498948689,167.721667776361,53.0228109606424));
#34360=CARTESIAN_POINT('Origin',(74.9879498948689,255.,53.0228109606356));
#34361=CARTESIAN_POINT('',(82.9094046261903,162.278332223638,53.0234187658783));
#34362=CARTESIAN_POINT('',(82.9093059554942,163.721667776361,53.0209644405026));
#34363=CARTESIAN_POINT('',(82.9129498948689,255.,53.0228109606356));
#34364=CARTESIAN_POINT('Ctrl Pts',(82.9129498948689,162.278332223638,53.0228109606289));
#34365=CARTESIAN_POINT('Ctrl Pts',(82.912949894867,162.455428795637,50.8182135007193));
#34366=CARTESIAN_POINT('Ctrl Pts',(81.9432795991072,162.632525367636,48.6308565362842));
#34367=CARTESIAN_POINT('Ctrl Pts',(80.3096882702499,162.809621939634,47.1504412801746));
#34368=CARTESIAN_POINT('Ctrl Pts',(78.6760969413927,162.986718511633,45.6700260240651));
#34369=CARTESIAN_POINT('Ctrl Pts',(76.4041347530392,163.163815083632,44.9197069006022));
#34370=CARTESIAN_POINT('Ctrl Pts',(74.2101800112171,163.340911655631,45.1360689838695));
#34371=CARTESIAN_POINT('Ctrl Pts',(72.016225269395,163.518008227629,45.3524310671367));
#34372=CARTESIAN_POINT('Ctrl Pts',(69.9345925076945,163.695104799628,46.5320903475041));
#34373=CARTESIAN_POINT('Ctrl Pts',(68.6216467656584,163.872201371627,48.3030853894816));
#34374=CARTESIAN_POINT('Ctrl Pts',(67.3087010236223,164.049297943625,50.0740804314591));
#34375=CARTESIAN_POINT('Ctrl Pts',(66.7849774198237,164.226394515624,52.4087119996442));
#34376=CARTESIAN_POINT('Ctrl Pts',(67.2156126057612,164.403491087623,54.5708413428778));
#34377=CARTESIAN_POINT('Ctrl Pts',(67.6462477916986,164.580587659622,56.7329706861115));
#34378=CARTESIAN_POINT('Ctrl Pts',(69.0245064207984,164.75768423162,58.6887810357247));
#34379=CARTESIAN_POINT('Ctrl Pts',(70.9158061804483,164.934780803619,59.8215807441408));
#34380=CARTESIAN_POINT('Ctrl Pts',(72.8071059400982,165.111877375618,60.954380452557));
#34381=CARTESIAN_POINT('Ctrl Pts',(75.1818659698115,165.288973947616,61.2464519739653));
#34382=CARTESIAN_POINT('Ctrl Pts',(77.2912945088677,165.466070519615,60.6057014773952));
#34383=CARTESIAN_POINT('Ctrl Pts',(79.4007230479239,165.643167091614,59.9649509808251));
#34384=CARTESIAN_POINT('Ctrl Pts',(81.2118275942079,165.820263663612,58.4014001198771));
#34385=CARTESIAN_POINT('Ctrl Pts',(82.15354406331,165.997360235611,56.4080561826547));
#34386=CARTESIAN_POINT('Ctrl Pts',(82.6515697929921,166.091017564954,55.3538784110913));
#34387=CARTESIAN_POINT('Ctrl Pts',(82.9129498948699,166.184674894296,54.1887099277281));
#34388=CARTESIAN_POINT('Ctrl Pts',(82.9129498948689,166.278332223638,53.0228109606286));
#34389=CARTESIAN_POINT('Ctrl Pts',(82.9224999886125,167.721667776361,53.0188336454937));
#34390=CARTESIAN_POINT('Ctrl Pts',(82.9079541551392,167.528112115953,55.4192369642975));
#34391=CARTESIAN_POINT('Ctrl Pts',(81.7452090935466,167.334556455544,57.8320530567318));
#34392=CARTESIAN_POINT('Ctrl Pts',(79.8479697065302,167.141000795135,59.3001204669499));
#34393=CARTESIAN_POINT('Ctrl Pts',(77.7684090433854,166.928844785583,60.9092665019874));
#34394=CARTESIAN_POINT('Ctrl Pts',(74.8064039462386,166.71668877603,61.3833619487564));
#34395=CARTESIAN_POINT('Ctrl Pts',(72.3307421974144,166.504532766478,60.5038395572588));
#34396=CARTESIAN_POINT('Ctrl Pts',(69.85508044859,166.292376756926,59.6243171657612));
#34397=CARTESIAN_POINT('Ctrl Pts',(67.8657620480882,166.080220747374,57.3911769359969));
#34398=CARTESIAN_POINT('Ctrl Pts',(67.2614600207839,165.868064737821,54.8305633445269));
#34399=CARTESIAN_POINT('Ctrl Pts',(66.9593090071318,165.761986733045,53.5502565487921));
#34400=CARTESIAN_POINT('Ctrl Pts',(67.0034120867789,165.655908728269,52.1880814126309));
#34401=CARTESIAN_POINT('Ctrl Pts',(67.3566273802562,165.549830723493,50.911429310626));
#34402=CARTESIAN_POINT('Ctrl Pts',(67.7098426737335,165.443752718716,49.6347772086211));
#34403=CARTESIAN_POINT('Ctrl Pts',(68.3721701810411,165.33767471394,48.4436481407725));
#34404=CARTESIAN_POINT('Ctrl Pts',(69.2894305829301,165.231596709164,47.500719680399));
#34405=CARTESIAN_POINT('Ctrl Pts',(71.1239513867081,165.019440699612,45.614862759652));
#34406=CARTESIAN_POINT('Ctrl Pts',(73.978203768812,164.80728469006,44.7218082688056));
#34407=CARTESIAN_POINT('Ctrl Pts',(76.553876331361,164.595128680507,45.2398541956007));
#34408=CARTESIAN_POINT('Ctrl Pts',(79.12954889391,164.382972670955,45.7579001223958));
#34409=CARTESIAN_POINT('Ctrl Pts',(81.4266416369042,164.170816661403,47.6870464668322));
#34410=CARTESIAN_POINT('Ctrl Pts',(82.3833659087906,163.95866065185,50.1362508644599));
#34411=CARTESIAN_POINT('Ctrl Pts',(82.7396082116808,163.879663026687,51.0482275337036));
#34412=CARTESIAN_POINT('Ctrl Pts',(82.9100094867986,163.800665401524,52.0323098404564));
#34413=CARTESIAN_POINT('Ctrl Pts',(82.9038913724499,163.721667776361,53.0182206691028));
#34414=CARTESIAN_POINT('Origin',(74.9879498948689,255.,53.0228109606356));
#34415=CARTESIAN_POINT('',(82.9156111860663,158.278332223638,53.0248046760933));
#34416=CARTESIAN_POINT('',(82.9097002693887,159.721667776361,53.0250701739541));
#34417=CARTESIAN_POINT('',(82.9129498948689,255.,53.0228109606356));
#34418=CARTESIAN_POINT('Ctrl Pts',(82.9226459731562,158.278332223638,53.0300748111075));
#34419=CARTESIAN_POINT('Ctrl Pts',(82.905435742135,158.466146307915,50.7000344004891));
#34420=CARTESIAN_POINT('Ctrl Pts',(81.8157007576566,158.653960392192,48.3521897248115));
#34421=CARTESIAN_POINT('Ctrl Pts',(80.0143420609404,158.841774476469,46.8779115309736));
#34422=CARTESIAN_POINT('Ctrl Pts',(77.9795155763405,159.053930486022,45.2125573069881));
#34423=CARTESIAN_POINT('Ctrl Pts',(75.0366495246558,159.266086495574,44.6618833787099));
#34424=CARTESIAN_POINT('Ctrl Pts',(72.5363346617808,159.478242505126,45.473895373638));
#34425=CARTESIAN_POINT('Ctrl Pts',(70.0360197989058,159.690398514678,46.285907368566));
#34426=CARTESIAN_POINT('Ctrl Pts',(67.97825612484,159.902554524231,48.4606052867));
#34427=CARTESIAN_POINT('Ctrl Pts',(67.3102007338575,160.114710533783,51.0037579577669));
#34428=CARTESIAN_POINT('Ctrl Pts',(66.642145342875,160.326866543336,53.5469106288341));
#34429=CARTESIAN_POINT('Ctrl Pts',(67.3637982349759,160.539022552888,56.4585180528339));
#34430=CARTESIAN_POINT('Ctrl Pts',(69.1411944418614,160.75117856244,58.3932850815706));
#34431=CARTESIAN_POINT('Ctrl Pts',(70.9185906487468,160.963334571992,60.328052110307));
#34432=CARTESIAN_POINT('Ctrl Pts',(73.7517301704166,161.175490581545,61.2859787437801));
#34433=CARTESIAN_POINT('Ctrl Pts',(76.3447982422542,161.387646591097,60.8410957481066));
#34434=CARTESIAN_POINT('Ctrl Pts',(77.6413322781732,161.493724595873,60.6186542502698));
#34435=CARTESIAN_POINT('Ctrl Pts',(78.8778484516341,161.599802600649,60.0455103451463));
#34436=CARTESIAN_POINT('Ctrl Pts',(79.9147990521175,161.705880605426,59.2212924824077));
#34437=CARTESIAN_POINT('Ctrl Pts',(80.9517496526007,161.811958610202,58.3970746196692));
#34438=CARTESIAN_POINT('Ctrl Pts',(81.7891346801065,161.918036614978,57.3217827993156));
#34439=CARTESIAN_POINT('Ctrl Pts',(82.2984059455822,162.024114619754,56.1088839970999));
#34440=CARTESIAN_POINT('Ctrl Pts',(82.7052314733612,162.108853821049,55.1399736563743));
#34441=CARTESIAN_POINT('Ctrl Pts',(82.9026734824335,162.193593022343,54.0832503757628));
#34442=CARTESIAN_POINT('Ctrl Pts',(82.8985428315738,162.278332223638,53.0252809253887));
#34443=CARTESIAN_POINT('Ctrl Pts',(82.9129498948689,163.721667776361,53.0228109606422));
#34444=CARTESIAN_POINT('Ctrl Pts',(82.9129498948671,163.544571204362,55.2274084205519));
#34445=CARTESIAN_POINT('Ctrl Pts',(81.9432795991071,163.367474632364,57.4147653849872));
#34446=CARTESIAN_POINT('Ctrl Pts',(80.3096882702497,163.190378060365,58.8951806410968));
#34447=CARTESIAN_POINT('Ctrl Pts',(78.6760969413922,163.013281488366,60.3755958972063));
#34448=CARTESIAN_POINT('Ctrl Pts',(76.4041347530385,162.836184916368,61.1259150206691));
#34449=CARTESIAN_POINT('Ctrl Pts',(74.2101800112163,162.659088344369,60.9095529374016));
#34450=CARTESIAN_POINT('Ctrl Pts',(72.016225269394,162.48199177237,60.6931908541341));
#34451=CARTESIAN_POINT('Ctrl Pts',(69.9345925076935,162.304895200371,59.5135315737663));
#34452=CARTESIAN_POINT('Ctrl Pts',(68.6216467656576,162.127798628373,57.7425365317885));
#34453=CARTESIAN_POINT('Ctrl Pts',(67.3087010236217,161.950702056374,55.9715414898106));
#34454=CARTESIAN_POINT('Ctrl Pts',(66.7849774198236,161.773605484375,53.6369099216253));
#34455=CARTESIAN_POINT('Ctrl Pts',(67.2156126057615,161.596508912377,51.4747805783916));
#34456=CARTESIAN_POINT('Ctrl Pts',(67.6462477916994,161.419412340378,49.3126512351578));
#34457=CARTESIAN_POINT('Ctrl Pts',(69.0245064207998,161.242315768379,47.3568408855449));
#34458=CARTESIAN_POINT('Ctrl Pts',(70.9158061804502,161.06521919638,46.2240411771292));
#34459=CARTESIAN_POINT('Ctrl Pts',(72.8071059401005,160.888122624382,45.0912414687134));
#34460=CARTESIAN_POINT('Ctrl Pts',(75.1818659698141,160.711026052383,44.7991699473059));
#34461=CARTESIAN_POINT('Ctrl Pts',(77.2912945088702,160.533929480384,45.4399204438767));
#34462=CARTESIAN_POINT('Ctrl Pts',(79.4007230479263,160.356832908385,46.0806709404476));
#34463=CARTESIAN_POINT('Ctrl Pts',(81.2118275942099,160.179736336387,47.6442218013964));
#34464=CARTESIAN_POINT('Ctrl Pts',(82.1535440633113,160.002639764388,49.6375657386193));
#34465=CARTESIAN_POINT('Ctrl Pts',(82.6515697929925,159.908982435046,50.6917435101817));
#34466=CARTESIAN_POINT('Ctrl Pts',(82.9129498948699,159.815325105703,51.8569119935438));
#34467=CARTESIAN_POINT('Ctrl Pts',(82.9129498948689,159.721667776361,53.0228109606421));
#34468=CARTESIAN_POINT('Origin',(74.9879498948689,255.,53.0228109606356));
#34469=CARTESIAN_POINT('',(82.9129498948689,154.278332223638,53.0228109606285));
#34470=CARTESIAN_POINT('',(82.9174930945309,155.721667776361,53.0233296472211));
#34471=CARTESIAN_POINT('',(82.9129498948689,255.,53.0228109606356));
#34472=CARTESIAN_POINT('Ctrl Pts',(82.9129498948689,154.278332223638,53.0228109606281));
#34473=CARTESIAN_POINT('Ctrl Pts',(82.9129498948668,154.455428795637,50.8182135007182));
#34474=CARTESIAN_POINT('Ctrl Pts',(81.9432795991065,154.632525367636,48.6308565362829));
#34475=CARTESIAN_POINT('Ctrl Pts',(80.3096882702487,154.809621939635,47.1504412801735));
#34476=CARTESIAN_POINT('Ctrl Pts',(78.6760969413909,154.986718511633,45.6700260240641));
#34477=CARTESIAN_POINT('Ctrl Pts',(76.4041347530369,155.163815083632,44.9197069006018));
#34478=CARTESIAN_POINT('Ctrl Pts',(74.2101800112145,155.340911655631,45.1360689838697));
#34479=CARTESIAN_POINT('Ctrl Pts',(72.0162252693922,155.518008227629,45.3524310671377));
#34480=CARTESIAN_POINT('Ctrl Pts',(69.9345925076918,155.695104799628,46.5320903475061));
#34481=CARTESIAN_POINT('Ctrl Pts',(68.6216467656563,155.872201371627,48.3030853894844));
#34482=CARTESIAN_POINT('Ctrl Pts',(67.3087010236208,156.049297943626,50.0740804314627));
#34483=CARTESIAN_POINT('Ctrl Pts',(66.7849774198233,156.226394515624,52.4087119996484));
#34484=CARTESIAN_POINT('Ctrl Pts',(67.215612605762,156.403491087623,54.5708413428822));
#34485=CARTESIAN_POINT('Ctrl Pts',(67.6462477917007,156.580587659622,56.7329706861159));
#34486=CARTESIAN_POINT('Ctrl Pts',(69.0245064208019,156.757684231621,58.6887810357285));
#34487=CARTESIAN_POINT('Ctrl Pts',(70.9158061804528,156.934780803619,59.8215807441436));
#34488=CARTESIAN_POINT('Ctrl Pts',(72.8071059401037,157.111877375618,60.9543804525586));
#34489=CARTESIAN_POINT('Ctrl Pts',(75.1818659698177,157.288973947617,61.2464519739652));
#34490=CARTESIAN_POINT('Ctrl Pts',(77.2912945088736,157.466070519616,60.6057014773934));
#34491=CARTESIAN_POINT('Ctrl Pts',(79.4007230479296,157.643167091614,59.9649509808215));
#34492=CARTESIAN_POINT('Ctrl Pts',(81.2118275942126,157.820263663613,58.4014001198718));
#34493=CARTESIAN_POINT('Ctrl Pts',(82.153544063313,157.997360235612,56.4080561826482));
#34494=CARTESIAN_POINT('Ctrl Pts',(82.6515697929932,158.091017564954,55.3538784110865));
#34495=CARTESIAN_POINT('Ctrl Pts',(82.91294989487,158.184674894296,54.1887099277255));
#34496=CARTESIAN_POINT('Ctrl Pts',(82.9129498948689,158.278332223638,53.0228109606282));
#34497=CARTESIAN_POINT('Ctrl Pts',(82.9048209325127,159.721667776361,53.0284623995511));
#34498=CARTESIAN_POINT('Ctrl Pts',(82.9112653993961,159.648906667991,53.9369704888767));
#34499=CARTESIAN_POINT('Ctrl Pts',(82.7673370425225,159.576145559622,54.8435061998724));
#34500=CARTESIAN_POINT('Ctrl Pts',(82.4642673810189,159.503384451252,55.6928454274716));
#34501=CARTESIAN_POINT('Ctrl Pts',(81.5805803201484,159.291228441699,58.1693390560172));
#34502=CARTESIAN_POINT('Ctrl Pts',(79.3439020395175,159.079072432147,60.1595583008234));
#34503=CARTESIAN_POINT('Ctrl Pts',(76.783162515954,158.866916422595,60.7541598362084));
#34504=CARTESIAN_POINT('Ctrl Pts',(74.222422992391,158.654760413043,61.3487613715933));
#34505=CARTESIAN_POINT('Ctrl Pts',(71.3376222258955,158.44260440349,60.5477451975575));
#34506=CARTESIAN_POINT('Ctrl Pts',(69.4531073498438,158.230448393938,58.7140257000022));
#34507=CARTESIAN_POINT('Ctrl Pts',(67.5685924737917,158.018292384386,56.8803062024467));
#34508=CARTESIAN_POINT('Ctrl Pts',(66.6843634881836,157.806136374833,54.0138833813717));
#34509=CARTESIAN_POINT('Ctrl Pts',(67.2085217329933,157.593980365281,51.4394477410545));
#34510=CARTESIAN_POINT('Ctrl Pts',(67.7326799778029,157.381824355729,48.8650121007375));
#34511=CARTESIAN_POINT('Ctrl Pts',(69.6652254530304,157.169668346176,46.5825636411782));
#34512=CARTESIAN_POINT('Ctrl Pts',(72.1159778560763,156.957512336624,45.6256229094774));
#34513=CARTESIAN_POINT('Ctrl Pts',(73.3413540575996,156.851434331848,45.1471525436269));
#34514=CARTESIAN_POINT('Ctrl Pts',(74.6962819910771,156.745356327072,45.0000591097411));
#34515=CARTESIAN_POINT('Ctrl Pts',(76.0098184047083,156.639278322295,45.1710085852169));
#34516=CARTESIAN_POINT('Ctrl Pts',(77.3233548183392,156.533200317519,45.3419580606926));
#34517=CARTESIAN_POINT('Ctrl Pts',(78.5954997121234,156.427122312743,45.8309504455298));
#34518=CARTESIAN_POINT('Ctrl Pts',(79.6575912243027,156.321044307967,46.6071220412562));
#34519=CARTESIAN_POINT('Ctrl Pts',(81.6579830685288,156.121252130765,48.0689992072128));
#34520=CARTESIAN_POINT('Ctrl Pts',(82.9132382168655,155.921459953563,50.5496067868154));
#34521=CARTESIAN_POINT('Ctrl Pts',(82.9256064713947,155.721667776361,53.0242559326596));
#34522=CARTESIAN_POINT('Origin',(74.9879498948689,255.,53.0228109606356));
#34523=CARTESIAN_POINT('',(82.908722947904,150.278332223638,53.0221202519349));
#34524=CARTESIAN_POINT('',(82.9129498948689,151.721667776361,53.0228109606417));
#34525=CARTESIAN_POINT('',(82.9129498948689,255.,53.0228109606356));
#34526=CARTESIAN_POINT('Ctrl Pts',(82.9129498948689,150.278332223638,53.0228109606279));
#34527=CARTESIAN_POINT('Ctrl Pts',(82.9129498948668,150.455428795637,50.8182135007181));
#34528=CARTESIAN_POINT('Ctrl Pts',(81.9432795991064,150.632525367636,48.6308565362828));
#34529=CARTESIAN_POINT('Ctrl Pts',(80.3096882702486,150.809621939635,47.1504412801734));
#34530=CARTESIAN_POINT('Ctrl Pts',(78.6760969413907,150.986718511633,45.670026024064));
#34531=CARTESIAN_POINT('Ctrl Pts',(76.4041347530367,151.163815083632,44.9197069006017));
#34532=CARTESIAN_POINT('Ctrl Pts',(74.2101800112144,151.340911655631,45.1360689838698));
#34533=CARTESIAN_POINT('Ctrl Pts',(72.016225269392,151.51800822763,45.3524310671378));
#34534=CARTESIAN_POINT('Ctrl Pts',(69.9345925076917,151.695104799628,46.5320903475062));
#34535=CARTESIAN_POINT('Ctrl Pts',(68.6216467656562,151.872201371627,48.3030853894846));
#34536=CARTESIAN_POINT('Ctrl Pts',(67.3087010236208,152.049297943626,50.0740804314629));
#34537=CARTESIAN_POINT('Ctrl Pts',(66.7849774198233,152.226394515624,52.4087119996486));
#34538=CARTESIAN_POINT('Ctrl Pts',(67.2156126057621,152.403491087623,54.5708413428823));
#34539=CARTESIAN_POINT('Ctrl Pts',(67.6462477917008,152.580587659622,56.7329706861161));
#34540=CARTESIAN_POINT('Ctrl Pts',(69.024506420802,152.757684231621,58.6887810357286));
#34541=CARTESIAN_POINT('Ctrl Pts',(70.915806180453,152.934780803619,59.8215807441437));
#34542=CARTESIAN_POINT('Ctrl Pts',(72.8071059401039,153.111877375618,60.9543804525587));
#34543=CARTESIAN_POINT('Ctrl Pts',(75.1818659698178,153.288973947617,61.2464519739652));
#34544=CARTESIAN_POINT('Ctrl Pts',(77.2912945088738,153.466070519616,60.6057014773933));
#34545=CARTESIAN_POINT('Ctrl Pts',(79.4007230479297,153.643167091614,59.9649509808214));
#34546=CARTESIAN_POINT('Ctrl Pts',(81.2118275942127,153.820263663613,58.4014001198717));
#34547=CARTESIAN_POINT('Ctrl Pts',(82.1535440633131,153.997360235612,56.4080561826481));
#34548=CARTESIAN_POINT('Ctrl Pts',(82.6515697929933,154.091017564954,55.3538784110863));
#34549=CARTESIAN_POINT('Ctrl Pts',(82.91294989487,154.184674894296,54.1887099277253));
#34550=CARTESIAN_POINT('Ctrl Pts',(82.9129498948689,154.278332223638,53.0228109606281));
#34551=CARTESIAN_POINT('Ctrl Pts',(82.9129498948689,155.721667776361,53.0228109606419));
#34552=CARTESIAN_POINT('Ctrl Pts',(82.9129498948672,155.544571204362,55.2274084205516));
#34553=CARTESIAN_POINT('Ctrl Pts',(81.9432795991073,155.367474632364,57.4147653849869));
#34554=CARTESIAN_POINT('Ctrl Pts',(80.3096882702499,155.190378060365,58.8951806410965));
#34555=CARTESIAN_POINT('Ctrl Pts',(78.6760969413925,155.013281488366,60.3755958972062));
#34556=CARTESIAN_POINT('Ctrl Pts',(76.4041347530389,154.836184916368,61.125915020669));
#34557=CARTESIAN_POINT('Ctrl Pts',(74.2101800112166,154.659088344369,60.9095529374016));
#34558=CARTESIAN_POINT('Ctrl Pts',(72.0162252693943,154.48199177237,60.6931908541342));
#34559=CARTESIAN_POINT('Ctrl Pts',(69.9345925076938,154.304895200371,59.5135315737665));
#34560=CARTESIAN_POINT('Ctrl Pts',(68.6216467656578,154.127798628373,57.7425365317887));
#34561=CARTESIAN_POINT('Ctrl Pts',(67.3087010236219,153.950702056374,55.971541489811));
#34562=CARTESIAN_POINT('Ctrl Pts',(66.7849774198236,153.773605484375,53.6369099216257));
#34563=CARTESIAN_POINT('Ctrl Pts',(67.2156126057614,153.596508912377,51.4747805783919));
#34564=CARTESIAN_POINT('Ctrl Pts',(67.6462477916993,153.419412340378,49.3126512351581));
#34565=CARTESIAN_POINT('Ctrl Pts',(69.0245064207996,153.242315768379,47.3568408855451));
#34566=CARTESIAN_POINT('Ctrl Pts',(70.9158061804499,153.06521919638,46.2240411771293));
#34567=CARTESIAN_POINT('Ctrl Pts',(72.8071059401002,152.888122624382,45.0912414687135));
#34568=CARTESIAN_POINT('Ctrl Pts',(75.1818659698138,152.711026052383,44.7991699473059));
#34569=CARTESIAN_POINT('Ctrl Pts',(77.2912945088699,152.533929480384,45.4399204438766));
#34570=CARTESIAN_POINT('Ctrl Pts',(79.400723047926,152.356832908386,46.0806709404474));
#34571=CARTESIAN_POINT('Ctrl Pts',(81.2118275942097,152.179736336387,47.6442218013961));
#34572=CARTESIAN_POINT('Ctrl Pts',(82.1535440633112,152.002639764388,49.637565738619));
#34573=CARTESIAN_POINT('Ctrl Pts',(82.6515697929924,151.908982435046,50.6917435101814));
#34574=CARTESIAN_POINT('Ctrl Pts',(82.9129498948698,151.815325105703,51.8569119935435));
#34575=CARTESIAN_POINT('Ctrl Pts',(82.9129498948689,151.721667776361,53.0228109606417));
#34576=CARTESIAN_POINT('Origin',(74.9879498948689,255.,53.0228109606356));
#34577=CARTESIAN_POINT('',(82.9101577115551,146.278332223638,53.0299467479158));
#34578=CARTESIAN_POINT('',(82.9129498948689,147.721667776361,53.0228109606416));
#34579=CARTESIAN_POINT('',(82.9129498948689,255.,53.0228109606356));
#34580=CARTESIAN_POINT('Ctrl Pts',(82.9101577115551,146.278332223638,53.0299467479158));
#34581=CARTESIAN_POINT('Ctrl Pts',(82.8934310719895,146.435182126421,51.0768094606804));
#34582=CARTESIAN_POINT('Ctrl Pts',(82.1655901552695,146.592032029204,49.1121571431887));
#34583=CARTESIAN_POINT('Ctrl Pts',(80.8558380248122,146.748881931987,47.6756344998972));
#34584=CARTESIAN_POINT('Ctrl Pts',(79.0842603536104,146.96103794154,45.7325863613593));
#34585=CARTESIAN_POINT('Ctrl Pts',(76.248052204302,147.173193951092,44.7557731642908));
#34586=CARTESIAN_POINT('Ctrl Pts',(73.657958079385,147.385349960644,45.1960834592049));
#34587=CARTESIAN_POINT('Ctrl Pts',(71.067863954468,147.597505970197,45.6363937541189));
#34588=CARTESIAN_POINT('Ctrl Pts',(68.7238838539422,147.809661979749,47.4938275410156));
#34589=CARTESIAN_POINT('Ctrl Pts',(67.6878907853398,148.021817989301,49.9122239656804));
#34590=CARTESIAN_POINT('Ctrl Pts',(67.1698942510386,148.127895994077,51.1214221780127));
#34591=CARTESIAN_POINT('Ctrl Pts',(66.9788944747182,148.233973998854,52.4708610497871));
#34592=CARTESIAN_POINT('Ctrl Pts',(67.1071136457221,148.34005200363,53.7892545711937));
#34593=CARTESIAN_POINT('Ctrl Pts',(67.235332816726,148.446130008406,55.1076480926003));
#34594=CARTESIAN_POINT('Ctrl Pts',(67.6827709350543,148.552208013182,56.3949962636391));
#34595=CARTESIAN_POINT('Ctrl Pts',(68.4240556941093,148.658286017958,57.4817242113098));
#34596=CARTESIAN_POINT('Ctrl Pts',(69.9066252122194,148.87044202751,59.6551801066513));
#34597=CARTESIAN_POINT('Ctrl Pts',(72.5645812932367,149.082598037063,61.0261551085201));
#34598=CARTESIAN_POINT('Ctrl Pts',(75.1909799153373,149.294754046615,60.9591401134426));
#34599=CARTESIAN_POINT('Ctrl Pts',(77.8173785374379,149.506910056167,60.8921251183651));
#34600=CARTESIAN_POINT('Ctrl Pts',(80.4122197006218,149.71906606572,59.3871201263413));
#34601=CARTESIAN_POINT('Ctrl Pts',(81.7762013420966,149.931222075272,57.1391259992369));
#34602=CARTESIAN_POINT('Ctrl Pts',(82.5200751089225,150.046925458061,55.9131389270623));
#34603=CARTESIAN_POINT('Ctrl Pts',(82.8978571389894,150.16262884085,54.4661662931259));
#34604=CARTESIAN_POINT('Ctrl Pts',(82.9003953240663,150.278332223638,53.0207594678455));
#34605=CARTESIAN_POINT('Ctrl Pts',(82.9129498948689,151.721667776361,53.0228109606417));
#34606=CARTESIAN_POINT('Ctrl Pts',(82.9129498948672,151.544571204362,55.2274084205517));
#34607=CARTESIAN_POINT('Ctrl Pts',(81.9432795991071,151.367474632364,57.4147653849873));
#34608=CARTESIAN_POINT('Ctrl Pts',(80.3096882702494,151.190378060365,58.895180641097));
#34609=CARTESIAN_POINT('Ctrl Pts',(78.6760969413916,151.013281488366,60.3755958972067));
#34610=CARTESIAN_POINT('Ctrl Pts',(76.4041347530375,150.836184916367,61.1259150206693));
#34611=CARTESIAN_POINT('Ctrl Pts',(74.210180011215,150.659088344369,60.9095529374014));
#34612=CARTESIAN_POINT('Ctrl Pts',(72.0162252693925,150.48199177237,60.6931908541336));
#34613=CARTESIAN_POINT('Ctrl Pts',(69.9345925076919,150.304895200371,59.5135315737651));
#34614=CARTESIAN_POINT('Ctrl Pts',(68.6216467656563,150.127798628372,57.7425365317867));
#34615=CARTESIAN_POINT('Ctrl Pts',(67.3087010236207,149.950702056374,55.9715414898083));
#34616=CARTESIAN_POINT('Ctrl Pts',(66.7849774198233,149.773605484375,53.6369099216224));
#34617=CARTESIAN_POINT('Ctrl Pts',(67.2156126057621,149.596508912376,51.4747805783885));
#34618=CARTESIAN_POINT('Ctrl Pts',(67.6462477917009,149.419412340378,49.3126512351547));
#34619=CARTESIAN_POINT('Ctrl Pts',(69.0245064208024,149.242315768379,47.356840885542));
#34620=CARTESIAN_POINT('Ctrl Pts',(70.9158061804536,149.06521919638,46.2240411771271));
#34621=CARTESIAN_POINT('Ctrl Pts',(72.8071059401047,148.888122624381,45.0912414687122));
#34622=CARTESIAN_POINT('Ctrl Pts',(75.1818659698189,148.711026052383,44.7991699473059));
#34623=CARTESIAN_POINT('Ctrl Pts',(77.2912945088749,148.533929480384,45.4399204438782));
#34624=CARTESIAN_POINT('Ctrl Pts',(79.4007230479309,148.356832908385,46.0806709404504));
#34625=CARTESIAN_POINT('Ctrl Pts',(81.2118275942137,148.179736336386,47.6442218014006));
#34626=CARTESIAN_POINT('Ctrl Pts',(82.1535440633138,148.002639764388,49.6375657386245));
#34627=CARTESIAN_POINT('Ctrl Pts',(82.6515697929933,147.908982435045,50.6917435101854));
#34628=CARTESIAN_POINT('Ctrl Pts',(82.9129498948698,147.815325105703,51.8569119935454));
#34629=CARTESIAN_POINT('Ctrl Pts',(82.9129498948689,147.721667776361,53.0228109606416));
#34630=CARTESIAN_POINT('Origin',(74.9879498948689,255.,53.0228109606356));
#34631=CARTESIAN_POINT('',(82.9265740259991,142.278332223638,53.0227242078164));
#34632=CARTESIAN_POINT('',(82.9129498948689,143.721667776361,53.0228109606414));
#34633=CARTESIAN_POINT('',(82.9129498948689,255.,53.0228109606356));
#34634=CARTESIAN_POINT('Ctrl Pts',(82.9265740259991,142.278332223638,53.0227242078164));
#34635=CARTESIAN_POINT('Ctrl Pts',(82.9266987001804,142.283423392889,52.959623945468));
#34636=CARTESIAN_POINT('Ctrl Pts',(82.926004395604,142.288514562139,52.8965249331533));
#34637=CARTESIAN_POINT('Ctrl Pts',(82.9244823469275,142.293605731389,52.8334440014662));
#34638=CARTESIAN_POINT('Ctrl Pts',(82.8610564897863,142.505761740941,50.2047750085305));
#34639=CARTESIAN_POINT('Ctrl Pts',(81.3602502928963,142.717917750493,47.6075030844636));
#34640=CARTESIAN_POINT('Ctrl Pts',(79.1160122844355,142.930073760046,46.241539507674));
#34641=CARTESIAN_POINT('Ctrl Pts',(76.8717742759746,143.142229769598,44.8755759308844));
#34642=CARTESIAN_POINT('Ctrl Pts',(73.8841044559424,143.35438577915,44.7409207013721));
#34643=CARTESIAN_POINT('Ctrl Pts',(71.5161226428102,143.566541788703,45.8874742490525));
#34644=CARTESIAN_POINT('Ctrl Pts',(70.3321317362438,143.672619793479,46.4607510228928));
#34645=CARTESIAN_POINT('Ctrl Pts',(69.3030628314027,143.778697798255,47.3543299910311));
#34646=CARTESIAN_POINT('Ctrl Pts',(68.5353606985202,143.884775803031,48.4337905360573));
#34647=CARTESIAN_POINT('Ctrl Pts',(67.7676585656378,143.990853807807,49.5132510810832));
#34648=CARTESIAN_POINT('Ctrl Pts',(67.2613232047143,144.096931812583,50.7785932029967));
#34649=CARTESIAN_POINT('Ctrl Pts',(67.108393547461,144.20300981736,52.0851509882432));
#34650=CARTESIAN_POINT('Ctrl Pts',(66.8025342329545,144.415165826912,54.6982665587361));
#34651=CARTESIAN_POINT('Ctrl Pts',(67.910297733129,144.627321836464,57.4762447825611));
#34652=CARTESIAN_POINT('Ctrl Pts',(69.9371654396076,144.839477846017,59.1478512051887));
#34653=CARTESIAN_POINT('Ctrl Pts',(71.9640331460865,145.051633855569,60.8194576278166));
#34654=CARTESIAN_POINT('Ctrl Pts',(74.9100050588693,145.263789865121,61.384692249247));
#34655=CARTESIAN_POINT('Ctrl Pts',(77.4138798670197,145.475945874673,60.5818632145908));
#34656=CARTESIAN_POINT('Ctrl Pts',(79.9177546751699,145.688101884226,59.7790341799346));
#34657=CARTESIAN_POINT('Ctrl Pts',(81.9795323786876,145.900257893778,57.6081414891914));
#34658=CARTESIAN_POINT('Ctrl Pts',(82.6569476338984,146.11241390333,55.0680536038164));
#34659=CARTESIAN_POINT('Ctrl Pts',(82.8335403239236,146.1677200101,54.4058881903149));
#34660=CARTESIAN_POINT('Ctrl Pts',(82.9160556132897,146.223026116869,53.7186333038295));
#34661=CARTESIAN_POINT('Ctrl Pts',(82.9101577115551,146.278332223638,53.0299467479158));
#34662=CARTESIAN_POINT('Ctrl Pts',(82.9129498948689,147.721667776361,53.0228109606416));
#34663=CARTESIAN_POINT('Ctrl Pts',(82.9129498948672,147.544571204362,55.2274084205511));
#34664=CARTESIAN_POINT('Ctrl Pts',(81.9432795991076,147.367474632364,57.4147653849863));
#34665=CARTESIAN_POINT('Ctrl Pts',(80.3096882702505,147.190378060365,58.895180641096));
#34666=CARTESIAN_POINT('Ctrl Pts',(78.6760969413934,147.013281488366,60.3755958972057));
#34667=CARTESIAN_POINT('Ctrl Pts',(76.40413475304,146.836184916368,61.1259150206688));
#34668=CARTESIAN_POINT('Ctrl Pts',(74.2101800112178,146.659088344369,60.9095529374017));
#34669=CARTESIAN_POINT('Ctrl Pts',(72.0162252693957,146.48199177237,60.6931908541347));
#34670=CARTESIAN_POINT('Ctrl Pts',(69.9345925076951,146.304895200372,59.5135315737675));
#34671=CARTESIAN_POINT('Ctrl Pts',(68.6216467656588,146.127798628373,57.7425365317901));
#34672=CARTESIAN_POINT('Ctrl Pts',(67.3087010236226,145.950702056374,55.9715414898127));
#34673=CARTESIAN_POINT('Ctrl Pts',(66.7849774198238,145.773605484375,53.6369099216277));
#34674=CARTESIAN_POINT('Ctrl Pts',(67.215612605761,145.596508912377,51.474780578394));
#34675=CARTESIAN_POINT('Ctrl Pts',(67.6462477916982,145.419412340378,49.3126512351603));
#34676=CARTESIAN_POINT('Ctrl Pts',(69.0245064207979,145.242315768379,47.356840885547));
#34677=CARTESIAN_POINT('Ctrl Pts',(70.9158061804476,145.065219196381,46.2240411771307));
#34678=CARTESIAN_POINT('Ctrl Pts',(72.8071059400974,144.888122624382,45.0912414687143));
#34679=CARTESIAN_POINT('Ctrl Pts',(75.1818659698108,144.711026052383,44.7991699473058));
#34680=CARTESIAN_POINT('Ctrl Pts',(77.291294508867,144.533929480384,45.4399204438757));
#34681=CARTESIAN_POINT('Ctrl Pts',(79.4007230479233,144.356832908386,46.0806709404456));
#34682=CARTESIAN_POINT('Ctrl Pts',(81.2118275942074,144.179736336387,47.6442218013935));
#34683=CARTESIAN_POINT('Ctrl Pts',(82.1535440633097,144.002639764388,49.6375657386158));
#34684=CARTESIAN_POINT('Ctrl Pts',(82.6515697929918,143.908982435046,50.691743510179));
#34685=CARTESIAN_POINT('Ctrl Pts',(82.9129498948698,143.815325105704,51.8569119935421));
#34686=CARTESIAN_POINT('Ctrl Pts',(82.9129498948689,143.721667776361,53.0228109606414));
#34687=CARTESIAN_POINT('Origin',(74.9879498948689,255.,53.0228109606356));
#34688=CARTESIAN_POINT('',(82.911308479162,138.278332223639,53.0202043904445));
#34689=CARTESIAN_POINT('',(82.9151797848103,139.721667776361,53.0223168535823));
#34690=CARTESIAN_POINT('',(82.9129498948689,255.,53.0228109606356));
#34691=CARTESIAN_POINT('Ctrl Pts',(82.9074078591984,138.278332223639,53.0140102011414));
#34692=CARTESIAN_POINT('Ctrl Pts',(82.9139627399995,138.343820668908,52.1971816301529));
#34693=CARTESIAN_POINT('Ctrl Pts',(82.7978356043124,138.409309114178,51.3824531381546));
#34694=CARTESIAN_POINT('Ctrl Pts',(82.5512943919456,138.474797559447,50.6098539304659));
#34695=CARTESIAN_POINT('Ctrl Pts',(81.7526008271395,138.686953568999,48.1069457577048));
#34696=CARTESIAN_POINT('Ctrl Pts',(79.5852150792516,138.899109578552,46.0461832764327));
#34697=CARTESIAN_POINT('Ctrl Pts',(77.0455679583654,139.111265588104,45.3590767298199));
#34698=CARTESIAN_POINT('Ctrl Pts',(75.7757443979224,139.21734359288,45.0155234565135));
#34699=CARTESIAN_POINT('Ctrl Pts',(74.4128554942297,139.323421597656,45.0153841668718));
#34700=CARTESIAN_POINT('Ctrl Pts',(73.1254101059182,139.429499602433,45.3269704393795));
#34701=CARTESIAN_POINT('Ctrl Pts',(71.8379647176066,139.535577607209,45.6385567118871));
#34702=CARTESIAN_POINT('Ctrl Pts',(70.625962844676,139.641655611985,46.2618685465441));
#34703=CARTESIAN_POINT('Ctrl Pts',(69.6537551006523,139.747733616761,47.1480360412744));
#34704=CARTESIAN_POINT('Ctrl Pts',(67.7093396126049,139.959889626313,48.9203710307349));
#34705=CARTESIAN_POINT('Ctrl Pts',(66.7241006401847,140.172045635866,51.744128660488));
#34706=CARTESIAN_POINT('Ctrl Pts',(67.1582616853377,140.384201645418,54.3352606367889));
#34707=CARTESIAN_POINT('Ctrl Pts',(67.5924227304907,140.59635765497,56.9263926130896));
#34708=CARTESIAN_POINT('Ctrl Pts',(69.4459837932168,140.808513664523,59.2848989359379));
#34709=CARTESIAN_POINT('Ctrl Pts',(71.8628400550648,141.020669674075,60.3206254072329));
#34710=CARTESIAN_POINT('Ctrl Pts',(74.2796963169129,141.232825683627,61.3563518785279));
#34711=CARTESIAN_POINT('Ctrl Pts',(77.2598477778832,141.444981693179,61.0692984982696));
#34712=CARTESIAN_POINT('Ctrl Pts',(79.436900749672,141.657137702732,59.5957387772383));
#34713=CARTESIAN_POINT('Ctrl Pts',(81.5617103503248,141.864202543034,58.1575404959124));
#34714=CARTESIAN_POINT('Ctrl Pts',(82.9215033559457,142.071267383336,55.5890984735887));
#34715=CARTESIAN_POINT('Ctrl Pts',(82.9265740259991,142.278332223638,53.0227242078164));
#34716=CARTESIAN_POINT('Ctrl Pts',(82.9129498948689,143.721667776361,53.0228109606414));
#34717=CARTESIAN_POINT('Ctrl Pts',(82.9129498948673,143.544571204362,55.2274084205511));
#34718=CARTESIAN_POINT('Ctrl Pts',(81.9432795991076,143.367474632364,57.4147653849865));
#34719=CARTESIAN_POINT('Ctrl Pts',(80.3096882702503,143.190378060365,58.8951806410962));
#34720=CARTESIAN_POINT('Ctrl Pts',(78.676096941393,143.013281488366,60.3755958972059));
#34721=CARTESIAN_POINT('Ctrl Pts',(76.4041347530394,142.836184916368,61.1259150206689));
#34722=CARTESIAN_POINT('Ctrl Pts',(74.2101800112171,142.659088344369,60.9095529374017));
#34723=CARTESIAN_POINT('Ctrl Pts',(72.0162252693948,142.48199177237,60.6931908541344));
#34724=CARTESIAN_POINT('Ctrl Pts',(69.9345925076942,142.304895200371,59.5135315737668));
#34725=CARTESIAN_POINT('Ctrl Pts',(68.6216467656581,142.127798628373,57.7425365317891));
#34726=CARTESIAN_POINT('Ctrl Pts',(67.308701023622,141.950702056374,55.9715414898115));
#34727=CARTESIAN_POINT('Ctrl Pts',(66.7849774198236,141.773605484375,53.6369099216262));
#34728=CARTESIAN_POINT('Ctrl Pts',(67.2156126057613,141.596508912377,51.4747805783924));
#34729=CARTESIAN_POINT('Ctrl Pts',(67.646247791699,141.419412340378,49.3126512351586));
#34730=CARTESIAN_POINT('Ctrl Pts',(69.0245064207992,141.242315768379,47.3568408855455));
#34731=CARTESIAN_POINT('Ctrl Pts',(70.9158061804494,141.06521919638,46.2240411771296));
#34732=CARTESIAN_POINT('Ctrl Pts',(72.8071059400996,140.888122624382,45.0912414687136));
#34733=CARTESIAN_POINT('Ctrl Pts',(75.1818659698132,140.711026052383,44.7991699473059));
#34734=CARTESIAN_POINT('Ctrl Pts',(77.2912945088694,140.533929480384,45.4399204438765));
#34735=CARTESIAN_POINT('Ctrl Pts',(79.4007230479256,140.356832908386,46.0806709404471));
#34736=CARTESIAN_POINT('Ctrl Pts',(81.2118275942094,140.179736336387,47.6442218013957));
#34737=CARTESIAN_POINT('Ctrl Pts',(82.153544063311,140.002639764388,49.6375657386185));
#34738=CARTESIAN_POINT('Ctrl Pts',(82.6515697929922,139.908982435046,50.6917435101809));
#34739=CARTESIAN_POINT('Ctrl Pts',(82.9129498948697,139.815325105704,51.8569119935429));
#34740=CARTESIAN_POINT('Ctrl Pts',(82.9129498948689,139.721667776361,53.0228109606412));
#34741=CARTESIAN_POINT('Origin',(74.9879498948689,255.,53.0228109606356));
#34742=CARTESIAN_POINT('',(82.9084961307343,134.278332223638,53.0246083443181));
#34743=CARTESIAN_POINT('',(82.9105909927084,135.721667776361,53.0215876101194));
#34744=CARTESIAN_POINT('',(82.9129498948689,255.,53.0228109606356));
#34745=CARTESIAN_POINT('Ctrl Pts',(82.9129498948689,134.278332223638,53.0228109606272));
#34746=CARTESIAN_POINT('Ctrl Pts',(82.9129498948666,134.455428795637,50.8182135007174));
#34747=CARTESIAN_POINT('Ctrl Pts',(81.943279599106,134.632525367636,48.6308565362822));
#34748=CARTESIAN_POINT('Ctrl Pts',(80.3096882702481,134.809621939635,47.1504412801729));
#34749=CARTESIAN_POINT('Ctrl Pts',(78.6760969413901,134.986718511633,45.6700260240637));
#34750=CARTESIAN_POINT('Ctrl Pts',(76.404134753036,135.163815083632,44.9197069006016));
#34751=CARTESIAN_POINT('Ctrl Pts',(74.2101800112137,135.340911655631,45.1360689838698));
#34752=CARTESIAN_POINT('Ctrl Pts',(72.0162252693913,135.51800822763,45.352431067138));
#34753=CARTESIAN_POINT('Ctrl Pts',(69.9345925076911,135.695104799628,46.5320903475067));
#34754=CARTESIAN_POINT('Ctrl Pts',(68.6216467656558,135.872201371627,48.3030853894851));
#34755=CARTESIAN_POINT('Ctrl Pts',(67.3087010236205,136.049297943626,50.0740804314636));
#34756=CARTESIAN_POINT('Ctrl Pts',(66.7849774198233,136.226394515624,52.4087119996493));
#34757=CARTESIAN_POINT('Ctrl Pts',(67.2156126057622,136.403491087623,54.570841342883));
#34758=CARTESIAN_POINT('Ctrl Pts',(67.6462477917011,136.580587659622,56.7329706861167));
#34759=CARTESIAN_POINT('Ctrl Pts',(69.0245064208025,136.757684231621,58.6887810357291));
#34760=CARTESIAN_POINT('Ctrl Pts',(70.9158061804535,136.934780803619,59.821580744144));
#34761=CARTESIAN_POINT('Ctrl Pts',(72.8071059401046,137.111877375618,60.9543804525589));
#34762=CARTESIAN_POINT('Ctrl Pts',(75.1818659698185,137.288973947617,61.2464519739652));
#34763=CARTESIAN_POINT('Ctrl Pts',(77.2912945088744,137.466070519616,60.6057014773931));
#34764=CARTESIAN_POINT('Ctrl Pts',(79.4007230479303,137.643167091614,59.9649509808211));
#34765=CARTESIAN_POINT('Ctrl Pts',(81.2118275942132,137.820263663613,58.4014001198711));
#34766=CARTESIAN_POINT('Ctrl Pts',(82.1535440633134,137.997360235612,56.4080561826475));
#34767=CARTESIAN_POINT('Ctrl Pts',(82.6515697929935,138.091017564954,55.3538784110857));
#34768=CARTESIAN_POINT('Ctrl Pts',(82.9129498948701,138.184674894296,54.1887099277246));
#34769=CARTESIAN_POINT('Ctrl Pts',(82.9129498948689,138.278332223638,53.0228109606274));
#34770=CARTESIAN_POINT('Ctrl Pts',(82.9245648731632,139.721667776361,53.0202372717949));
#34771=CARTESIAN_POINT('Ctrl Pts',(82.909178717574,139.526581028984,55.437258796622));
#34772=CARTESIAN_POINT('Ctrl Pts',(81.7198417702367,139.331494281607,57.8629826494013));
#34773=CARTESIAN_POINT('Ctrl Pts',(79.7986919370961,139.13640753423,59.3333874365964));
#34774=CARTESIAN_POINT('Ctrl Pts',(78.7540707933465,139.030329529453,60.1329169184087));
#34775=CARTESIAN_POINT('Ctrl Pts',(77.4930805681288,138.924251524677,60.6499950895933));
#34776=CARTESIAN_POINT('Ctrl Pts',(76.183657351348,138.818173519901,60.8500262683011));
#34777=CARTESIAN_POINT('Ctrl Pts',(74.874234134567,138.712095515125,61.0500574470088));
#34778=CARTESIAN_POINT('Ctrl Pts',(73.5163779262234,138.606017510349,60.9330416332398));
#34779=CARTESIAN_POINT('Ctrl Pts',(72.2806943133818,138.499939505573,60.4818579287348));
#34780=CARTESIAN_POINT('Ctrl Pts',(69.8093270876987,138.28778349602,59.5794905197248));
#34781=CARTESIAN_POINT('Ctrl Pts',(67.8266502440253,138.075627486468,57.3404515477713));
#34782=CARTESIAN_POINT('Ctrl Pts',(67.2455404690043,137.863471476916,54.7782704142227));
#34783=CARTESIAN_POINT('Ctrl Pts',(66.6644306939832,137.651315467363,52.2160892806742));
#34784=CARTESIAN_POINT('Ctrl Pts',(67.4848879876146,137.439159457811,49.3307659855306));
#34785=CARTESIAN_POINT('Ctrl Pts',(69.3282823691089,137.227003448259,47.4557138081096));
#34786=CARTESIAN_POINT('Ctrl Pts',(71.1716767506032,137.014847438706,45.5806616306886));
#34787=CARTESIAN_POINT('Ctrl Pts',(74.0380082199606,136.802691429154,44.71588057099));
#34788=CARTESIAN_POINT('Ctrl Pts',(76.6113017439743,136.590535419602,45.2535592228728));
#34789=CARTESIAN_POINT('Ctrl Pts',(79.1845952679878,136.378379410049,45.7912378747556));
#34790=CARTESIAN_POINT('Ctrl Pts',(81.4648508466579,136.166223400497,47.7313762382197));
#34791=CARTESIAN_POINT('Ctrl Pts',(82.4032294849873,135.954067390945,50.187667964563));
#34792=CARTESIAN_POINT('Ctrl Pts',(82.7458685871294,135.87660085275,51.0845570851549));
#34793=CARTESIAN_POINT('Ctrl Pts',(82.9095994626181,135.799134314556,52.0502633081634));
#34794=CARTESIAN_POINT('Ctrl Pts',(82.9035238655686,135.721667776361,53.0179225264982));
#34795=CARTESIAN_POINT('Origin',(74.9879498948689,255.,53.0228109606356));
#34796=CARTESIAN_POINT('',(82.9145063072273,130.278332223638,53.0234757497479));
#34797=CARTESIAN_POINT('',(82.9112639633797,131.721667776361,53.0239353364917));
#34798=CARTESIAN_POINT('',(82.9129498948689,255.,53.0228109606356));
#34799=CARTESIAN_POINT('Ctrl Pts',(82.9208881629639,130.278332223638,53.0262016265857));
#34800=CARTESIAN_POINT('Ctrl Pts',(82.9158838709538,130.358537216171,52.0302352857169));
#34801=CARTESIAN_POINT('Ctrl Pts',(82.716706393915,130.438742208703,51.0317289921228));
#34802=CARTESIAN_POINT('Ctrl Pts',(82.3471180811525,130.518947201235,50.1008836172503));
#34803=CARTESIAN_POINT('Ctrl Pts',(81.8583057320879,130.625025206011,48.8697605037879));
#34804=CARTESIAN_POINT('Ctrl Pts',(81.0714049762425,130.731103210788,47.7569921614725));
#34805=CARTESIAN_POINT('Ctrl Pts',(80.0578201388033,130.837181215564,46.9184657733554));
#34806=CARTESIAN_POINT('Ctrl Pts',(78.0306504639246,131.049337225116,45.2414129971209));
#34807=CARTESIAN_POINT('Ctrl Pts',(75.0967444626701,131.261493234668,44.6613280376804));
#34808=CARTESIAN_POINT('Ctrl Pts',(72.5919475119749,131.473649244221,45.4540782931361));
#34809=CARTESIAN_POINT('Ctrl Pts',(70.0871505612799,131.685805253773,46.2468285485919));
#34810=CARTESIAN_POINT('Ctrl Pts',(68.0114626611442,131.897961263325,48.4124140189437));
#34811=CARTESIAN_POINT('Ctrl Pts',(67.324404396993,132.110117272878,50.9504988196226));
#34812=CARTESIAN_POINT('Ctrl Pts',(66.6373461328418,132.32227328243,53.4885836203017));
#34813=CARTESIAN_POINT('Ctrl Pts',(67.3389175046757,132.534429291982,56.3991677513083));
#34814=CARTESIAN_POINT('Ctrl Pts',(69.1028352259173,132.746585301535,58.348406619716));
#34815=CARTESIAN_POINT('Ctrl Pts',(70.8667529471589,132.958741311087,60.2976454881235));
#34816=CARTESIAN_POINT('Ctrl Pts',(73.6930170178079,133.170897320639,61.2855390939326));
#34817=CARTESIAN_POINT('Ctrl Pts',(76.2868996221862,133.383053330192,60.8546138701645));
#34818=CARTESIAN_POINT('Ctrl Pts',(78.8807822265645,133.595209339744,60.4236886463964));
#34819=CARTESIAN_POINT('Ctrl Pts',(81.2422833646718,133.807365349296,58.5739445930511));
#34820=CARTESIAN_POINT('Ctrl Pts',(82.2804982552316,134.019521358848,56.1605298809147));
#34821=CARTESIAN_POINT('Ctrl Pts',(82.702673889459,134.105791647112,55.1791483807895));
#34822=CARTESIAN_POINT('Ctrl Pts',(82.9060403020962,134.192061935375,54.1045623012985));
#34823=CARTESIAN_POINT('Ctrl Pts',(82.9001107603132,134.278332223638,53.027992387025));
#34824=CARTESIAN_POINT('Ctrl Pts',(82.9129498948689,135.721667776361,53.022810960641));
#34825=CARTESIAN_POINT('Ctrl Pts',(82.9129498948674,135.544571204363,55.2274084205507));
#34826=CARTESIAN_POINT('Ctrl Pts',(81.9432795991078,135.367474632364,57.4147653849862));
#34827=CARTESIAN_POINT('Ctrl Pts',(80.3096882702505,135.190378060365,58.895180641096));
#34828=CARTESIAN_POINT('Ctrl Pts',(78.6760969413933,135.013281488366,60.3755958972058));
#34829=CARTESIAN_POINT('Ctrl Pts',(76.4041347530397,134.836184916368,61.1259150206688));
#34830=CARTESIAN_POINT('Ctrl Pts',(74.2101800112174,134.659088344369,60.9095529374017));
#34831=CARTESIAN_POINT('Ctrl Pts',(72.0162252693952,134.48199177237,60.6931908541345));
#34832=CARTESIAN_POINT('Ctrl Pts',(69.9345925076945,134.304895200372,59.513531573767));
#34833=CARTESIAN_POINT('Ctrl Pts',(68.6216467656583,134.127798628373,57.7425365317894));
#34834=CARTESIAN_POINT('Ctrl Pts',(67.3087010236222,133.950702056374,55.9715414898118));
#34835=CARTESIAN_POINT('Ctrl Pts',(66.7849774198237,133.773605484375,53.6369099216266));
#34836=CARTESIAN_POINT('Ctrl Pts',(67.2156126057613,133.596508912377,51.4747805783927));
#34837=CARTESIAN_POINT('Ctrl Pts',(67.6462477916989,133.419412340378,49.3126512351589));
#34838=CARTESIAN_POINT('Ctrl Pts',(69.024506420799,133.242315768379,47.3568408855458));
#34839=CARTESIAN_POINT('Ctrl Pts',(70.9158061804491,133.06521919638,46.2240411771298));
#34840=CARTESIAN_POINT('Ctrl Pts',(72.8071059400993,132.888122624382,45.0912414687137));
#34841=CARTESIAN_POINT('Ctrl Pts',(75.1818659698129,132.711026052383,44.7991699473059));
#34842=CARTESIAN_POINT('Ctrl Pts',(77.2912945088691,132.533929480384,45.4399204438764));
#34843=CARTESIAN_POINT('Ctrl Pts',(79.4007230479253,132.356832908386,46.0806709404469));
#34844=CARTESIAN_POINT('Ctrl Pts',(81.2118275942091,132.179736336387,47.6442218013954));
#34845=CARTESIAN_POINT('Ctrl Pts',(82.1535440633108,132.002639764388,49.6375657386182));
#34846=CARTESIAN_POINT('Ctrl Pts',(82.6515697929921,131.908982435046,50.6917435101806));
#34847=CARTESIAN_POINT('Ctrl Pts',(82.9129498948697,131.815325105704,51.8569119935426));
#34848=CARTESIAN_POINT('Ctrl Pts',(82.9129498948689,131.721667776361,53.0228109606409));
#34849=CARTESIAN_POINT('Origin',(74.9879498948689,255.,53.0228109606356));
#34850=CARTESIAN_POINT('',(82.9138193369606,126.278332223638,53.0221792875591));
#34851=CARTESIAN_POINT('',(82.9235377668022,127.721667776361,53.0258702510677));
#34852=CARTESIAN_POINT('',(82.9129498948689,255.,53.0228109606356));
#34853=CARTESIAN_POINT('Ctrl Pts',(82.9129498948689,126.278332223638,53.0228109606273));
#34854=CARTESIAN_POINT('Ctrl Pts',(82.9129498948666,126.455428795637,50.8182135007172));
#34855=CARTESIAN_POINT('Ctrl Pts',(81.9432795991058,126.632525367636,48.6308565362817));
#34856=CARTESIAN_POINT('Ctrl Pts',(80.3096882702475,126.809621939635,47.1504412801724));
#34857=CARTESIAN_POINT('Ctrl Pts',(78.6760969413891,126.986718511633,45.6700260240632));
#34858=CARTESIAN_POINT('Ctrl Pts',(76.4041347530346,127.163815083632,44.9197069006013));
#34859=CARTESIAN_POINT('Ctrl Pts',(74.210180011212,127.340911655631,45.13606898387));
#34860=CARTESIAN_POINT('Ctrl Pts',(72.0162252693894,127.51800822763,45.3524310671387));
#34861=CARTESIAN_POINT('Ctrl Pts',(69.9345925076892,127.695104799628,46.5320903475081));
#34862=CARTESIAN_POINT('Ctrl Pts',(68.6216467656543,127.872201371627,48.3030853894872));
#34863=CARTESIAN_POINT('Ctrl Pts',(67.3087010236194,128.049297943626,50.0740804314663));
#34864=CARTESIAN_POINT('Ctrl Pts',(66.784977419823,128.226394515625,52.4087119996526));
#34865=CARTESIAN_POINT('Ctrl Pts',(67.2156126057629,128.403491087624,54.5708413428864));
#34866=CARTESIAN_POINT('Ctrl Pts',(67.6462477917028,128.580587659622,56.7329706861202));
#34867=CARTESIAN_POINT('Ctrl Pts',(69.0245064208054,128.757684231621,58.6887810357323));
#34868=CARTESIAN_POINT('Ctrl Pts',(70.9158061804573,128.93478080362,59.8215807441463));
#34869=CARTESIAN_POINT('Ctrl Pts',(72.8071059401092,129.111877375619,60.9543804525602));
#34870=CARTESIAN_POINT('Ctrl Pts',(75.1818659698237,129.288973947617,61.2464519739651));
#34871=CARTESIAN_POINT('Ctrl Pts',(77.2912945088795,129.466070519616,60.6057014773916));
#34872=CARTESIAN_POINT('Ctrl Pts',(79.4007230479353,129.643167091615,59.964950980818));
#34873=CARTESIAN_POINT('Ctrl Pts',(81.2118275942172,129.820263663614,58.4014001198665));
#34874=CARTESIAN_POINT('Ctrl Pts',(82.153544063316,129.997360235612,56.4080561826419));
#34875=CARTESIAN_POINT('Ctrl Pts',(82.6515697929944,130.091017564954,55.3538784110816));
#34876=CARTESIAN_POINT('Ctrl Pts',(82.9129498948701,130.184674894296,54.1887099277226));
#34877=CARTESIAN_POINT('Ctrl Pts',(82.9129498948689,130.278332223638,53.0228109606275));
#34878=CARTESIAN_POINT('Ctrl Pts',(82.9051652400584,131.721667776361,53.0280026768235));
#34879=CARTESIAN_POINT('Ctrl Pts',(82.9116631823551,131.647375581023,53.9548329532724));
#34880=CARTESIAN_POINT('Ctrl Pts',(82.7614734299345,131.573083385685,54.8798174951143));
#34881=CARTESIAN_POINT('Ctrl Pts',(82.4455487077382,131.498791190346,55.7446903029458));
#34882=CARTESIAN_POINT('Ctrl Pts',(81.5433633829565,131.286635180794,58.2145051044087));
#34883=CARTESIAN_POINT('Ctrl Pts',(79.2896083620333,131.074479171242,60.1941083459282));
#34884=CARTESIAN_POINT('Ctrl Pts',(76.7260550880175,130.862323161689,60.7691347305574));
#34885=CARTESIAN_POINT('Ctrl Pts',(74.1625018140018,130.650167152137,61.3441611151866));
#34886=CARTESIAN_POINT('Ctrl Pts',(71.2891502868935,130.438011142585,60.5146106429257));
#34887=CARTESIAN_POINT('Ctrl Pts',(69.4132672444211,130.225855133032,58.6698923132104));
#34888=CARTESIAN_POINT('Ctrl Pts',(68.4753257231848,130.119777128256,57.7475331483527));
#34889=CARTESIAN_POINT('Ctrl Pts',(67.7867513231075,130.01369912348,56.5713820191313));
#34890=CARTESIAN_POINT('Ctrl Pts',(67.4053169315246,129.907621118704,55.3028752442113));
#34891=CARTESIAN_POINT('Ctrl Pts',(67.0238825399419,129.801543113928,54.0343684692913));
#34892=CARTESIAN_POINT('Ctrl Pts',(66.9495881568535,129.695465109152,52.6735060486728));
#34893=CARTESIAN_POINT('Ctrl Pts',(67.2232779325066,129.589387104375,51.3868146975871));
#34894=CARTESIAN_POINT('Ctrl Pts',(67.7706574838129,129.377231094823,48.8134319954155));
#34895=CARTESIAN_POINT('Ctrl Pts',(69.7099736700853,129.165075085271,46.5367335713753));
#34896=CARTESIAN_POINT('Ctrl Pts',(72.1655260602513,128.952919075718,45.6025370230583));
#34897=CARTESIAN_POINT('Ctrl Pts',(74.6210784504169,128.740763066166,44.6683404747414));
#34898=CARTESIAN_POINT('Ctrl Pts',(77.5928670444764,128.528607056614,45.0766458021476));
#34899=CARTESIAN_POINT('Ctrl Pts',(79.7075944750379,128.316451047062,46.6392882462806));
#34900=CARTESIAN_POINT('Ctrl Pts',(81.6838202101202,128.118189956828,48.0995871804121));
#34901=CARTESIAN_POINT('Ctrl Pts',(82.9115729772427,127.919928866595,50.5679706767429));
#34902=CARTESIAN_POINT('Ctrl Pts',(82.9235377668022,127.721667776361,53.0258702510677));
#34903=CARTESIAN_POINT('Origin',(74.9879498948689,255.,53.0228109606356));
#34904=CARTESIAN_POINT('',(82.9069886672033,122.278332223639,53.0212720983085));
#34905=CARTESIAN_POINT('',(82.9132333187719,123.721667776361,53.0218936349848));
#34906=CARTESIAN_POINT('',(82.9129498948689,255.,53.0228109606356));
#34907=CARTESIAN_POINT('Ctrl Pts',(82.8984425219126,122.278332223638,53.0190659519314));
#34908=CARTESIAN_POINT('Ctrl Pts',(82.9027496025291,122.373253763433,51.8339480579543));
#34909=CARTESIAN_POINT('Ctrl Pts',(82.65469030603,122.468175303228,50.6504444566772));
#34910=CARTESIAN_POINT('Ctrl Pts',(82.146555570156,122.563096843023,49.5904784597474));
#34911=CARTESIAN_POINT('Ctrl Pts',(81.0108403456583,122.775252852576,47.2213833454514));
#34912=CARTESIAN_POINT('Ctrl Pts',(78.575911790868,122.987408862128,45.4694234083418));
#34913=CARTESIAN_POINT('Ctrl Pts',(75.9666213292996,123.19956487168,45.1445745189417));
#34914=CARTESIAN_POINT('Ctrl Pts',(73.3573308677313,123.411720881233,44.8197256295416));
#34915=CARTESIAN_POINT('Ctrl Pts',(70.5736784993851,123.623876890785,45.9219877878507));
#34916=CARTESIAN_POINT('Ctrl Pts',(68.8906711024336,123.836032900337,47.9414986185291));
#34917=CARTESIAN_POINT('Ctrl Pts',(67.207663705482,124.04818890989,49.9610094492078));
#34918=CARTESIAN_POINT('Ctrl Pts',(66.6253012799254,124.260344919442,52.8977689522558));
#34919=CARTESIAN_POINT('Ctrl Pts',(67.4152328050517,124.472500928994,55.4057425763972));
#34920=CARTESIAN_POINT('Ctrl Pts',(68.205164330178,124.684656938547,57.9137162005383));
#34921=CARTESIAN_POINT('Ctrl Pts',(70.3673898059867,124.896812948099,59.9929039457728));
#34922=CARTESIAN_POINT('Ctrl Pts',(72.9024154550697,125.108968957651,60.6829080691138));
#34923=CARTESIAN_POINT('Ctrl Pts',(75.4374411041527,125.321124967204,61.3729121924548));
#34924=CARTESIAN_POINT('Ctrl Pts',(78.3452669265099,125.533280976756,60.6737326939024));
#34925=CARTESIAN_POINT('Ctrl Pts',(80.3024009664751,125.745436986308,58.9154524959155));
#34926=CARTESIAN_POINT('Ctrl Pts',(81.2809679864577,125.851514991084,58.0363123969221));
#34927=CARTESIAN_POINT('Ctrl Pts',(82.0218620608422,125.95759299586,56.89239712307));
#34928=CARTESIAN_POINT('Ctrl Pts',(82.4600916525821,126.063671000637,55.6423745400647));
#34929=CARTESIAN_POINT('Ctrl Pts',(82.7556945607658,126.135224741637,54.7991856778871));
#34930=CARTESIAN_POINT('Ctrl Pts',(82.9135843024676,126.206778482638,53.9077177001598));
#34931=CARTESIAN_POINT('Ctrl Pts',(82.9189338752071,126.278332223638,53.0184634379379));
#34932=CARTESIAN_POINT('Ctrl Pts',(82.9235377668022,127.721667776361,53.0258702510677));
#34933=CARTESIAN_POINT('Ctrl Pts',(82.9243763064541,127.707772857042,53.1981295493446));
#34934=CARTESIAN_POINT('Ctrl Pts',(82.9192431881647,127.693877937723,53.3703373531198));
#34935=CARTESIAN_POINT('Ctrl Pts',(82.9079775455321,127.679983018405,53.5421430349923));
#34936=CARTESIAN_POINT('Ctrl Pts',(82.7359669184006,127.467827008852,56.1653758187108));
#34937=CARTESIAN_POINT('Ctrl Pts',(81.1342793970736,127.2556709993,58.6948618252878));
#34938=CARTESIAN_POINT('Ctrl Pts',(78.8336056229594,127.043514989748,59.9679775697825));
#34939=CARTESIAN_POINT('Ctrl Pts',(76.5329318488456,126.831358980195,61.2410933142769));
#34940=CARTESIAN_POINT('Ctrl Pts',(73.5332718219452,126.619202970643,61.2578387966896));
#34941=CARTESIAN_POINT('Ctrl Pts',(71.2207350026679,126.407046961091,60.0109890899398));
#34942=CARTESIAN_POINT('Ctrl Pts',(68.9081981833903,126.194890951538,58.7641393831897));
#34943=CARTESIAN_POINT('Ctrl Pts',(67.2827845717363,125.982734941986,56.2536944872763));
#34944=CARTESIAN_POINT('Ctrl Pts',(67.0761308428276,125.770578932434,53.6308683128316));
#34945=CARTESIAN_POINT('Ctrl Pts',(66.9728039783733,125.664500927658,52.3194552256093));
#34946=CARTESIAN_POINT('Ctrl Pts',(67.2241670846051,125.558422922881,50.9799468187542));
#34947=CARTESIAN_POINT('Ctrl Pts',(67.7679802600526,125.452344918105,49.7721103797818));
#34948=CARTESIAN_POINT('Ctrl Pts',(68.3117934355002,125.346266913329,48.5642739408093));
#34949=CARTESIAN_POINT('Ctrl Pts',(69.1480566801635,125.240188908553,47.4881094697194));
#34950=CARTESIAN_POINT('Ctrl Pts',(70.1984110257089,125.134110903777,46.6961268467724));
#34951=CARTESIAN_POINT('Ctrl Pts',(72.2991197167995,124.921954894224,45.1121616008784));
#34952=CARTESIAN_POINT('Ctrl Pts',(75.2561928114182,124.709798884672,44.664923747555));
#34953=CARTESIAN_POINT('Ctrl Pts',(77.7227071033452,124.49764287512,45.5697817361127));
#34954=CARTESIAN_POINT('Ctrl Pts',(80.1892213952723,124.285486865568,46.4746397246703));
#34955=CARTESIAN_POINT('Ctrl Pts',(82.1651768845073,124.073330856015,48.7315935551091));
#34956=CARTESIAN_POINT('Ctrl Pts',(82.7371225012787,123.861174846463,51.2980700746261));
#34957=CARTESIAN_POINT('Ctrl Pts',(82.8624869401202,123.814672489762,51.8606146229795));
#34958=CARTESIAN_POINT('Ctrl Pts',(82.9203971144115,123.768170133062,52.4380298825457));
#34959=CARTESIAN_POINT('Ctrl Pts',(82.9149187311829,123.721667776361,53.016438653844));
#34960=CARTESIAN_POINT('Origin',(74.9879498948689,255.,53.0228109606356));
#34961=CARTESIAN_POINT('',(82.9120726157757,118.278332223638,53.026230598807));
#34962=CARTESIAN_POINT('',(82.9129498948689,119.721667776361,53.0228109606404));
#34963=CARTESIAN_POINT('',(82.9129498948689,255.,53.0228109606356));
#34964=CARTESIAN_POINT('Ctrl Pts',(82.9129498948689,118.278332223638,53.022810960627));
#34965=CARTESIAN_POINT('Ctrl Pts',(82.9129498948665,118.455428795637,50.8182135007173));
#34966=CARTESIAN_POINT('Ctrl Pts',(81.943279599106,118.632525367636,48.6308565362822));
#34967=CARTESIAN_POINT('Ctrl Pts',(80.3096882702482,118.809621939635,47.1504412801731));
#34968=CARTESIAN_POINT('Ctrl Pts',(78.6760969413904,118.986718511633,45.6700260240639));
#34969=CARTESIAN_POINT('Ctrl Pts',(76.4041347530365,119.163815083632,44.9197069006017));
#34970=CARTESIAN_POINT('Ctrl Pts',(74.2101800112143,119.340911655631,45.1360689838698));
#34971=CARTESIAN_POINT('Ctrl Pts',(72.0162252693922,119.518008227629,45.3524310671378));
#34972=CARTESIAN_POINT('Ctrl Pts',(69.9345925076919,119.695104799628,46.5320903475061));
#34973=CARTESIAN_POINT('Ctrl Pts',(68.6216467656565,119.872201371627,48.3030853894842));
#34974=CARTESIAN_POINT('Ctrl Pts',(67.308701023621,120.049297943626,50.0740804314624));
#34975=CARTESIAN_POINT('Ctrl Pts',(66.7849774198234,120.226394515624,52.4087119996478));
#34976=CARTESIAN_POINT('Ctrl Pts',(67.2156126057619,120.403491087623,54.5708413428815));
#34977=CARTESIAN_POINT('Ctrl Pts',(67.6462477917003,120.580587659622,56.7329706861151));
#34978=CARTESIAN_POINT('Ctrl Pts',(69.0245064208012,120.757684231621,58.6887810357277));
#34979=CARTESIAN_POINT('Ctrl Pts',(70.9158061804518,120.934780803619,59.821580744143));
#34980=CARTESIAN_POINT('Ctrl Pts',(72.8071059401024,121.111877375618,60.9543804525582));
#34981=CARTESIAN_POINT('Ctrl Pts',(75.1818659698161,121.288973947617,61.2464519739652));
#34982=CARTESIAN_POINT('Ctrl Pts',(77.2912945088721,121.466070519615,60.6057014773938));
#34983=CARTESIAN_POINT('Ctrl Pts',(79.400723047928,121.643167091614,59.9649509808225));
#34984=CARTESIAN_POINT('Ctrl Pts',(81.2118275942112,121.820263663613,58.4014001198733));
#34985=CARTESIAN_POINT('Ctrl Pts',(82.1535440633121,121.997360235612,56.4080561826501));
#34986=CARTESIAN_POINT('Ctrl Pts',(82.651569792993,122.091017564954,55.3538784110875));
#34987=CARTESIAN_POINT('Ctrl Pts',(82.9129498948701,122.184674894296,54.1887099277254));
#34988=CARTESIAN_POINT('Ctrl Pts',(82.9129498948689,122.278332223638,53.0228109606271));
#34989=CARTESIAN_POINT('Ctrl Pts',(82.9129498948689,123.721667776361,53.0228109606405));
#34990=CARTESIAN_POINT('Ctrl Pts',(82.9129498948675,123.544571204363,55.2274084205502));
#34991=CARTESIAN_POINT('Ctrl Pts',(81.9432795991081,123.367474632364,57.4147653849857));
#34992=CARTESIAN_POINT('Ctrl Pts',(80.3096882702509,123.190378060365,58.8951806410956));
#34993=CARTESIAN_POINT('Ctrl Pts',(78.6760969413938,123.013281488366,60.3755958972055));
#34994=CARTESIAN_POINT('Ctrl Pts',(76.4041347530403,122.836184916368,61.1259150206688));
#34995=CARTESIAN_POINT('Ctrl Pts',(74.210180011218,122.659088344369,60.9095529374017));
#34996=CARTESIAN_POINT('Ctrl Pts',(72.0162252693957,122.48199177237,60.6931908541347));
#34997=CARTESIAN_POINT('Ctrl Pts',(69.9345925076949,122.304895200372,59.5135315737674));
#34998=CARTESIAN_POINT('Ctrl Pts',(68.6216467656586,122.127798628373,57.7425365317898));
#34999=CARTESIAN_POINT('Ctrl Pts',(67.3087010236223,121.950702056374,55.9715414898123));
#35000=CARTESIAN_POINT('Ctrl Pts',(66.7849774198237,121.773605484375,53.6369099216271));
#35001=CARTESIAN_POINT('Ctrl Pts',(67.2156126057612,121.596508912377,51.4747805783933));
#35002=CARTESIAN_POINT('Ctrl Pts',(67.6462477916986,121.419412340378,49.3126512351594));
#35003=CARTESIAN_POINT('Ctrl Pts',(69.0245064207986,121.242315768379,47.3568408855462));
#35004=CARTESIAN_POINT('Ctrl Pts',(70.9158061804487,121.065219196381,46.22404117713));
#35005=CARTESIAN_POINT('Ctrl Pts',(72.8071059400988,120.888122624382,45.0912414687139));
#35006=CARTESIAN_POINT('Ctrl Pts',(75.1818659698123,120.711026052383,44.7991699473058));
#35007=CARTESIAN_POINT('Ctrl Pts',(77.2912945088686,120.533929480384,45.4399204438762));
#35008=CARTESIAN_POINT('Ctrl Pts',(79.4007230479249,120.356832908386,46.0806709404466));
#35009=CARTESIAN_POINT('Ctrl Pts',(81.2118275942088,120.179736336387,47.644221801395));
#35010=CARTESIAN_POINT('Ctrl Pts',(82.1535440633106,120.002639764388,49.6375657386177));
#35011=CARTESIAN_POINT('Ctrl Pts',(82.651569792992,119.908982435046,50.6917435101801));
#35012=CARTESIAN_POINT('Ctrl Pts',(82.9129498948696,119.815325105704,51.8569119935421));
#35013=CARTESIAN_POINT('Ctrl Pts',(82.9129498948689,119.721667776361,53.0228109606404));
#35014=CARTESIAN_POINT('Origin',(74.9879498948689,255.,53.0228109606356));
#35015=CARTESIAN_POINT('',(82.9265976773671,114.278332223639,53.0209215921915));
#35016=CARTESIAN_POINT('',(82.9129498948689,115.721667776361,53.0228109606402));
#35017=CARTESIAN_POINT('',(82.9129498948689,255.,53.0228109606356));
#35018=CARTESIAN_POINT('Ctrl Pts',(82.9265976773671,114.278332223639,53.0209215921915));
#35019=CARTESIAN_POINT('Ctrl Pts',(82.926669806443,114.28189230592,52.9767949794036));
#35020=CARTESIAN_POINT('Ctrl Pts',(82.9263402120587,114.285452388202,52.9326702304328));
#35021=CARTESIAN_POINT('Ctrl Pts',(82.9256058490196,114.289012470483,52.8885531439508));
#35022=CARTESIAN_POINT('Ctrl Pts',(82.881842947036,114.501168480036,50.259483285201));
#35023=CARTESIAN_POINT('Ctrl Pts',(81.4006143848999,114.713324489588,47.6576254258715));
#35024=CARTESIAN_POINT('Ctrl Pts',(79.1653127964464,114.92548049914,46.274019737072));
#35025=CARTESIAN_POINT('Ctrl Pts',(76.930011207993,115.137636508692,44.8904140482725));
#35026=CARTESIAN_POINT('Ctrl Pts',(73.9406365932216,115.349792518245,44.7250605300029));
#35027=CARTESIAN_POINT('Ctrl Pts',(71.5680013688734,115.561948527797,45.8584296693205));
#35028=CARTESIAN_POINT('Ctrl Pts',(69.1953661445251,115.774104537349,46.9917988086382));
#35029=CARTESIAN_POINT('Ctrl Pts',(67.4394703105995,115.986260546902,49.4238906055428));
#35030=CARTESIAN_POINT('Ctrl Pts',(67.1112761817494,116.198416556454,52.030564606166));
#35031=CARTESIAN_POINT('Ctrl Pts',(66.7830820528992,116.410572566006,54.6372386067891));
#35032=CARTESIAN_POINT('Ctrl Pts',(67.8825896291245,116.622728575559,57.4184948111306));
#35033=CARTESIAN_POINT('Ctrl Pts',(69.8976241478683,116.834884585111,59.1101090677785));
#35034=CARTESIAN_POINT('Ctrl Pts',(70.9051414072403,116.940962589887,59.9559161961026));
#35035=CARTESIAN_POINT('Ctrl Pts',(72.1415404022421,117.047040594663,60.5293128375032));
#35036=CARTESIAN_POINT('Ctrl Pts',(73.440615299286,117.153118599439,60.7881680962311));
#35037=CARTESIAN_POINT('Ctrl Pts',(74.7396901963296,117.259196604216,61.0470233549589));
#35038=CARTESIAN_POINT('Ctrl Pts',(76.1014409954152,117.365274608992,60.9913372310143));
#35039=CARTESIAN_POINT('Ctrl Pts',(77.3562073346029,117.471352613768,60.5963155097164));
#35040=CARTESIAN_POINT('Ctrl Pts',(79.8657400129785,117.68350862332,59.8062720671206));
#35041=CARTESIAN_POINT('Ctrl Pts',(81.9473348517627,117.895664632872,57.6588862351121));
#35042=CARTESIAN_POINT('Ctrl Pts',(82.643354326633,118.107820642425,55.125505564479));
#35043=CARTESIAN_POINT('Ctrl Pts',(82.8298199083623,118.164657836163,54.4468057327257));
#35044=CARTESIAN_POINT('Ctrl Pts',(82.9168400828375,118.221495029901,53.7404023094359));
#35045=CARTESIAN_POINT('Ctrl Pts',(82.9105319413203,118.278332223638,53.0322361553416));
#35046=CARTESIAN_POINT('Ctrl Pts',(82.9129498948689,119.721667776361,53.0228109606404));
#35047=CARTESIAN_POINT('Ctrl Pts',(82.9129498948676,119.544571204363,55.2274084205503));
#35048=CARTESIAN_POINT('Ctrl Pts',(81.9432795991079,119.367474632364,57.4147653849862));
#35049=CARTESIAN_POINT('Ctrl Pts',(80.3096882702504,119.190378060365,58.8951806410961));
#35050=CARTESIAN_POINT('Ctrl Pts',(78.6760969413929,119.013281488366,60.3755958972061));
#35051=CARTESIAN_POINT('Ctrl Pts',(76.4041347530389,118.836184916368,61.1259150206691));
#35052=CARTESIAN_POINT('Ctrl Pts',(74.2101800112163,118.659088344369,60.9095529374016));
#35053=CARTESIAN_POINT('Ctrl Pts',(72.0162252693938,118.48199177237,60.6931908541341));
#35054=CARTESIAN_POINT('Ctrl Pts',(69.934592507693,118.304895200371,59.513531573766));
#35055=CARTESIAN_POINT('Ctrl Pts',(68.6216467656571,118.127798628373,57.7425365317878));
#35056=CARTESIAN_POINT('Ctrl Pts',(67.3087010236212,117.950702056374,55.9715414898096));
#35057=CARTESIAN_POINT('Ctrl Pts',(66.7849774198234,117.773605484375,53.6369099216238));
#35058=CARTESIAN_POINT('Ctrl Pts',(67.2156126057618,117.596508912376,51.4747805783899));
#35059=CARTESIAN_POINT('Ctrl Pts',(67.6462477917003,117.419412340378,49.3126512351559));
#35060=CARTESIAN_POINT('Ctrl Pts',(69.0245064208014,117.242315768379,47.3568408855431));
#35061=CARTESIAN_POINT('Ctrl Pts',(70.9158061804524,117.06521919638,46.2240411771278));
#35062=CARTESIAN_POINT('Ctrl Pts',(72.8071059401034,116.888122624381,45.0912414687125));
#35063=CARTESIAN_POINT('Ctrl Pts',(75.1818659698175,116.711026052383,44.7991699473059));
#35064=CARTESIAN_POINT('Ctrl Pts',(77.2912945088736,116.533929480384,45.4399204438778));
#35065=CARTESIAN_POINT('Ctrl Pts',(79.4007230479297,116.356832908385,46.0806709404496));
#35066=CARTESIAN_POINT('Ctrl Pts',(81.2118275942128,116.179736336386,47.6442218013996));
#35067=CARTESIAN_POINT('Ctrl Pts',(82.1535440633132,116.002639764388,49.6375657386233));
#35068=CARTESIAN_POINT('Ctrl Pts',(82.6515697929929,115.908982435046,50.6917435101841));
#35069=CARTESIAN_POINT('Ctrl Pts',(82.9129498948696,115.815325105703,51.856911993544));
#35070=CARTESIAN_POINT('Ctrl Pts',(82.9129498948689,115.721667776361,53.0228109606402));
#35071=CARTESIAN_POINT('Origin',(74.9879498948689,255.,53.0228109606356));
#35072=CARTESIAN_POINT('',(82.9072283316561,110.278332223639,53.0161030812075));
#35073=CARTESIAN_POINT('',(82.914162998225,111.721667776361,53.022195355026));
#35074=CARTESIAN_POINT('',(82.9129498948689,255.,53.0228109606356));
#35075=CARTESIAN_POINT('Ctrl Pts',(82.9072283316561,110.278332223639,53.0161030812075));
#35076=CARTESIAN_POINT('Ctrl Pts',(82.91339009057,110.34228958194,52.2189267668967));
#35077=CARTESIAN_POINT('Ctrl Pts',(82.8024737341836,110.406246940241,51.4234892477125));
#35078=CARTESIAN_POINT('Ctrl Pts',(82.5672179608654,110.470204298542,50.666704134855));
#35079=CARTESIAN_POINT('Ctrl Pts',(81.7868397930174,110.682360308094,48.1563360724852));
#35080=CARTESIAN_POINT('Ctrl Pts',(79.6382966506498,110.894516317646,46.0712785819531));
#35081=CARTESIAN_POINT('Ctrl Pts',(77.1037815994124,111.106672327198,45.3711664703411));
#35082=CARTESIAN_POINT('Ctrl Pts',(74.5692665481747,111.318828336751,44.671054358729));
#35083=CARTESIAN_POINT('Ctrl Pts',(71.6487795880667,111.530984346303,45.3558876260377));
#35084=CARTESIAN_POINT('Ctrl Pts',(69.6917252898121,111.743140355855,47.1087136885494));
#35085=CARTESIAN_POINT('Ctrl Pts',(67.7346709915576,111.955296365408,48.8615397510611));
#35086=CARTESIAN_POINT('Ctrl Pts',(66.741049355156,112.16745237496,51.682358608776));
#35087=CARTESIAN_POINT('Ctrl Pts',(67.1531566815994,112.379608384512,54.2808370975297));
#35088=CARTESIAN_POINT('Ctrl Pts',(67.3592103448211,112.485686389289,55.5800763419067));
#35089=CARTESIAN_POINT('Ctrl Pts',(67.9166962487536,112.591764394065,56.8237304940425));
#35090=CARTESIAN_POINT('Ctrl Pts',(68.7277558216382,112.697842398841,57.8710050532353));
#35091=CARTESIAN_POINT('Ctrl Pts',(69.5388153945226,112.803920403617,58.918279612428));
#35092=CARTESIAN_POINT('Ctrl Pts',(70.6034486363594,112.909998408393,59.7691745786775));
#35093=CARTESIAN_POINT('Ctrl Pts',(71.8098206718925,113.016076413169,60.2937193700344));
#35094=CARTESIAN_POINT('Ctrl Pts',(74.2225647429588,113.228232422722,61.3428089527482));
#35095=CARTESIAN_POINT('Ctrl Pts',(77.2022639888126,113.440388432274,61.0864978358941));
#35096=CARTESIAN_POINT('Ctrl Pts',(79.3889649908238,113.652544441826,59.6302013483819));
#35097=CARTESIAN_POINT('Ctrl Pts',(81.5389720735405,113.861140369097,58.1983422328436));
#35098=CARTESIAN_POINT('Ctrl Pts',(82.9223714178924,114.069736296368,55.6064325393708));
#35099=CARTESIAN_POINT('Ctrl Pts',(82.9265976773671,114.278332223639,53.0209215921915));
#35100=CARTESIAN_POINT('Ctrl Pts',(82.9129498948689,115.721667776361,53.0228109606402));
#35101=CARTESIAN_POINT('Ctrl Pts',(82.9129498948676,115.544571204363,55.2274084205502));
#35102=CARTESIAN_POINT('Ctrl Pts',(81.943279599108,115.367474632364,57.414765384986));
#35103=CARTESIAN_POINT('Ctrl Pts',(80.3096882702505,115.190378060365,58.895180641096));
#35104=CARTESIAN_POINT('Ctrl Pts',(78.676096941393,115.013281488366,60.375595897206));
#35105=CARTESIAN_POINT('Ctrl Pts',(76.4041347530391,114.836184916368,61.125915020669));
#35106=CARTESIAN_POINT('Ctrl Pts',(74.2101800112165,114.659088344369,60.9095529374016));
#35107=CARTESIAN_POINT('Ctrl Pts',(72.0162252693939,114.48199177237,60.6931908541341));
#35108=CARTESIAN_POINT('Ctrl Pts',(69.9345925076931,114.304895200371,59.5135315737661));
#35109=CARTESIAN_POINT('Ctrl Pts',(68.6216467656572,114.127798628373,57.7425365317879));
#35110=CARTESIAN_POINT('Ctrl Pts',(67.3087010236213,113.950702056374,55.9715414898098));
#35111=CARTESIAN_POINT('Ctrl Pts',(66.7849774198234,113.773605484375,53.636909921624));
#35112=CARTESIAN_POINT('Ctrl Pts',(67.2156126057618,113.596508912376,51.47478057839));
#35113=CARTESIAN_POINT('Ctrl Pts',(67.6462477917002,113.419412340378,49.3126512351561));
#35114=CARTESIAN_POINT('Ctrl Pts',(69.0245064208013,113.242315768379,47.3568408855432));
#35115=CARTESIAN_POINT('Ctrl Pts',(70.9158061804523,113.06521919638,46.2240411771279));
#35116=CARTESIAN_POINT('Ctrl Pts',(72.8071059401032,112.888122624381,45.0912414687126));
#35117=CARTESIAN_POINT('Ctrl Pts',(75.1818659698173,112.711026052383,44.7991699473059));
#35118=CARTESIAN_POINT('Ctrl Pts',(77.2912945088734,112.533929480384,45.4399204438777));
#35119=CARTESIAN_POINT('Ctrl Pts',(79.4007230479296,112.356832908385,46.0806709404495));
#35120=CARTESIAN_POINT('Ctrl Pts',(81.2118275942127,112.179736336386,47.6442218013994));
#35121=CARTESIAN_POINT('Ctrl Pts',(82.1535440633131,112.002639764388,49.6375657386231));
#35122=CARTESIAN_POINT('Ctrl Pts',(82.6515697929928,111.908982435046,50.691743510184));
#35123=CARTESIAN_POINT('Ctrl Pts',(82.9129498948696,111.815325105703,51.8569119935438));
#35124=CARTESIAN_POINT('Ctrl Pts',(82.9129498948689,111.721667776361,53.02281096064));
#35125=CARTESIAN_POINT('Origin',(74.9879498948689,255.,53.0228109606356));
#35126=CARTESIAN_POINT('',(82.9013905598197,106.278332223639,53.0264432070762));
#35127=CARTESIAN_POINT('',(82.9112471737191,107.721667776361,53.0211761040089));
#35128=CARTESIAN_POINT('',(82.9129498948689,255.,53.0228109606356));
#35129=CARTESIAN_POINT('Ctrl Pts',(82.9013905598197,106.278332223639,53.0264432070762));
#35130=CARTESIAN_POINT('Ctrl Pts',(82.8957299962823,106.402686857959,51.473491209011));
#35131=CARTESIAN_POINT('Ctrl Pts',(82.4553262468078,106.527041492279,49.9172246269154));
#35132=CARTESIAN_POINT('Ctrl Pts',(81.602793261273,106.6513961266,48.633248972721));
#35133=CARTESIAN_POINT('Ctrl Pts',(80.148323975016,106.863552136152,46.4427141957518));
#35134=CARTESIAN_POINT('Ctrl Pts',(77.4942997286751,107.075708145705,45.0447170612752));
#35135=CARTESIAN_POINT('Ctrl Pts',(74.8673520726336,107.287864155257,45.0848012745632));
#35136=CARTESIAN_POINT('Ctrl Pts',(72.2404044165922,107.500020164809,45.1248854878513));
#35137=CARTESIAN_POINT('Ctrl Pts',(69.6405333508502,107.712176174362,46.6030510489039));
#35138=CARTESIAN_POINT('Ctrl Pts',(68.2477787460151,107.924332183914,48.8351257599594));
#35139=CARTESIAN_POINT('Ctrl Pts',(67.5514014435974,108.03041018869,49.9511631154873));
#35140=CARTESIAN_POINT('Ctrl Pts',(67.1568032564067,108.136488193466,51.2556777585156));
#35141=CARTESIAN_POINT('Ctrl Pts',(67.0824240849773,108.242566198242,52.5782016229346));
#35142=CARTESIAN_POINT('Ctrl Pts',(67.008044913548,108.348644203018,53.9007254873536));
#35143=CARTESIAN_POINT('Ctrl Pts',(67.2538847578803,108.454722207795,55.2412585731629));
#35144=CARTESIAN_POINT('Ctrl Pts',(67.8207339014658,108.560800212571,56.4283401940603));
#35145=CARTESIAN_POINT('Ctrl Pts',(68.9544321886369,108.772956222123,58.8025034358548));
#35146=CARTESIAN_POINT('Ctrl Pts',(71.3721676728211,108.985112231675,60.5628608180023));
#35147=CARTESIAN_POINT('Ctrl Pts',(73.9780553079737,109.197268241228,60.8972413866579));
#35148=CARTESIAN_POINT('Ctrl Pts',(76.5839429431266,109.40942425078,61.2316219553135));
#35149=CARTESIAN_POINT('Ctrl Pts',(79.3779827292481,109.621580260332,60.140025710477));
#35150=CARTESIAN_POINT('Ctrl Pts',(81.0688960256448,109.833736269885,58.1263882709549));
#35151=CARTESIAN_POINT('Ctrl Pts',(82.2500601625347,109.981934921136,56.7197896397118));
#35152=CARTESIAN_POINT('Ctrl Pts',(82.8929506256246,110.130133572387,54.8632784137831));
#35153=CARTESIAN_POINT('Ctrl Pts',(82.9072283316561,110.278332223639,53.0161030812075));
#35154=CARTESIAN_POINT('Ctrl Pts',(82.9203893972147,111.721667776361,53.0190356850543));
#35155=CARTESIAN_POINT('Ctrl Pts',(82.9044169888665,111.525049942016,55.4585889787224));
#35156=CARTESIAN_POINT('Ctrl Pts',(81.7038364465635,111.32843210767,57.9063818370155));
#35157=CARTESIAN_POINT('Ctrl Pts',(79.7574894659549,111.131814273324,59.369308726392));
#35158=CARTESIAN_POINT('Ctrl Pts',(77.6573279522039,110.919658263772,60.9478467677124));
#35159=CARTESIAN_POINT('Ctrl Pts',(74.6888706496056,110.707502254219,61.3797054608276));
#35160=CARTESIAN_POINT('Ctrl Pts',(72.2237319036017,110.495346244667,60.4648205081005));
#35161=CARTESIAN_POINT('Ctrl Pts',(69.7585931575979,110.283190235115,59.5499355553734));
#35162=CARTESIAN_POINT('Ctrl Pts',(67.7967729681888,110.071034225562,57.2883069568041));
#35163=CARTESIAN_POINT('Ctrl Pts',(67.2345508544968,109.85887821601,54.7202640856088));
#35164=CARTESIAN_POINT('Ctrl Pts',(66.6723287408047,109.646722206458,52.1522212144135));
#35165=CARTESIAN_POINT('Ctrl Pts',(67.5097047028302,109.434566196906,49.277764070592));
#35166=CARTESIAN_POINT('Ctrl Pts',(69.3670720102395,109.222410187353,47.4165520463605));
#35167=CARTESIAN_POINT('Ctrl Pts',(71.2244393176486,109.010254177801,45.5553400221291));
#35168=CARTESIAN_POINT('Ctrl Pts',(74.1017979704413,108.798098168248,44.7073731174872));
#35169=CARTESIAN_POINT('Ctrl Pts',(76.6694103498548,108.585942158696,45.2639945335493));
#35170=CARTESIAN_POINT('Ctrl Pts',(79.2370227292686,108.373786149144,45.8206159496114));
#35171=CARTESIAN_POINT('Ctrl Pts',(81.494888835303,108.161630139592,47.7818256863778));
#35172=CARTESIAN_POINT('Ctrl Pts',(82.4208099654913,107.949474130039,50.2444651170894));
#35173=CARTESIAN_POINT('Ctrl Pts',(82.7522181540638,107.873538678813,51.1258996650548));
#35174=CARTESIAN_POINT('Ctrl Pts',(82.9129926600863,107.797603227587,52.0715716978783));
#35175=CARTESIAN_POINT('Ctrl Pts',(82.9088160628959,107.721667776361,53.0188418887739));
#35176=CARTESIAN_POINT('Origin',(74.9879498948689,255.,53.0228109606356));
#35177=CARTESIAN_POINT('',(82.9152391029311,102.278332223638,53.0245422282611));
#35178=CARTESIAN_POINT('',(82.9071031787868,103.721667776361,53.0246287521325));
#35179=CARTESIAN_POINT('',(82.9129498948689,255.,53.0228109606356));
#35180=CARTESIAN_POINT('Ctrl Pts',(82.9213199937229,102.278332223639,53.0291410455188));
#35181=CARTESIAN_POINT('Ctrl Pts',(82.9025444830628,102.463084133978,50.7348024945283));
#35182=CARTESIAN_POINT('Ctrl Pts',(81.852113259209,102.647836044318,48.4242605728558));
#35183=CARTESIAN_POINT('Ctrl Pts',(80.1020724172332,102.832587954658,46.9505550011793));
#35184=CARTESIAN_POINT('Ctrl Pts',(78.092449453638,103.044743964211,45.258255891705));
#35185=CARTESIAN_POINT('Ctrl Pts',(75.1602793383455,103.256899973763,44.6694593229734));
#35186=CARTESIAN_POINT('Ctrl Pts',(72.6451198214141,103.469055983315,45.4414020082891));
#35187=CARTESIAN_POINT('Ctrl Pts',(71.3875400629484,103.575133988091,45.827373350947));
#35188=CARTESIAN_POINT('Ctrl Pts',(70.2342129540729,103.681211992867,46.5535295071167));
#35189=CARTESIAN_POINT('Ctrl Pts',(69.3108412201961,103.787289997644,47.5032590866166));
#35190=CARTESIAN_POINT('Ctrl Pts',(68.3874694863192,103.89336800242,48.4529886661165));
#35191=CARTESIAN_POINT('Ctrl Pts',(67.694053127441,103.999446007196,49.6262916689466));
#35192=CARTESIAN_POINT('Ctrl Pts',(67.3436203427675,104.105524011972,50.8942339348569));
#35193=CARTESIAN_POINT('Ctrl Pts',(66.6427547734206,104.317680021524,53.4301184666777));
#35194=CARTESIAN_POINT('Ctrl Pts',(67.313823500893,104.529836031077,56.3445600508194));
#35195=CARTESIAN_POINT('Ctrl Pts',(69.0619992390115,104.741992040629,58.3057694533032));
#35196=CARTESIAN_POINT('Ctrl Pts',(70.8101749771299,104.954148050181,60.2669788557869));
#35197=CARTESIAN_POINT('Ctrl Pts',(73.6354577258942,105.166304059734,61.2749560766129));
#35198=CARTESIAN_POINT('Ctrl Pts',(76.2324908878125,105.378460069286,60.8634439022218));
#35199=CARTESIAN_POINT('Ctrl Pts',(78.8295240497311,105.590616078838,60.4519317278306));
#35200=CARTESIAN_POINT('Ctrl Pts',(81.1983076248037,105.802772088391,58.6209301582221));
#35201=CARTESIAN_POINT('Ctrl Pts',(82.2552422492533,106.014928097943,56.2138931636867));
#35202=CARTESIAN_POINT('Ctrl Pts',(82.6926576859061,106.102729473175,55.2177339749835));
#35203=CARTESIAN_POINT('Ctrl Pts',(82.9053872364686,106.190530848407,54.1229147768275));
#35204=CARTESIAN_POINT('Ctrl Pts',(82.9013905598197,106.278332223639,53.0264432070762));
#35205=CARTESIAN_POINT('Ctrl Pts',(82.9129498948689,107.721667776361,53.0228109606394));
#35206=CARTESIAN_POINT('Ctrl Pts',(82.9129498948679,107.544571204363,55.2274084205489));
#35207=CARTESIAN_POINT('Ctrl Pts',(81.9432795991088,107.367474632364,57.4147653849844));
#35208=CARTESIAN_POINT('Ctrl Pts',(80.3096882702521,107.190378060365,58.8951806410946));
#35209=CARTESIAN_POINT('Ctrl Pts',(78.6760969413954,107.013281488367,60.3755958972047));
#35210=CARTESIAN_POINT('Ctrl Pts',(76.4041347530422,106.836184916368,61.1259150206684));
#35211=CARTESIAN_POINT('Ctrl Pts',(74.21018001122,106.659088344369,60.9095529374019));
#35212=CARTESIAN_POINT('Ctrl Pts',(72.0162252693978,106.48199177237,60.6931908541355));
#35213=CARTESIAN_POINT('Ctrl Pts',(69.9345925076968,106.304895200372,59.5135315737688));
#35214=CARTESIAN_POINT('Ctrl Pts',(68.6216467656601,106.127798628373,57.7425365317918));
#35215=CARTESIAN_POINT('Ctrl Pts',(67.3087010236234,105.950702056374,55.9715414898148));
#35216=CARTESIAN_POINT('Ctrl Pts',(66.784977419824,105.773605484376,53.63690992163));
#35217=CARTESIAN_POINT('Ctrl Pts',(67.2156126057606,105.596508912377,51.4747805783961));
#35218=CARTESIAN_POINT('Ctrl Pts',(67.6462477916972,105.419412340378,49.3126512351623));
#35219=CARTESIAN_POINT('Ctrl Pts',(69.0245064207963,105.242315768379,47.3568408855486));
#35220=CARTESIAN_POINT('Ctrl Pts',(70.9158061804458,105.065219196381,46.2240411771318));
#35221=CARTESIAN_POINT('Ctrl Pts',(72.8071059400953,104.888122624382,45.0912414687149));
#35222=CARTESIAN_POINT('Ctrl Pts',(75.1818659698085,104.711026052383,44.7991699473058));
#35223=CARTESIAN_POINT('Ctrl Pts',(77.2912945088649,104.533929480385,45.4399204438751));
#35224=CARTESIAN_POINT('Ctrl Pts',(79.4007230479214,104.356832908386,46.0806709404444));
#35225=CARTESIAN_POINT('Ctrl Pts',(81.2118275942059,104.179736336387,47.6442218013918));
#35226=CARTESIAN_POINT('Ctrl Pts',(82.1535440633088,104.002639764389,49.6375657386139));
#35227=CARTESIAN_POINT('Ctrl Pts',(82.6515697929912,103.908982435046,50.691743510177));
#35228=CARTESIAN_POINT('Ctrl Pts',(82.9129498948695,103.815325105704,51.8569119935402));
#35229=CARTESIAN_POINT('Ctrl Pts',(82.9129498948689,103.721667776361,53.0228109606397));
#35230=CARTESIAN_POINT('Origin',(74.9879498948689,255.,53.0228109606356));
#35231=CARTESIAN_POINT('',(82.9148571242665,98.2783322236385,53.0204066145287));
#35232=CARTESIAN_POINT('',(82.9174705652005,99.7216677763613,53.0248696685428));
#35233=CARTESIAN_POINT('',(82.9129498948689,255.,53.0228109606356));
#35234=CARTESIAN_POINT('Ctrl Pts',(82.9129498948689,98.2783322236385,53.0228109606261));
#35235=CARTESIAN_POINT('Ctrl Pts',(82.9129498948663,98.4554287956372,50.8182135007165));
#35236=CARTESIAN_POINT('Ctrl Pts',(81.9432795991056,98.632525367636,48.6308565362815));
#35237=CARTESIAN_POINT('Ctrl Pts',(80.3096882702476,98.8096219396347,47.1504412801725));
#35238=CARTESIAN_POINT('Ctrl Pts',(78.6760969413896,98.9867185116334,45.6700260240635));
#35239=CARTESIAN_POINT('Ctrl Pts',(76.4041347530357,99.1638150836321,44.9197069006016));
#35240=CARTESIAN_POINT('Ctrl Pts',(74.2101800112135,99.3409116556309,45.1360689838698));
#35241=CARTESIAN_POINT('Ctrl Pts',(72.0162252693913,99.5180082276296,45.3524310671381));
#35242=CARTESIAN_POINT('Ctrl Pts',(69.9345925076912,99.6951047996283,46.5320903475066));
#35243=CARTESIAN_POINT('Ctrl Pts',(68.621646765656,99.872201371627,48.3030853894849));
#35244=CARTESIAN_POINT('Ctrl Pts',(67.3087010236207,100.049297943626,50.0740804314632));
#35245=CARTESIAN_POINT('Ctrl Pts',(66.7849774198233,100.226394515624,52.4087119996487));
#35246=CARTESIAN_POINT('Ctrl Pts',(67.215612605762,100.403491087623,54.5708413428823));
#35247=CARTESIAN_POINT('Ctrl Pts',(67.6462477917007,100.580587659622,56.7329706861159));
#35248=CARTESIAN_POINT('Ctrl Pts',(69.0245064208018,100.757684231621,58.6887810357283));
#35249=CARTESIAN_POINT('Ctrl Pts',(70.9158061804525,100.934780803619,59.8215807441434));
#35250=CARTESIAN_POINT('Ctrl Pts',(72.8071059401033,101.111877375618,60.9543804525585));
#35251=CARTESIAN_POINT('Ctrl Pts',(75.181865969817,101.288973947617,61.2464519739652));
#35252=CARTESIAN_POINT('Ctrl Pts',(77.2912945088729,101.466070519615,60.6057014773936));
#35253=CARTESIAN_POINT('Ctrl Pts',(79.4007230479288,101.643167091614,59.964950980822));
#35254=CARTESIAN_POINT('Ctrl Pts',(81.2118275942118,101.820263663613,58.4014001198726));
#35255=CARTESIAN_POINT('Ctrl Pts',(82.1535440633125,101.997360235612,56.4080561826493));
#35256=CARTESIAN_POINT('Ctrl Pts',(82.6515697929932,102.091017564954,55.3538784110869));
#35257=CARTESIAN_POINT('Ctrl Pts',(82.9129498948702,102.184674894296,54.1887099277249));
#35258=CARTESIAN_POINT('Ctrl Pts',(82.9129498948689,102.278332223638,53.0228109606267));
#35259=CARTESIAN_POINT('Ctrl Pts',(82.9002911396369,103.721667776361,53.0267466703926));
#35260=CARTESIAN_POINT('Ctrl Pts',(82.9057021213605,103.645844494054,53.9729164059735));
#35261=CARTESIAN_POINT('Ctrl Pts',(82.7488630974118,103.570021211748,54.9176096992055));
#35262=CARTESIAN_POINT('Ctrl Pts',(82.4215784532667,103.494197929441,55.7991000146744));
#35263=CARTESIAN_POINT('Ctrl Pts',(81.9637019147087,103.388119924664,57.0323192983762));
#35264=CARTESIAN_POINT('Ctrl Pts',(81.1722212836696,103.282041919888,58.1418347754652));
#35265=CARTESIAN_POINT('Ctrl Pts',(80.1708053598078,103.175963915112,59.0088802071099));
#35266=CARTESIAN_POINT('Ctrl Pts',(79.169389435946,103.069885910336,59.8759256387545));
#35267=CARTESIAN_POINT('Ctrl Pts',(77.9580382192615,102.96380790556,60.5005010249548));
#35268=CARTESIAN_POINT('Ctrl Pts',(76.6719915821466,102.857729900784,60.7772044282973));
#35269=CARTESIAN_POINT('Ctrl Pts',(74.0998983079167,102.645573891231,61.3306112349823));
#35270=CARTESIAN_POINT('Ctrl Pts',(71.2290233519653,102.433417881679,60.4925301102361));
#35271=CARTESIAN_POINT('Ctrl Pts',(69.3719298576632,102.221261872127,58.6341263636949));
#35272=CARTESIAN_POINT('Ctrl Pts',(67.5148363633613,102.009105862574,56.7757226171537));
#35273=CARTESIAN_POINT('Ctrl Pts',(66.6715243307089,101.796949853022,53.8969962488175));
#35274=CARTESIAN_POINT('Ctrl Pts',(67.2321703217131,101.58479384347,51.328027664629));
#35275=CARTESIAN_POINT('Ctrl Pts',(67.7928163127172,101.372637833918,48.7590590804408));
#35276=CARTESIAN_POINT('Ctrl Pts',(69.7574203273777,101.160481824365,46.4998482804));
#35277=CARTESIAN_POINT('Ctrl Pts',(72.2214217592123,100.948325814813,45.5835323756284));
#35278=CARTESIAN_POINT('Ctrl Pts',(74.6854231910471,100.736169805261,44.6672164708568));
#35279=CARTESIAN_POINT('Ctrl Pts',(77.6488220400558,100.524013795708,45.0937954613543));
#35280=CARTESIAN_POINT('Ctrl Pts',(79.7518025028245,100.311857786156,46.6722113403257));
#35281=CARTESIAN_POINT('Ctrl Pts',(81.7018738403247,100.115127782891,48.1358595380769));
#35282=CARTESIAN_POINT('Ctrl Pts',(82.9121010957909,99.9183977796261,50.5899325326873));
#35283=CARTESIAN_POINT('Ctrl Pts',(82.9250431686022,99.7216677763613,53.0283182231438));
#35284=CARTESIAN_POINT('Origin',(74.9879498948689,255.,53.0228109606356));
#35285=CARTESIAN_POINT('',(82.9078887632605,94.2783322236386,53.0225290086082));
#35286=CARTESIAN_POINT('',(82.9129498948689,95.7216677763614,53.0228109606393));
#35287=CARTESIAN_POINT('',(82.9129498948689,255.,53.0228109606356));
#35288=CARTESIAN_POINT('Ctrl Pts',(82.8975201390833,94.2783322236385,53.0219513800174));
#35289=CARTESIAN_POINT('Ctrl Pts',(82.8998090143212,94.371722676465,51.8556225753435));
#35290=CARTESIAN_POINT('Ctrl Pts',(82.658061451432,94.4651131292914,50.6900196140694));
#35291=CARTESIAN_POINT('Ctrl Pts',(82.1665533003896,94.5585035821179,49.6413515712521));
#35292=CARTESIAN_POINT('Ctrl Pts',(81.608271351691,94.6645815868941,48.4502168215223));
#35293=CARTESIAN_POINT('Ctrl Pts',(80.7277566876189,94.7706595916702,47.409947572931));
#35294=CARTESIAN_POINT('Ctrl Pts',(79.6580752337028,94.8767375964464,46.6286773122345));
#35295=CARTESIAN_POINT('Ctrl Pts',(78.588393779787,94.9828156012226,45.8474070515383));
#35296=CARTESIAN_POINT('Ctrl Pts',(77.3295455360272,95.0888936059988,45.3251357787369));
#35297=CARTESIAN_POINT('Ctrl Pts',(76.025022796263,95.194971610775,45.1557216479993));
#35298=CARTESIAN_POINT('Ctrl Pts',(73.4159773167343,95.4071276203273,44.8168933865239));
#35299=CARTESIAN_POINT('Ctrl Pts',(70.6242338531869,95.6192836298796,45.8894936933033));
#35300=CARTESIAN_POINT('Ctrl Pts',(68.9271693444514,95.8314396394319,47.8950940485404));
#35301=CARTESIAN_POINT('Ctrl Pts',(67.2301048357161,96.0435956489842,49.9006944037773));
#35302=CARTESIAN_POINT('Ctrl Pts',(66.6277192817928,96.2557516585364,52.839294807472));
#35303=CARTESIAN_POINT('Ctrl Pts',(67.398870273312,96.4679076680887,55.353106586833));
#35304=CARTESIAN_POINT('Ctrl Pts',(68.1700212648314,96.6800636776411,57.8669183661945));
#35305=CARTESIAN_POINT('Ctrl Pts',(70.3147088017936,96.8922196871935,59.9559415212221));
#35306=CARTESIAN_POINT('Ctrl Pts',(72.8460411335263,97.1043756967458,60.6653740548343));
#35307=CARTESIAN_POINT('Ctrl Pts',(75.3773734652585,97.3165317062981,61.3748065884463));
#35308=CARTESIAN_POINT('Ctrl Pts',(78.2953505917612,97.5286877158503,60.7046485006431));
#35309=CARTESIAN_POINT('Ctrl Pts',(80.2606118745933,97.7408437254026,58.9577450677149));
#35310=CARTESIAN_POINT('Ctrl Pts',(81.9202480039677,97.9200065581479,57.4825091399822));
#35311=CARTESIAN_POINT('Ctrl Pts',(82.9004481365671,98.0991693908933,55.2393847052011));
#35312=CARTESIAN_POINT('Ctrl Pts',(82.9197187285079,98.2783322236386,53.0142778398783));
#35313=CARTESIAN_POINT('Ctrl Pts',(82.9129498948689,99.7216677763614,53.0228109606395));
#35314=CARTESIAN_POINT('Ctrl Pts',(82.9129498948678,99.5445712043626,55.2274084205496));
#35315=CARTESIAN_POINT('Ctrl Pts',(81.9432795991082,99.3674746323639,57.4147653849857));
#35316=CARTESIAN_POINT('Ctrl Pts',(80.3096882702507,99.1903780603651,58.8951806410958));
#35317=CARTESIAN_POINT('Ctrl Pts',(78.6760969413931,99.0132814883663,60.375595897206));
#35318=CARTESIAN_POINT('Ctrl Pts',(76.404134753039,98.8361849163676,61.1259150206691));
#35319=CARTESIAN_POINT('Ctrl Pts',(74.2101800112163,98.6590883443688,60.9095529374016));
#35320=CARTESIAN_POINT('Ctrl Pts',(72.0162252693936,98.4819917723701,60.693190854134));
#35321=CARTESIAN_POINT('Ctrl Pts',(69.9345925076927,98.3048952003713,59.5135315737658));
#35322=CARTESIAN_POINT('Ctrl Pts',(68.6216467656568,98.1277986283726,57.7425365317874));
#35323=CARTESIAN_POINT('Ctrl Pts',(67.308701023621,97.9507020563738,55.971541489809));
#35324=CARTESIAN_POINT('Ctrl Pts',(66.7849774198233,97.7736054843751,53.636909921623));
#35325=CARTESIAN_POINT('Ctrl Pts',(67.215612605762,97.5965089123763,51.474780578389));
#35326=CARTESIAN_POINT('Ctrl Pts',(67.6462477917008,97.4194123403775,49.3126512351549));
#35327=CARTESIAN_POINT('Ctrl Pts',(69.0245064208023,97.2423157683788,47.3568408855421));
#35328=CARTESIAN_POINT('Ctrl Pts',(70.9158061804536,97.06521919638,46.2240411771271));
#35329=CARTESIAN_POINT('Ctrl Pts',(72.8071059401049,96.8881226243813,45.0912414687121));
#35330=CARTESIAN_POINT('Ctrl Pts',(75.1818659698193,96.7110260523825,44.7991699473059));
#35331=CARTESIAN_POINT('Ctrl Pts',(77.2912945088754,96.5339294803838,45.4399204438783));
#35332=CARTESIAN_POINT('Ctrl Pts',(79.4007230479315,96.356832908385,46.0806709404507));
#35333=CARTESIAN_POINT('Ctrl Pts',(81.2118275942143,96.1797363363863,47.6442218014012));
#35334=CARTESIAN_POINT('Ctrl Pts',(82.1535440633142,96.0026397643875,49.6375657386254));
#35335=CARTESIAN_POINT('Ctrl Pts',(82.651569792993,95.9089824350455,50.6917435101853));
#35336=CARTESIAN_POINT('Ctrl Pts',(82.9129498948694,95.8153251057034,51.8569119935439));
#35337=CARTESIAN_POINT('Ctrl Pts',(82.9129498948689,95.7216677763614,53.0228109606389));
#35338=CARTESIAN_POINT('Origin',(74.9879498948689,255.,53.0228109606356));
#35339=CARTESIAN_POINT('',(82.9129498948689,90.2783322236385,53.0228109606262));
#35340=CARTESIAN_POINT('',(82.906851181591,91.7216677763616,53.0226606669491));
#35341=CARTESIAN_POINT('',(82.9129498948689,255.,53.0228109606356));
#35342=CARTESIAN_POINT('Ctrl Pts',(82.9129498948689,90.2783322236385,53.0228109606262));
#35343=CARTESIAN_POINT('Ctrl Pts',(82.9129498948663,90.4554287956373,50.8182135007164));
#35344=CARTESIAN_POINT('Ctrl Pts',(81.9432795991055,90.632525367636,48.6308565362813));
#35345=CARTESIAN_POINT('Ctrl Pts',(80.3096882702473,90.8096219396347,47.1504412801723));
#35346=CARTESIAN_POINT('Ctrl Pts',(78.6760969413892,90.9867185116335,45.6700260240633));
#35347=CARTESIAN_POINT('Ctrl Pts',(76.404134753035,91.1638150836322,44.9197069006014));
#35348=CARTESIAN_POINT('Ctrl Pts',(74.2101800112127,91.3409116556309,45.1360689838699));
#35349=CARTESIAN_POINT('Ctrl Pts',(72.0162252693904,91.5180082276297,45.3524310671384));
#35350=CARTESIAN_POINT('Ctrl Pts',(69.9345925076903,91.6951047996284,46.5320903475073));
#35351=CARTESIAN_POINT('Ctrl Pts',(68.6216467656552,91.8722013716271,48.3030853894859));
#35352=CARTESIAN_POINT('Ctrl Pts',(67.3087010236201,92.0492979436258,50.0740804314645));
#35353=CARTESIAN_POINT('Ctrl Pts',(66.7849774198232,92.2263945156246,52.4087119996503));
#35354=CARTESIAN_POINT('Ctrl Pts',(67.2156126057624,92.4034910876233,54.5708413428839));
#35355=CARTESIAN_POINT('Ctrl Pts',(67.6462477917016,92.580587659622,56.7329706861176));
#35356=CARTESIAN_POINT('Ctrl Pts',(69.0245064208032,92.7576842316208,58.6887810357299));
#35357=CARTESIAN_POINT('Ctrl Pts',(70.9158061804544,92.9347808036195,59.8215807441445));
#35358=CARTESIAN_POINT('Ctrl Pts',(72.8071059401056,93.1118773756182,60.9543804525592));
#35359=CARTESIAN_POINT('Ctrl Pts',(75.1818659698196,93.288973947617,61.2464519739652));
#35360=CARTESIAN_POINT('Ctrl Pts',(77.2912945088754,93.4660705196157,60.6057014773928));
#35361=CARTESIAN_POINT('Ctrl Pts',(79.4007230479312,93.6431670916144,59.9649509808205));
#35362=CARTESIAN_POINT('Ctrl Pts',(81.2118275942138,93.8202636636132,58.4014001198703));
#35363=CARTESIAN_POINT('Ctrl Pts',(82.1535440633138,93.9973602356119,56.4080561826466));
#35364=CARTESIAN_POINT('Ctrl Pts',(82.6515697929939,94.0910175649541,55.3538784110845));
#35365=CARTESIAN_POINT('Ctrl Pts',(82.9129498948704,94.1846748942963,54.188709927723));
#35366=CARTESIAN_POINT('Ctrl Pts',(82.9129498948689,94.2783322236386,53.0228109606255));
#35367=CARTESIAN_POINT('Ctrl Pts',(82.9129498948689,95.7216677763614,53.0228109606389));
#35368=CARTESIAN_POINT('Ctrl Pts',(82.912949894868,95.5445712043627,55.2274084205487));
#35369=CARTESIAN_POINT('Ctrl Pts',(81.9432795991088,95.367474632364,57.4147653849845));
#35370=CARTESIAN_POINT('Ctrl Pts',(80.3096882702518,95.1903780603652,58.8951806410948));
#35371=CARTESIAN_POINT('Ctrl Pts',(78.6760969413948,95.0132814883665,60.3755958972051));
#35372=CARTESIAN_POINT('Ctrl Pts',(76.4041347530412,94.8361849163678,61.1259150206686));
#35373=CARTESIAN_POINT('Ctrl Pts',(74.2101800112187,94.659088344369,60.9095529374018));
#35374=CARTESIAN_POINT('Ctrl Pts',(72.0162252693962,94.4819917723703,60.693190854135));
#35375=CARTESIAN_POINT('Ctrl Pts',(69.9345925076952,94.3048952003716,59.5135315737677));
#35376=CARTESIAN_POINT('Ctrl Pts',(68.6216467656588,94.1277986283728,57.7425365317901));
#35377=CARTESIAN_POINT('Ctrl Pts',(67.3087010236224,93.9507020563741,55.9715414898125));
#35378=CARTESIAN_POINT('Ctrl Pts',(66.7849774198237,93.7736054843754,53.6369099216271));
#35379=CARTESIAN_POINT('Ctrl Pts',(67.2156126057612,93.5965089123766,51.4747805783931));
#35380=CARTESIAN_POINT('Ctrl Pts',(67.6462477916987,93.4194123403779,49.3126512351591));
#35381=CARTESIAN_POINT('Ctrl Pts',(69.0245064207989,93.2423157683792,47.3568408855458));
#35382=CARTESIAN_POINT('Ctrl Pts',(70.9158061804492,93.0652191963804,46.2240411771297));
#35383=CARTESIAN_POINT('Ctrl Pts',(72.8071059400995,92.8881226243817,45.0912414687136));
#35384=CARTESIAN_POINT('Ctrl Pts',(75.1818659698133,92.711026052383,44.7991699473058));
#35385=CARTESIAN_POINT('Ctrl Pts',(77.2912945088696,92.5339294803842,45.4399204438765));
#35386=CARTESIAN_POINT('Ctrl Pts',(79.4007230479259,92.3568329083855,46.0806709404473));
#35387=CARTESIAN_POINT('Ctrl Pts',(81.2118275942097,92.1797363363868,47.6442218013961));
#35388=CARTESIAN_POINT('Ctrl Pts',(82.1535440633112,92.0026397643881,49.6375657386191));
#35389=CARTESIAN_POINT('Ctrl Pts',(82.6515697929919,91.9089824350458,50.6917435101805));
#35390=CARTESIAN_POINT('Ctrl Pts',(82.9129498948693,91.8153251057037,51.8569119935412));
#35391=CARTESIAN_POINT('Ctrl Pts',(82.9129498948689,91.7216677763615,53.0228109606383));
#35392=CARTESIAN_POINT('Origin',(74.9879498948689,255.,53.0228109606356));
#35393=CARTESIAN_POINT('',(82.923214744261,86.2783322236386,53.0234237509025));
#35394=CARTESIAN_POINT('',(82.9133860738174,87.7216677763614,53.0299211193051));
#35395=CARTESIAN_POINT('',(82.9129498948689,255.,53.0228109606356));
#35396=CARTESIAN_POINT('Ctrl Pts',(82.923214744261,86.2783322236386,53.0234237509025));
#35397=CARTESIAN_POINT('Ctrl Pts',(82.9231887310882,86.2803612189517,52.998261746315));
#35398=CARTESIAN_POINT('Ctrl Pts',(82.9230330643765,86.2823902142647,52.9731001886098));
#35399=CARTESIAN_POINT('Ctrl Pts',(82.9227472344118,86.2844192095777,52.947940164016));
#35400=CARTESIAN_POINT('Ctrl Pts',(82.8928602532351,86.4965752191301,50.3171551721588));
#35401=CARTESIAN_POINT('Ctrl Pts',(81.4398681471162,86.7087312286823,47.703132042207));
#35402=CARTESIAN_POINT('Ctrl Pts',(79.2163713661519,86.9208872382346,46.3036597142281));
#35403=CARTESIAN_POINT('Ctrl Pts',(76.9928745851877,87.1330432477869,44.9041873862493));
#35404=CARTESIAN_POINT('Ctrl Pts',(73.9988731293783,87.3451992573393,44.719265860243));
#35405=CARTESIAN_POINT('Ctrl Pts',(71.6178272157902,87.5573552668916,45.8348571255192));
#35406=CARTESIAN_POINT('Ctrl Pts',(69.236781302202,87.7695112764439,46.9504483907955));
#35407=CARTESIAN_POINT('Ctrl Pts',(67.4686909308351,87.9816672859962,49.3665524473543));
#35408=CARTESIAN_POINT('Ctrl Pts',(67.1207426280689,88.1938232955485,51.9722903221266));
#35409=CARTESIAN_POINT('Ctrl Pts',(66.7727943253027,88.4059793051008,54.5780281968992));
#35410=CARTESIAN_POINT('Ctrl Pts',(67.8449880911375,88.6181353146531,57.3733998898852));
#35411=CARTESIAN_POINT('Ctrl Pts',(69.8498961129948,88.8302913242055,59.0746545262256));
#35412=CARTESIAN_POINT('Ctrl Pts',(71.8548041348518,89.0424473337578,60.7759091625658));
#35413=CARTESIAN_POINT('Ctrl Pts',(74.7924264127309,89.2546033433102,61.3830467422606));
#35414=CARTESIAN_POINT('Ctrl Pts',(77.3052194191063,89.4667593528625,60.6160186861589));
#35415=CARTESIAN_POINT('Ctrl Pts',(79.8180124254817,89.6789153624148,59.8489906300571));
#35416=CARTESIAN_POINT('Ctrl Pts',(81.9059761603533,89.891071371967,57.7077969381589));
#35417=CARTESIAN_POINT('Ctrl Pts',(82.625093647743,90.1032273815193,55.1770276985099));
#35418=CARTESIAN_POINT('Ctrl Pts',(82.8229369775333,90.1615956622257,54.4807634272564));
#35419=CARTESIAN_POINT('Ctrl Pts',(82.9171712325869,90.2199639429321,53.7550118690877));
#35420=CARTESIAN_POINT('Ctrl Pts',(82.9127205943178,90.2783322236385,53.0279097020349));
#35421=CARTESIAN_POINT('Ctrl Pts',(82.9000974149753,91.7216677763615,53.0224942304407));
#35422=CARTESIAN_POINT('Ctrl Pts',(82.9004702208451,91.6148803125606,54.3566851265562));
#35423=CARTESIAN_POINT('Ctrl Pts',(82.5815271080044,91.5080928487596,55.6910138645003));
#35424=CARTESIAN_POINT('Ctrl Pts',(81.9431078719293,91.4013053849587,56.8503669330465));
#35425=CARTESIAN_POINT('Ctrl Pts',(80.6747522735636,91.1891493754064,59.1536683874527));
#35426=CARTESIAN_POINT('Ctrl Pts',(78.1454156900416,90.9769933658541,60.7663360951428));
#35427=CARTESIAN_POINT('Ctrl Pts',(75.524149721516,90.7648373563018,60.9436083546364));
#35428=CARTESIAN_POINT('Ctrl Pts',(72.9028837529902,90.5526813467495,61.1208806141299));
#35429=CARTESIAN_POINT('Ctrl Pts',(70.1896883994607,90.3405253371971,59.8627574254265));
#35430=CARTESIAN_POINT('Ctrl Pts',(68.6171357769601,90.1283693276448,57.7534918768312));
#35431=CARTESIAN_POINT('Ctrl Pts',(67.8308594657099,90.0222913228686,56.6988591025336));
#35432=CARTESIAN_POINT('Ctrl Pts',(67.3297438372168,89.9162133180924,55.4314407382631));
#35433=CARTESIAN_POINT('Ctrl Pts',(67.1462614461992,89.8101353133163,54.1195962942507));
#35434=CARTESIAN_POINT('Ctrl Pts',(66.9627790551816,89.7040573085401,52.8077518502383));
#35435=CARTESIAN_POINT('Ctrl Pts',(67.0969299016394,89.597979303764,51.4514813264839));
#35436=CARTESIAN_POINT('Ctrl Pts',(67.563679444442,89.4919012989879,50.2215928800997));
#35437=CARTESIAN_POINT('Ctrl Pts',(68.4971785300472,89.2797452894356,47.7618159873313));
#35438=CARTESIAN_POINT('Ctrl Pts',(70.7610724010317,89.0675892798832,45.8075674040433));
#35439=CARTESIAN_POINT('Ctrl Pts',(73.3303864196594,88.8554332703309,45.2588541771032));
#35440=CARTESIAN_POINT('Ctrl Pts',(75.8997004382875,88.6432772607786,44.7101409501631));
#35441=CARTESIAN_POINT('Ctrl Pts',(78.7744346045589,88.4311212512264,45.5669630795712));
#35442=CARTESIAN_POINT('Ctrl Pts',(80.6260625288807,88.2189652416741,47.4338850232124));
#35443=CARTESIAN_POINT('Ctrl Pts',(82.0728121408136,88.0531994199032,48.892584453046));
#35444=CARTESIAN_POINT('Ctrl Pts',(82.8949645428175,87.8874335981323,50.9679407850187));
#35445=CARTESIAN_POINT('Ctrl Pts',(82.9133860738174,87.7216677763614,53.0299211193051));
#35446=CARTESIAN_POINT('Origin',(74.9879498948689,255.,53.0228109606356));
#35447=CARTESIAN_POINT('',(82.9112619154184,82.2783322236386,53.0204263509097));
#35448=CARTESIAN_POINT('',(82.9253497859361,83.7216677763615,53.0207628815399));
#35449=CARTESIAN_POINT('',(82.9129498948689,255.,53.0228109606356));
#35450=CARTESIAN_POINT('Ctrl Pts',(82.9076441624805,82.2783322236387,53.0153155489345));
#35451=CARTESIAN_POINT('Ctrl Pts',(82.9148898770911,82.3407584949712,52.2380428063635));
#35452=CARTESIAN_POINT('Ctrl Pts',(82.8102713239623,82.4031847663036,51.4624782333206));
#35453=CARTESIAN_POINT('Ctrl Pts',(82.5863312910923,82.4656110376361,50.7225627634984));
#35454=CARTESIAN_POINT('Ctrl Pts',(81.8252699183938,82.6777670471884,48.2079561702668));
#35455=CARTESIAN_POINT('Ctrl Pts',(79.6860648096109,82.8899230567406,46.105090936656));
#35456=CARTESIAN_POINT('Ctrl Pts',(77.1568571560168,83.1020790662929,45.3860414538124));
#35457=CARTESIAN_POINT('Ctrl Pts',(74.6276495024229,83.3142350758453,44.6669919709688));
#35458=CARTESIAN_POINT('Ctrl Pts',(71.7084393040178,83.5263910853977,45.3317582388919));
#35459=CARTESIAN_POINT('Ctrl Pts',(69.7370844997,83.73854709495,47.0709241679838));
#35460=CARTESIAN_POINT('Ctrl Pts',(67.7657296953823,83.9507031045023,48.8100900970757));
#35461=CARTESIAN_POINT('Ctrl Pts',(66.7422302851519,84.1628591140545,51.6236556873363));
#35462=CARTESIAN_POINT('Ctrl Pts',(67.1403706679598,84.3750151236068,54.2227724121782));
#35463=CARTESIAN_POINT('Ctrl Pts',(67.5385110507677,84.5871711331591,56.8218891370208));
#35464=CARTESIAN_POINT('Ctrl Pts',(69.3582912266146,84.7993271427115,59.2065569964446));
#35465=CARTESIAN_POINT('Ctrl Pts',(71.7584050082544,85.0114831522639,60.2751610236323));
#35466=CARTESIAN_POINT('Ctrl Pts',(74.1585187898934,85.2236391618162,61.3437650508196));
#35467=CARTESIAN_POINT('Ctrl Pts',(77.1389661773251,85.4357951713685,61.0963052457719));
#35468=CARTESIAN_POINT('Ctrl Pts',(79.3413937306905,85.6479511809208,59.6571263905914));
#35469=CARTESIAN_POINT('Ctrl Pts',(80.4426075073733,85.7540291856969,58.9375369630011));
#35470=CARTESIAN_POINT('Ctrl Pts',(81.3493163255395,85.8601071904731,57.9200177728776));
#35471=CARTESIAN_POINT('Ctrl Pts',(81.9730871299462,85.9661851952492,56.7514666971134));
#35472=CARTESIAN_POINT('Ctrl Pts',(82.5849268272283,86.0702342047124,55.6052669529073));
#35473=CARTESIAN_POINT('Ctrl Pts',(82.9245487270679,86.1742832141755,54.3137577583859));
#35474=CARTESIAN_POINT('Ctrl Pts',(82.923214744261,86.2783322236386,53.0234237509025));
#35475=CARTESIAN_POINT('Ctrl Pts',(82.9133860738174,87.7216677763614,53.0299211193051));
#35476=CARTESIAN_POINT('Ctrl Pts',(82.9185414084526,87.6752775885799,53.6069740599373));
#35477=CARTESIAN_POINT('Ctrl Pts',(82.8607500486254,87.6288874007985,54.1829794175166));
#35478=CARTESIAN_POINT('Ctrl Pts',(82.7360858105918,87.5824972130171,54.7441283695434));
#35479=CARTESIAN_POINT('Ctrl Pts',(82.1659594856094,87.3703412034647,57.3104280143593));
#35480=CARTESIAN_POINT('Ctrl Pts',(80.1971851532724,87.1581851939125,59.5660055461174));
#35481=CARTESIAN_POINT('Ctrl Pts',(77.7292412067298,86.9460291843602,60.4732961227791));
#35482=CARTESIAN_POINT('Ctrl Pts',(75.2612972601866,86.7338731748078,61.380586699441));
#35483=CARTESIAN_POINT('Ctrl Pts',(72.2941836994374,86.5217171652554,60.9395903210058));
#35484=CARTESIAN_POINT('Ctrl Pts',(70.1988923804859,86.3095611557031,59.354593469127));
#35485=CARTESIAN_POINT('Ctrl Pts',(68.1036010615352,86.0974051461508,57.7695966172488));
#35486=CARTESIAN_POINT('Ctrl Pts',(66.8801319843817,85.8852491365986,55.0405992919284));
#35487=CARTESIAN_POINT('Ctrl Pts',(67.0759628953565,85.6730931270463,52.4169428435099));
#35488=CARTESIAN_POINT('Ctrl Pts',(67.173878350844,85.5670151222701,51.1051146193002));
#35489=CARTESIAN_POINT('Ctrl Pts',(67.6266188033639,85.4609371174939,49.819621614316));
#35490=CARTESIAN_POINT('Ctrl Pts',(68.3483029371681,85.3548591127177,48.7088679764125));
#35491=CARTESIAN_POINT('Ctrl Pts',(69.0699870709721,85.2487811079416,47.5981143385093));
#35492=CARTESIAN_POINT('Ctrl Pts',(70.0606148860604,85.1427031031655,46.6621000676865));
#35493=CARTESIAN_POINT('Ctrl Pts',(71.2194816091533,85.0366250983894,46.0395981445058));
#35494=CARTESIAN_POINT('Ctrl Pts',(73.5372150553394,84.8244690888371,44.7945942981443));
#35495=CARTESIAN_POINT('Ctrl Pts',(76.5279041335448,84.6123130792847,44.8036398423513));
#35496=CARTESIAN_POINT('Ctrl Pts',(78.827536031194,84.4001570697323,46.0741333948936));
#35497=CARTESIAN_POINT('Ctrl Pts',(81.127167928843,84.18800106018,47.3446269474357));
#35498=CARTESIAN_POINT('Ctrl Pts',(82.7357426459362,83.9758450506277,49.8765685083131));
#35499=CARTESIAN_POINT('Ctrl Pts',(82.9095242971506,83.7636890410754,52.5002535983109));
#35500=CARTESIAN_POINT('Ctrl Pts',(82.9209978110418,83.7496819528374,52.6734760709703));
#35501=CARTESIAN_POINT('Ctrl Pts',(82.9262170881152,83.7356748645995,52.8470984520006));
#35502=CARTESIAN_POINT('Ctrl Pts',(82.9253497859361,83.7216677763615,53.0207628815399));
#35503=CARTESIAN_POINT('Origin',(74.9879498948689,255.,53.0228109606356));
#35504=CARTESIAN_POINT('',(82.9085981452144,78.2783322236386,53.0246573544551));
#35505=CARTESIAN_POINT('',(82.911245752919,79.7216677763615,53.0212425220677));
#35506=CARTESIAN_POINT('',(82.9129498948689,255.,53.0228109606356));
#35507=CARTESIAN_POINT('Ctrl Pts',(82.9129498948689,78.2783322236386,53.0228109606257));
#35508=CARTESIAN_POINT('Ctrl Pts',(82.9129498948662,78.4554287956373,50.8182135007157));
#35509=CARTESIAN_POINT('Ctrl Pts',(81.9432795991051,78.6325253676361,48.6308565362806));
#35510=CARTESIAN_POINT('Ctrl Pts',(80.3096882702466,78.8096219396348,47.1504412801716));
#35511=CARTESIAN_POINT('Ctrl Pts',(78.6760969413882,78.9867185116336,45.6700260240627));
#35512=CARTESIAN_POINT('Ctrl Pts',(76.4041347530337,79.1638150836323,44.9197069006012));
#35513=CARTESIAN_POINT('Ctrl Pts',(74.2101800112113,79.340911655631,45.1360689838701));
#35514=CARTESIAN_POINT('Ctrl Pts',(72.0162252693889,79.5180082276298,45.352431067139));
#35515=CARTESIAN_POINT('Ctrl Pts',(69.9345925076889,79.6951047996286,46.5320903475084));
#35516=CARTESIAN_POINT('Ctrl Pts',(68.6216467656541,79.8722013716273,48.3030853894874));
#35517=CARTESIAN_POINT('Ctrl Pts',(67.3087010236194,80.049297943626,50.0740804314665));
#35518=CARTESIAN_POINT('Ctrl Pts',(66.784977419823,80.2263945156247,52.4087119996525));
#35519=CARTESIAN_POINT('Ctrl Pts',(67.2156126057628,80.4034910876235,54.5708413428862));
#35520=CARTESIAN_POINT('Ctrl Pts',(67.6462477917027,80.5805876596222,56.7329706861199));
#35521=CARTESIAN_POINT('Ctrl Pts',(69.0245064208051,80.757684231621,58.6887810357319));
#35522=CARTESIAN_POINT('Ctrl Pts',(70.9158061804568,80.9347808036198,59.8215807441459));
#35523=CARTESIAN_POINT('Ctrl Pts',(72.8071059401084,81.1118773756185,60.95438045256));
#35524=CARTESIAN_POINT('Ctrl Pts',(75.1818659698227,81.2889739476172,61.2464519739651));
#35525=CARTESIAN_POINT('Ctrl Pts',(77.2912945088785,81.466070519616,60.6057014773919));
#35526=CARTESIAN_POINT('Ctrl Pts',(79.4007230479342,81.6431670916147,59.9649509808187));
#35527=CARTESIAN_POINT('Ctrl Pts',(81.2118275942163,81.8202636636135,58.4014001198676));
#35528=CARTESIAN_POINT('Ctrl Pts',(82.1535440633154,81.9973602356122,56.4080561826433));
#35529=CARTESIAN_POINT('Ctrl Pts',(82.6515697929944,82.0910175649544,55.3538784110821));
#35530=CARTESIAN_POINT('Ctrl Pts',(82.9129498948703,82.1846748942964,54.1887099277221));
#35531=CARTESIAN_POINT('Ctrl Pts',(82.9129498948689,82.2783322236386,53.0228109606259));
#35532=CARTESIAN_POINT('Ctrl Pts',(82.9253497859361,83.7216677763615,53.0207628815399));
#35533=CARTESIAN_POINT('Ctrl Pts',(82.91308064132,83.5235188550472,55.4774775676541));
#35534=CARTESIAN_POINT('Ctrl Pts',(81.6827731049543,83.3253699337328,57.9426069471548));
#35535=CARTESIAN_POINT('Ctrl Pts',(79.7090566453533,83.1272210124185,59.4030691718097));
#35536=CARTESIAN_POINT('Ctrl Pts',(77.5958187570055,82.9150650028661,60.9667710361928));
#35537=CARTESIAN_POINT('Ctrl Pts',(74.6303543949743,82.7029089933138,61.3787461458397));
#35538=CARTESIAN_POINT('Ctrl Pts',(72.1721275036747,82.4907529837614,60.4454487309336));
#35539=CARTESIAN_POINT('Ctrl Pts',(69.713900612376,82.2785969742091,59.5121513160278));
#35540=CARTESIAN_POINT('Ctrl Pts',(67.7629111918085,82.0664409646569,57.23358137657));
#35541=CARTESIAN_POINT('Ctrl Pts',(67.2202981950566,81.8542849551046,54.6629721360415));
#35542=CARTESIAN_POINT('Ctrl Pts',(66.6776851983047,81.6421289455523,52.0923628955127));
#35543=CARTESIAN_POINT('Ctrl Pts',(67.5434486253686,81.429972936,49.2297143539131));
#35544=CARTESIAN_POINT('Ctrl Pts',(69.4117049022399,81.2178169264477,47.377272347006));
#35545=CARTESIAN_POINT('Ctrl Pts',(70.3458330406758,81.1117389216715,46.4510513435522));
#35546=CARTESIAN_POINT('Ctrl Pts',(71.5305843915636,81.0056609168953,45.7773819737716));
#35547=CARTESIAN_POINT('Ctrl Pts',(72.8038060612515,80.8995829121191,45.4119942168095));
#35548=CARTESIAN_POINT('Ctrl Pts',(74.0770277309391,80.7935049073429,45.0466064598474));
#35549=CARTESIAN_POINT('Ctrl Pts',(75.4387197194266,80.6874269025668,44.9895003157035));
#35550=CARTESIAN_POINT('Ctrl Pts',(76.7218528853392,80.5813488977906,45.2794141042527));
#35551=CARTESIAN_POINT('Ctrl Pts',(79.2881192171644,80.3691928882383,45.859241681351));
#35552=CARTESIAN_POINT('Ctrl Pts',(81.5401502586898,80.1570368786861,47.8271489892214));
#35553=CARTESIAN_POINT('Ctrl Pts',(82.4432684135962,79.9448808691338,50.2943008552432));
#35554=CARTESIAN_POINT('Ctrl Pts',(82.7599972788634,79.8704765048764,51.1595455707012));
#35555=CARTESIAN_POINT('Ctrl Pts',(82.9108171050971,79.796072140619,52.0861946849957));
#35556=CARTESIAN_POINT('Ctrl Pts',(82.9045916518496,79.7216677763616,53.0151182970485));
#35557=CARTESIAN_POINT('Origin',(74.9879498948689,255.,53.0228109606356));
#35558=CARTESIAN_POINT('',(82.9153733449052,74.2783322236386,53.0241785897874));
#35559=CARTESIAN_POINT('',(82.9105899036684,75.7216677763615,53.0242486736905));
#35560=CARTESIAN_POINT('',(82.9129498948689,255.,53.0228109606356));
#35561=CARTESIAN_POINT('Ctrl Pts',(82.9213292833048,74.2783322236386,53.0275397134229));
#35562=CARTESIAN_POINT('Ctrl Pts',(82.9025944532997,74.4615530470099,50.7531106339741));
#35563=CARTESIAN_POINT('Ctrl Pts',(81.8714282549828,74.6447738703813,48.4655481839494));
#35564=CARTESIAN_POINT('Ctrl Pts',(80.1458417428987,74.8279946937527,46.9901750960443));
#35565=CARTESIAN_POINT('Ctrl Pts',(78.1477416263029,75.040150703305,45.2818034100573));
#35566=CARTESIAN_POINT('Ctrl Pts',(75.2185691545151,75.2523067128573,44.6624077336402));
#35567=CARTESIAN_POINT('Ctrl Pts',(72.7008217304853,75.4644627224097,45.4206104918576));
#35568=CARTESIAN_POINT('Ctrl Pts',(70.1830743064558,75.676618731962,46.1788132500749));
#35569=CARTESIAN_POINT('Ctrl Pts',(68.0767519301841,75.8887747415143,48.3146144429265));
#35570=CARTESIAN_POINT('Ctrl Pts',(67.3547954479706,76.1009307510666,50.8407259942096));
#35571=CARTESIAN_POINT('Ctrl Pts',(66.632838965757,76.3130867606189,53.3668375454927));
#35572=CARTESIAN_POINT('Ctrl Pts',(67.2952483776016,76.5252427701712,56.2832594552074));
#35573=CARTESIAN_POINT('Ctrl Pts',(69.0286775479858,76.7373987797235,58.262437622095));
#35574=CARTESIAN_POINT('Ctrl Pts',(69.8953921331778,76.8434767844997,59.2520267055389));
#35575=CARTESIAN_POINT('Ctrl Pts',(71.0298616580048,76.9495547892759,60.0073048532759));
#35576=CARTESIAN_POINT('Ctrl Pts',(72.2742514908426,77.055632794052,60.4612823604607));
#35577=CARTESIAN_POINT('Ctrl Pts',(73.5186413236806,77.1617107988282,60.9152598676457));
#35578=CARTESIAN_POINT('Ctrl Pts',(74.8729514645296,77.2677888036043,61.0679367342783));
#35579=CARTESIAN_POINT('Ctrl Pts',(76.1732887679165,77.3738668083805,60.8689301422339));
#35580=CARTESIAN_POINT('Ctrl Pts',(78.7739633746896,77.5860228179328,60.4709169581452));
#35581=CARTESIAN_POINT('Ctrl Pts',(81.1587466316146,77.7981788274851,58.6661699393487));
#35582=CARTESIAN_POINT('Ctrl Pts',(82.2330447085192,78.0103348370374,56.2685994244952));
#35583=CARTESIAN_POINT('Ctrl Pts',(82.6853990516724,78.0996672992378,55.2590551846553));
#35584=CARTESIAN_POINT('Ctrl Pts',(82.9054048022027,78.1889997614382,54.1444035333906));
#35585=CARTESIAN_POINT('Ctrl Pts',(82.9011716266685,78.2783322236386,53.0278083348896));
#35586=CARTESIAN_POINT('Ctrl Pts',(82.9129498948689,79.7216677763615,53.0228109606377));
#35587=CARTESIAN_POINT('Ctrl Pts',(82.9129498948683,79.5445712043628,55.2274084205477));
#35588=CARTESIAN_POINT('Ctrl Pts',(81.9432795991093,79.367474632364,57.4147653849839));
#35589=CARTESIAN_POINT('Ctrl Pts',(80.3096882702523,79.1903780603653,58.8951806410944));
#35590=CARTESIAN_POINT('Ctrl Pts',(78.6760969413953,79.0132814883665,60.3755958972049));
#35591=CARTESIAN_POINT('Ctrl Pts',(76.4041347530416,78.8361849163678,61.1259150206686));
#35592=CARTESIAN_POINT('Ctrl Pts',(74.2101800112189,78.6590883443691,60.9095529374018));
#35593=CARTESIAN_POINT('Ctrl Pts',(72.0162252693963,78.4819917723703,60.6931908541351));
#35594=CARTESIAN_POINT('Ctrl Pts',(69.9345925076951,78.3048952003716,59.5135315737677));
#35595=CARTESIAN_POINT('Ctrl Pts',(68.6216467656587,78.1277986283728,57.7425365317899));
#35596=CARTESIAN_POINT('Ctrl Pts',(67.3087010236222,77.9507020563741,55.9715414898121));
#35597=CARTESIAN_POINT('Ctrl Pts',(66.7849774198236,77.7736054843754,53.6369099216265));
#35598=CARTESIAN_POINT('Ctrl Pts',(67.2156126057613,77.5965089123766,51.4747805783924));
#35599=CARTESIAN_POINT('Ctrl Pts',(67.6462477916991,77.4194123403779,49.3126512351583));
#35600=CARTESIAN_POINT('Ctrl Pts',(69.0245064207996,77.2423157683791,47.356840885545));
#35601=CARTESIAN_POINT('Ctrl Pts',(70.9158061804502,77.0652191963804,46.2240411771291));
#35602=CARTESIAN_POINT('Ctrl Pts',(72.8071059401008,76.8881226243816,45.0912414687133));
#35603=CARTESIAN_POINT('Ctrl Pts',(75.1818659698148,76.7110260523829,44.7991699473058));
#35604=CARTESIAN_POINT('Ctrl Pts',(77.2912945088711,76.5339294803842,45.439920443877));
#35605=CARTESIAN_POINT('Ctrl Pts',(79.4007230479274,76.3568329083854,46.0806709404482));
#35606=CARTESIAN_POINT('Ctrl Pts',(81.211827594211,76.1797363363866,47.6442218013975));
#35607=CARTESIAN_POINT('Ctrl Pts',(82.1535440633121,76.0026397643879,49.6375657386209));
#35608=CARTESIAN_POINT('Ctrl Pts',(82.6515697929922,75.9089824350457,50.6917435101819));
#35609=CARTESIAN_POINT('Ctrl Pts',(82.9129498948693,75.8153251057036,51.856911993542));
#35610=CARTESIAN_POINT('Ctrl Pts',(82.9129498948689,75.7216677763615,53.0228109606385));
#35611=CARTESIAN_POINT('Origin',(74.9879498948689,255.,53.0228109606356));
#35612=CARTESIAN_POINT('',(82.9144228299092,70.2783322236386,53.0212847568831));
#35613=CARTESIAN_POINT('',(82.9149525301073,71.7216677763616,53.0232506905358));
#35614=CARTESIAN_POINT('',(82.9129498948689,255.,53.0228109606356));
#35615=CARTESIAN_POINT('Ctrl Pts',(82.9129498948689,70.2783322236386,53.0228109606254));
#35616=CARTESIAN_POINT('Ctrl Pts',(82.9129498948661,70.4554287956373,50.8182135007157));
#35617=CARTESIAN_POINT('Ctrl Pts',(81.9432795991052,70.6325253676361,48.6308565362808));
#35618=CARTESIAN_POINT('Ctrl Pts',(80.3096882702471,70.8096219396348,47.150441280172));
#35619=CARTESIAN_POINT('Ctrl Pts',(78.6760969413889,70.9867185116335,45.6700260240632));
#35620=CARTESIAN_POINT('Ctrl Pts',(76.4041347530349,71.1638150836322,44.9197069006015));
#35621=CARTESIAN_POINT('Ctrl Pts',(74.2101800112128,71.3409116556309,45.1360689838699));
#35622=CARTESIAN_POINT('Ctrl Pts',(72.0162252693906,71.5180082276296,45.3524310671384));
#35623=CARTESIAN_POINT('Ctrl Pts',(69.9345925076906,71.6951047996284,46.5320903475071));
#35624=CARTESIAN_POINT('Ctrl Pts',(68.6216467656555,71.8722013716271,48.3030853894855));
#35625=CARTESIAN_POINT('Ctrl Pts',(67.3087010236204,72.0492979436258,50.0740804314639));
#35626=CARTESIAN_POINT('Ctrl Pts',(66.7849774198233,72.2263945156245,52.4087119996495));
#35627=CARTESIAN_POINT('Ctrl Pts',(67.2156126057622,72.4034910876232,54.570841342883));
#35628=CARTESIAN_POINT('Ctrl Pts',(67.6462477917011,72.580587659622,56.7329706861166));
#35629=CARTESIAN_POINT('Ctrl Pts',(69.0245064208023,72.7576842316206,58.6887810357289));
#35630=CARTESIAN_POINT('Ctrl Pts',(70.9158061804532,72.9347808036194,59.8215807441438));
#35631=CARTESIAN_POINT('Ctrl Pts',(72.807105940104,73.1118773756181,60.9543804525587));
#35632=CARTESIAN_POINT('Ctrl Pts',(75.1818659698178,73.2889739476168,61.2464519739652));
#35633=CARTESIAN_POINT('Ctrl Pts',(77.2912945088736,73.4660705196156,60.6057014773934));
#35634=CARTESIAN_POINT('Ctrl Pts',(79.4007230479294,73.6431670916143,59.9649509808216));
#35635=CARTESIAN_POINT('Ctrl Pts',(81.2118275942123,73.820263663613,58.401400119872));
#35636=CARTESIAN_POINT('Ctrl Pts',(82.1535440633128,73.9973602356117,56.4080561826487));
#35637=CARTESIAN_POINT('Ctrl Pts',(82.6515697929935,74.091017564954,55.353878411086));
#35638=CARTESIAN_POINT('Ctrl Pts',(82.9129498948704,74.1846748942963,54.1887099277238));
#35639=CARTESIAN_POINT('Ctrl Pts',(82.9129498948689,74.2783322236386,53.0228109606255));
#35640=CARTESIAN_POINT('Ctrl Pts',(82.9024847110463,75.7216677763615,53.0291863790398));
#35641=CARTESIAN_POINT('Ctrl Pts',(82.9094436057292,75.644313407086,53.993811927591));
#35642=CARTESIAN_POINT('Ctrl Pts',(82.7471053581289,75.5669590378106,54.9563720673458));
#35643=CARTESIAN_POINT('Ctrl Pts',(82.4058558444903,75.4896046685351,55.8514524956269));
#35644=CARTESIAN_POINT('Ctrl Pts',(81.4699276512495,75.2774486589828,58.3063453952938));
#35645=CARTESIAN_POINT('Ctrl Pts',(79.1882052139606,75.0652926494305,60.2536469660177));
#35646=CARTESIAN_POINT('Ctrl Pts',(76.6147118588759,74.8531366398782,60.7931425314416));
#35647=CARTESIAN_POINT('Ctrl Pts',(74.0412185037915,74.6409806303259,61.3326380968654));
#35648=CARTESIAN_POINT('Ctrl Pts',(71.1759542309114,74.4288246207735,60.4643276569895));
#35649=CARTESIAN_POINT('Ctrl Pts',(69.3317194678335,74.2166686112212,58.5908987066219));
#35650=CARTESIAN_POINT('Ctrl Pts',(67.4874847047556,74.0045126016689,56.7174697562543));
#35651=CARTESIAN_POINT('Ctrl Pts',(66.6642794514797,73.7923565921166,53.8389222953949));
#35652=CARTESIAN_POINT('Ctrl Pts',(67.2441244107334,73.5802005825643,51.2742189330149));
#35653=CARTESIAN_POINT('Ctrl Pts',(67.8239693699872,73.368044573012,48.7095155706345));
#35654=CARTESIAN_POINT('Ctrl Pts',(69.8068645417708,73.1558885634596,46.4586563067335));
#35655=CARTESIAN_POINT('Ctrl Pts',(72.2761531551931,72.9437325539073,45.5613968819512));
#35656=CARTESIAN_POINT('Ctrl Pts',(74.7454417686152,72.731576544355,44.664137457169));
#35657=CARTESIAN_POINT('Ctrl Pts',(77.7011238236759,72.5194205348028,45.1204778715052));
#35658=CARTESIAN_POINT('Ctrl Pts',(79.7969456072804,72.3072645252504,46.7109035869639));
#35659=CARTESIAN_POINT('Ctrl Pts',(80.8448564990826,72.2011865204743,47.5061164446932));
#35660=CARTESIAN_POINT('Ctrl Pts',(81.6778023230208,72.095108515698,48.5848506277031));
#35661=CARTESIAN_POINT('Ctrl Pts',(82.2178940525135,71.9890305109219,49.794355715263));
#35662=CARTESIAN_POINT('Ctrl Pts',(82.6716494501422,71.8999095994018,50.8105154377147));
#35663=CARTESIAN_POINT('Ctrl Pts',(82.9186956245664,71.8107886878817,51.9189789817963));
#35664=CARTESIAN_POINT('Ctrl Pts',(82.922415508883,71.7216677763616,53.0248893788183));
#35665=CARTESIAN_POINT('Origin',(74.9879498948689,255.,53.0228109606356));
#35666=CARTESIAN_POINT('',(82.908625053032,66.2783322236386,53.0218734498001));
#35667=CARTESIAN_POINT('',(82.9131277587349,67.7216677763615,53.0225723293765));
#35668=CARTESIAN_POINT('',(82.9129498948689,255.,53.0228109606356));
#35669=CARTESIAN_POINT('Ctrl Pts',(82.9012831846627,66.2783322236387,53.0202819278075));
#35670=CARTESIAN_POINT('Ctrl Pts',(82.9054592133395,66.3701915894966,51.8729674294636));
#35671=CARTESIAN_POINT('Ctrl Pts',(82.6726571039608,66.4620509553545,50.7270111641337));
#35672=CARTESIAN_POINT('Ctrl Pts',(82.194940541544,66.5539103212124,49.6935928802838));
#35673=CARTESIAN_POINT('Ctrl Pts',(81.0916187557596,66.7660663307647,47.3068368075379));
#35674=CARTESIAN_POINT('Ctrl Pts',(78.6818908535276,66.978222340317,45.5203732267803));
#35675=CARTESIAN_POINT('Ctrl Pts',(76.0795684308802,67.1903783498693,45.159293262891));
#35676=CARTESIAN_POINT('Ctrl Pts',(73.4772460082324,67.4025343594217,44.7982132990016));
#35677=CARTESIAN_POINT('Ctrl Pts',(70.6823290651691,67.614690368974,45.8625169519807));
#35678=CARTESIAN_POINT('Ctrl Pts',(68.9654077236915,67.8268463785263,47.8560324428168));
#35679=CARTESIAN_POINT('Ctrl Pts',(68.1069470529528,67.9329243833025,48.8527901882348));
#35680=CARTESIAN_POINT('Ctrl Pts',(67.5179852826105,68.0390023880786,50.0818508931169));
#35681=CARTESIAN_POINT('Ctrl Pts',(67.2427484732325,68.1450803928548,51.3775539192241));
#35682=CARTESIAN_POINT('Ctrl Pts',(66.9675116638546,68.2511583976309,52.6732569453312));
#35683=CARTESIAN_POINT('Ctrl Pts',(67.0059998154409,68.3572364024071,54.0356022926634));
#35684=CARTESIAN_POINT('Ctrl Pts',(67.3851473064755,68.4633144071832,55.2952561761957));
#35685=CARTESIAN_POINT('Ctrl Pts',(68.1434422885447,68.6754704167355,57.8145639432602));
#35686=CARTESIAN_POINT('Ctrl Pts',(70.2643746284068,68.8876264262879,59.9231058551253));
#35687=CARTESIAN_POINT('Ctrl Pts',(72.7887653822357,69.0997824358402,60.6510564397939));
#35688=CARTESIAN_POINT('Ctrl Pts',(75.3131561360648,69.3119384453925,61.3790070244627));
#35689=CARTESIAN_POINT('Ctrl Pts',(78.241005303861,69.5240944549449,60.7263662819347));
#35690=CARTESIAN_POINT('Ctrl Pts',(80.2192776127132,69.7362504644972,58.9942109234851));
#35691=CARTESIAN_POINT('Ctrl Pts',(81.9041781653871,69.916944384211,57.5189289273164));
#35692=CARTESIAN_POINT('Ctrl Pts',(82.9002574879822,70.0976383039249,55.2605691016666));
#35693=CARTESIAN_POINT('Ctrl Pts',(82.9187125221374,70.2783322236387,53.0168399279172));
#35694=CARTESIAN_POINT('Ctrl Pts',(82.9129498948689,71.7216677763616,53.0228109606374));
#35695=CARTESIAN_POINT('Ctrl Pts',(82.9129498948684,71.5445712043629,55.2274084205471));
#35696=CARTESIAN_POINT('Ctrl Pts',(81.9432795991098,71.3674746323641,57.414765384983));
#35697=CARTESIAN_POINT('Ctrl Pts',(80.3096882702532,71.1903780603654,58.8951806410935));
#35698=CARTESIAN_POINT('Ctrl Pts',(78.6760969413967,71.0132814883667,60.3755958972041));
#35699=CARTESIAN_POINT('Ctrl Pts',(76.4041347530435,70.836184916368,61.1259150206682));
#35700=CARTESIAN_POINT('Ctrl Pts',(74.2101800112211,70.6590883443693,60.909552937402));
#35701=CARTESIAN_POINT('Ctrl Pts',(72.0162252693987,70.4819917723705,60.6931908541359));
#35702=CARTESIAN_POINT('Ctrl Pts',(69.9345925076975,70.3048952003718,59.5135315737694));
#35703=CARTESIAN_POINT('Ctrl Pts',(68.6216467656605,70.1277986283731,57.7425365317923));
#35704=CARTESIAN_POINT('Ctrl Pts',(67.3087010236235,69.9507020563743,55.9715414898153));
#35705=CARTESIAN_POINT('Ctrl Pts',(66.7849774198239,69.7736054843757,53.6369099216303));
#35706=CARTESIAN_POINT('Ctrl Pts',(67.2156126057606,69.5965089123769,51.4747805783963));
#35707=CARTESIAN_POINT('Ctrl Pts',(67.6462477916972,69.4194123403782,49.3126512351623));
#35708=CARTESIAN_POINT('Ctrl Pts',(69.0245064207964,69.2423157683795,47.3568408855485));
#35709=CARTESIAN_POINT('Ctrl Pts',(70.915806180446,69.0652191963807,46.2240411771316));
#35710=CARTESIAN_POINT('Ctrl Pts',(72.8071059400957,68.888122624382,45.0912414687147));
#35711=CARTESIAN_POINT('Ctrl Pts',(75.1818659698091,68.7110260523833,44.7991699473058));
#35712=CARTESIAN_POINT('Ctrl Pts',(77.2912945088656,68.5339294803846,45.4399204438753));
#35713=CARTESIAN_POINT('Ctrl Pts',(79.4007230479221,68.3568329083859,46.0806709404449));
#35714=CARTESIAN_POINT('Ctrl Pts',(81.2118275942067,68.1797363363871,47.6442218013926));
#35715=CARTESIAN_POINT('Ctrl Pts',(82.1535440633093,68.0026397643884,49.6375657386149));
#35716=CARTESIAN_POINT('Ctrl Pts',(82.6515697929912,67.9089824350461,50.6917435101773));
#35717=CARTESIAN_POINT('Ctrl Pts',(82.9129498948693,67.8153251057038,51.8569119935396));
#35718=CARTESIAN_POINT('Ctrl Pts',(82.9129498948689,67.7216677763615,53.0228109606381));
#35719=CARTESIAN_POINT('Origin',(74.9879498948689,255.,53.0228109606356));
#35720=CARTESIAN_POINT('',(82.9129498948689,62.2783322236386,53.022810960625));
#35721=CARTESIAN_POINT('',(82.9062487487382,63.7216677763616,53.0219139020423));
#35722=CARTESIAN_POINT('',(82.9129498948689,255.,53.0228109606356));
#35723=CARTESIAN_POINT('Ctrl Pts',(82.9129498948689,62.2783322236386,53.022810960625));
#35724=CARTESIAN_POINT('Ctrl Pts',(82.912949894866,62.4554287956374,50.8182135007154));
#35725=CARTESIAN_POINT('Ctrl Pts',(81.943279599105,62.6325253676361,48.6308565362805));
#35726=CARTESIAN_POINT('Ctrl Pts',(80.3096882702468,62.8096219396348,47.1504412801718));
#35727=CARTESIAN_POINT('Ctrl Pts',(78.6760969413886,62.9867185116335,45.670026024063));
#35728=CARTESIAN_POINT('Ctrl Pts',(76.4041347530346,63.1638150836322,44.9197069006014));
#35729=CARTESIAN_POINT('Ctrl Pts',(74.2101800112124,63.3409116556309,45.1360689838699));
#35730=CARTESIAN_POINT('Ctrl Pts',(72.0162252693903,63.5180082276297,45.3524310671385));
#35731=CARTESIAN_POINT('Ctrl Pts',(69.9345925076903,63.6951047996283,46.5320903475073));
#35732=CARTESIAN_POINT('Ctrl Pts',(68.6216467656553,63.8722013716271,48.3030853894858));
#35733=CARTESIAN_POINT('Ctrl Pts',(67.3087010236203,64.0492979436258,50.0740804314643));
#35734=CARTESIAN_POINT('Ctrl Pts',(66.7849774198233,64.2263945156245,52.4087119996498));
#35735=CARTESIAN_POINT('Ctrl Pts',(67.2156126057623,64.4034910876233,54.5708413428834));
#35736=CARTESIAN_POINT('Ctrl Pts',(67.6462477917012,64.580587659622,56.7329706861169));
#35737=CARTESIAN_POINT('Ctrl Pts',(69.0245064208026,64.7576842316207,58.6887810357291));
#35738=CARTESIAN_POINT('Ctrl Pts',(70.9158061804535,64.9347808036194,59.821580744144));
#35739=CARTESIAN_POINT('Ctrl Pts',(72.8071059401044,65.1118773756181,60.9543804525588));
#35740=CARTESIAN_POINT('Ctrl Pts',(75.1818659698181,65.2889739476169,61.2464519739652));
#35741=CARTESIAN_POINT('Ctrl Pts',(77.2912945088739,65.4660705196156,60.6057014773933));
#35742=CARTESIAN_POINT('Ctrl Pts',(79.4007230479297,65.6431670916143,59.9649509808214));
#35743=CARTESIAN_POINT('Ctrl Pts',(81.2118275942126,65.820263663613,58.4014001198717));
#35744=CARTESIAN_POINT('Ctrl Pts',(82.153544063313,65.9973602356117,56.4080561826484));
#35745=CARTESIAN_POINT('Ctrl Pts',(82.6515697929936,66.091017564954,55.3538784110857));
#35746=CARTESIAN_POINT('Ctrl Pts',(82.9129498948704,66.1846748942963,54.1887099277235));
#35747=CARTESIAN_POINT('Ctrl Pts',(82.9129498948689,66.2783322236386,53.0228109606252));
#35748=CARTESIAN_POINT('Ctrl Pts',(82.9166465239286,67.7216677763615,53.0178513738214));
#35749=CARTESIAN_POINT('Ctrl Pts',(82.9116093512061,67.6590299543487,53.7969963792745));
#35750=CARTESIAN_POINT('Ctrl Pts',(82.7910644468045,67.596392132336,54.5778695919009));
#35751=CARTESIAN_POINT('Ctrl Pts',(82.5635267122257,67.5337543103233,55.3262109863277));
#35752=CARTESIAN_POINT('Ctrl Pts',(82.1781884593963,67.4276763055471,56.593537331042));
#35753=CARTESIAN_POINT('Ctrl Pts',(81.4859960123467,67.321598300771,57.7675627990191));
#35754=CARTESIAN_POINT('Ctrl Pts',(80.5452190389621,67.2155202959948,58.6870297166436));
#35755=CARTESIAN_POINT('Ctrl Pts',(78.6636650921934,67.0033642864425,60.5259635518921));
#35756=CARTESIAN_POINT('Ctrl Pts',(75.7877730400849,66.7912082768902,61.3466631857312));
#35757=CARTESIAN_POINT('Ctrl Pts',(73.2260023948809,66.5790522673379,60.7637464737497));
#35758=CARTESIAN_POINT('Ctrl Pts',(70.6642317496769,66.3668962577856,60.1808297617682));
#35759=CARTESIAN_POINT('Ctrl Pts',(68.4165825113773,66.1547402482333,58.194296703966));
#35760=CARTESIAN_POINT('Ctrl Pts',(67.5220058998071,65.942584238681,55.7217158256514));
#35761=CARTESIAN_POINT('Ctrl Pts',(66.6274292882369,65.7304282291287,53.2491349473366));
#35762=CARTESIAN_POINT('Ctrl Pts',(67.0859253033961,65.5182722195764,50.2905062485098));
#35763=CARTESIAN_POINT('Ctrl Pts',(68.6826220783526,65.3061162100241,48.2020864386379));
#35764=CARTESIAN_POINT('Ctrl Pts',(70.279318853309,65.0939602004718,46.113666628766));
#35765=CARTESIAN_POINT('Ctrl Pts',(73.0142163880631,64.8818041909194,44.8954557078497));
#35766=CARTESIAN_POINT('Ctrl Pts',(75.634848720819,64.6696481813671,45.1104201009277));
#35767=CARTESIAN_POINT('Ctrl Pts',(78.2554810535745,64.4574921718148,45.3253844940057));
#35768=CARTESIAN_POINT('Ctrl Pts',(80.7618481843323,64.2453361622624,46.9735242010776));
#35769=CARTESIAN_POINT('Ctrl Pts',(81.9960700343584,64.0331801527101,49.2928252071254));
#35770=CARTESIAN_POINT('Ctrl Pts',(82.6001465380191,63.9293426939273,50.4279819397991));
#35771=CARTESIAN_POINT('Ctrl Pts',(82.8994797620802,63.8255052351444,51.723915824649));
#35772=CARTESIAN_POINT('Ctrl Pts',(82.8974486171957,63.7216677763616,53.0207358597371));
#35773=CARTESIAN_POINT('Origin',(74.9879498948689,255.,53.0228109606356));
#35774=CARTESIAN_POINT('',(82.9163763150487,58.2783322236387,53.0223520988813));
#35775=CARTESIAN_POINT('',(82.9129498948689,59.7216677763615,53.0228109606378));
#35776=CARTESIAN_POINT('',(82.9129498948689,255.,53.0228109606356));
#35777=CARTESIAN_POINT('Ctrl Pts',(82.9129498948689,58.2783322236386,53.0228109606249));
#35778=CARTESIAN_POINT('Ctrl Pts',(82.9129498948659,58.4554287956374,50.8182135007149));
#35779=CARTESIAN_POINT('Ctrl Pts',(81.9432795991046,58.6325253676362,48.6308565362798));
#35780=CARTESIAN_POINT('Ctrl Pts',(80.309688270246,58.8096219396349,47.1504412801711));
#35781=CARTESIAN_POINT('Ctrl Pts',(78.6760969413874,58.9867185116336,45.6700260240623));
#35782=CARTESIAN_POINT('Ctrl Pts',(76.4041347530328,59.1638150836324,44.919706900601));
#35783=CARTESIAN_POINT('Ctrl Pts',(74.2101800112104,59.3409116556311,45.1360689838701));
#35784=CARTESIAN_POINT('Ctrl Pts',(72.0162252693881,59.5180082276298,45.3524310671393));
#35785=CARTESIAN_POINT('Ctrl Pts',(69.9345925076882,59.6951047996286,46.5320903475089));
#35786=CARTESIAN_POINT('Ctrl Pts',(68.6216467656536,59.8722013716274,48.3030853894881));
#35787=CARTESIAN_POINT('Ctrl Pts',(67.308701023619,60.0492979436261,50.0740804314673));
#35788=CARTESIAN_POINT('Ctrl Pts',(66.7849774198229,60.2263945156248,52.4087119996534));
#35789=CARTESIAN_POINT('Ctrl Pts',(67.215612605763,60.4034910876236,54.5708413428871));
#35790=CARTESIAN_POINT('Ctrl Pts',(67.6462477917031,60.5805876596223,56.7329706861207));
#35791=CARTESIAN_POINT('Ctrl Pts',(69.0245064208057,60.7576842316211,58.6887810357325));
#35792=CARTESIAN_POINT('Ctrl Pts',(70.9158061804575,60.9347808036198,59.8215807441464));
#35793=CARTESIAN_POINT('Ctrl Pts',(72.8071059401093,61.1118773756186,60.9543804525602));
#35794=CARTESIAN_POINT('Ctrl Pts',(75.1818659698236,61.2889739476173,61.2464519739651));
#35795=CARTESIAN_POINT('Ctrl Pts',(77.2912945088793,61.466070519616,60.6057014773917));
#35796=CARTESIAN_POINT('Ctrl Pts',(79.4007230479349,61.6431670916148,59.9649509808182));
#35797=CARTESIAN_POINT('Ctrl Pts',(81.2118275942168,61.8202636636135,58.4014001198669));
#35798=CARTESIAN_POINT('Ctrl Pts',(82.1535440633157,61.9973602356122,56.4080561826425));
#35799=CARTESIAN_POINT('Ctrl Pts',(82.6515697929946,62.0910175649543,55.3538784110813));
#35800=CARTESIAN_POINT('Ctrl Pts',(82.9129498948705,62.1846748942965,54.1887099277212));
#35801=CARTESIAN_POINT('Ctrl Pts',(82.9129498948689,62.2783322236386,53.022810960625));
#35802=CARTESIAN_POINT('Ctrl Pts',(82.9129498948689,63.7216677763616,53.0228109606371));
#35803=CARTESIAN_POINT('Ctrl Pts',(82.9129498948685,63.5445712043629,55.2274084205467));
#35804=CARTESIAN_POINT('Ctrl Pts',(81.94327959911,63.3674746323641,57.4147653849827));
#35805=CARTESIAN_POINT('Ctrl Pts',(80.3096882702535,63.1903780603654,58.8951806410933));
#35806=CARTESIAN_POINT('Ctrl Pts',(78.676096941397,63.0132814883667,60.3755958972039));
#35807=CARTESIAN_POINT('Ctrl Pts',(76.4041347530438,62.836184916368,61.1259150206681));
#35808=CARTESIAN_POINT('Ctrl Pts',(74.2101800112214,62.6590883443693,60.9095529374021));
#35809=CARTESIAN_POINT('Ctrl Pts',(72.016225269399,62.4819917723706,60.693190854136));
#35810=CARTESIAN_POINT('Ctrl Pts',(69.9345925076977,62.3048952003718,59.5135315737696));
#35811=CARTESIAN_POINT('Ctrl Pts',(68.6216467656607,62.1277986283731,57.7425365317926));
#35812=CARTESIAN_POINT('Ctrl Pts',(67.3087010236236,61.9507020563744,55.9715414898156));
#35813=CARTESIAN_POINT('Ctrl Pts',(66.784977419824,61.7736054843757,53.6369099216307));
#35814=CARTESIAN_POINT('Ctrl Pts',(67.2156126057605,61.596508912377,51.4747805783966));
#35815=CARTESIAN_POINT('Ctrl Pts',(67.646247791697,61.4194123403782,49.3126512351626));
#35816=CARTESIAN_POINT('Ctrl Pts',(69.0245064207961,61.2423157683795,47.3568408855488));
#35817=CARTESIAN_POINT('Ctrl Pts',(70.9158061804457,61.0652191963808,46.2240411771318));
#35818=CARTESIAN_POINT('Ctrl Pts',(72.8071059400953,60.888122624382,45.0912414687148));
#35819=CARTESIAN_POINT('Ctrl Pts',(75.1818659698088,60.7110260523834,44.7991699473058));
#35820=CARTESIAN_POINT('Ctrl Pts',(77.2912945088653,60.5339294803846,45.4399204438752));
#35821=CARTESIAN_POINT('Ctrl Pts',(79.4007230479218,60.3568329083859,46.0806709404447));
#35822=CARTESIAN_POINT('Ctrl Pts',(81.2118275942064,60.1797363363872,47.6442218013923));
#35823=CARTESIAN_POINT('Ctrl Pts',(82.1535440633091,60.0026397643884,49.6375657386146));
#35824=CARTESIAN_POINT('Ctrl Pts',(82.651569792991,59.9089824350462,50.6917435101767));
#35825=CARTESIAN_POINT('Ctrl Pts',(82.9129498948691,59.8153251057039,51.8569119935386));
#35826=CARTESIAN_POINT('Ctrl Pts',(82.9129498948689,59.7216677763616,53.0228109606369));
#35827=CARTESIAN_POINT('Origin',(74.9879498948689,255.,53.0228109606356));
#35828=CARTESIAN_POINT('',(82.9104010142055,54.2783322236387,53.0210824732343));
#35829=CARTESIAN_POINT('',(82.9171842364519,55.7216677763613,53.0215139011292));
#35830=CARTESIAN_POINT('',(82.9129498948689,255.,53.0228109606356));
#35831=CARTESIAN_POINT('Ctrl Pts',(82.904538510375,54.2783322236387,53.0171068991978));
#35832=CARTESIAN_POINT('Ctrl Pts',(82.9106802894969,54.3392274080026,52.2581622407597));
#35833=CARTESIAN_POINT('Ctrl Pts',(82.8107733365512,54.4001225923666,51.5005576736762));
#35834=CARTESIAN_POINT('Ctrl Pts',(82.5983352092591,54.4610177767305,50.7758908858849));
#35835=CARTESIAN_POINT('Ctrl Pts',(82.2282728978152,54.5670957815067,49.5135380778694));
#35836=CARTESIAN_POINT('Ctrl Pts',(81.5167365904301,54.6731737862828,48.351134418858));
#35837=CARTESIAN_POINT('Ctrl Pts',(80.5787412531064,54.779251791059,47.4158449555051));
#35838=CARTESIAN_POINT('Ctrl Pts',(79.6407459157828,54.8853297958351,46.4805554921522));
#35839=CARTESIAN_POINT('Ctrl Pts',(78.4762915485206,54.9914078006112,45.7723802244579));
#35840=CARTESIAN_POINT('Ctrl Pts',(77.2128749343213,55.0974858053874,45.4059662710925));
#35841=CARTESIAN_POINT('Ctrl Pts',(74.6860417059226,55.3096418149397,44.6731383643616));
#35842=CARTESIAN_POINT('Ctrl Pts',(71.7633594897756,55.5217978244921,45.3073557149463));
#35843=CARTESIAN_POINT('Ctrl Pts',(69.780233864638,55.7339538340444,47.0306297751755));
#35844=CARTESIAN_POINT('Ctrl Pts',(67.7971082395001,55.9461098435967,48.7539038354048));
#35845=CARTESIAN_POINT('Ctrl Pts',(66.7535392053719,56.158265853149,51.5662346052788));
#35846=CARTESIAN_POINT('Ctrl Pts',(67.1322283071543,56.3704218627014,54.1682565263949));
#35847=CARTESIAN_POINT('Ctrl Pts',(67.5109174089366,56.5825778722537,56.7702784475106));
#35848=CARTESIAN_POINT('Ctrl Pts',(69.3118646466293,56.794733881806,59.1619915198684));
#35849=CARTESIAN_POINT('Ctrl Pts',(71.7053648627521,57.0068898913583,60.2492332633831));
#35850=CARTESIAN_POINT('Ctrl Pts',(74.0988650788749,57.2190459009106,61.3364750068978));
#35851=CARTESIAN_POINT('Ctrl Pts',(77.0849182734277,57.4312019104629,61.1192454215695));
#35852=CARTESIAN_POINT('Ctrl Pts',(79.2936426408122,57.6433579200152,59.6925498749662));
#35853=CARTESIAN_POINT('Ctrl Pts',(81.4971833591665,57.855016021223,58.2692026361445));
#35854=CARTESIAN_POINT('Ctrl Pts',(82.9270395905761,58.0666741224308,55.6420597589509));
#35855=CARTESIAN_POINT('Ctrl Pts',(82.9268744173332,58.2783322236386,53.0209462066481));
#35856=CARTESIAN_POINT('Ctrl Pts',(82.9129498948689,59.7216677763616,53.0228109606369));
#35857=CARTESIAN_POINT('Ctrl Pts',(82.9129498948685,59.5445712043628,55.2274084205472));
#35858=CARTESIAN_POINT('Ctrl Pts',(81.9432795991095,59.367474632364,57.4147653849837));
#35859=CARTESIAN_POINT('Ctrl Pts',(80.3096882702523,59.1903780603653,58.8951806410944));
#35860=CARTESIAN_POINT('Ctrl Pts',(78.676096941395,59.0132814883665,60.3755958972051));
#35861=CARTESIAN_POINT('Ctrl Pts',(76.4041347530409,58.8361849163678,61.1259150206688));
#35862=CARTESIAN_POINT('Ctrl Pts',(74.210180011218,58.659088344369,60.9095529374017));
#35863=CARTESIAN_POINT('Ctrl Pts',(72.0162252693951,58.4819917723702,60.6931908541347));
#35864=CARTESIAN_POINT('Ctrl Pts',(69.9345925076938,58.3048952003714,59.5135315737667));
#35865=CARTESIAN_POINT('Ctrl Pts',(68.6216467656576,58.1277986283727,57.7425365317884));
#35866=CARTESIAN_POINT('Ctrl Pts',(67.3087010236213,57.9507020563739,55.9715414898101));
#35867=CARTESIAN_POINT('Ctrl Pts',(66.7849774198233,57.7736054843752,53.636909921624));
#35868=CARTESIAN_POINT('Ctrl Pts',(67.2156126057619,57.5965089123764,51.4747805783897));
#35869=CARTESIAN_POINT('Ctrl Pts',(67.6462477917004,57.4194123403776,49.3126512351555));
#35870=CARTESIAN_POINT('Ctrl Pts',(69.0245064208019,57.2423157683788,47.3568408855424));
#35871=CARTESIAN_POINT('Ctrl Pts',(70.9158061804533,57.0652191963801,46.2240411771273));
#35872=CARTESIAN_POINT('Ctrl Pts',(72.8071059401047,56.8881226243813,45.0912414687121));
#35873=CARTESIAN_POINT('Ctrl Pts',(75.1818659698192,56.7110260523826,44.7991699473058));
#35874=CARTESIAN_POINT('Ctrl Pts',(77.2912945088755,56.5339294803838,45.4399204438783));
#35875=CARTESIAN_POINT('Ctrl Pts',(79.4007230479317,56.356832908385,46.0806709404508));
#35876=CARTESIAN_POINT('Ctrl Pts',(81.2118275942146,56.1797363363862,47.6442218014015));
#35877=CARTESIAN_POINT('Ctrl Pts',(82.1535440633144,56.0026397643875,49.6375657386259));
#35878=CARTESIAN_POINT('Ctrl Pts',(82.6515697929931,55.9089824350455,50.6917435101855));
#35879=CARTESIAN_POINT('Ctrl Pts',(82.9129498948693,55.8153251057034,51.8569119935439));
#35880=CARTESIAN_POINT('Ctrl Pts',(82.9129498948689,55.7216677763614,53.0228109606385));
#35881=CARTESIAN_POINT('Origin',(74.9879498948689,255.,53.0228109606356));
#35882=CARTESIAN_POINT('',(82.9117139092691,50.2783322236387,53.0232455636512));
#35883=CARTESIAN_POINT('',(82.9045864038165,51.7216677763616,53.0169664367311));
#35884=CARTESIAN_POINT('',(82.9129498948689,255.,53.0228109606356));
#35885=CARTESIAN_POINT('Ctrl Pts',(82.9129498948689,50.2783322236387,53.0228109606245));
#35886=CARTESIAN_POINT('Ctrl Pts',(82.9129498948658,50.4554287956374,50.8182135007149));
#35887=CARTESIAN_POINT('Ctrl Pts',(81.9432795991047,50.6325253676361,48.6308565362801));
#35888=CARTESIAN_POINT('Ctrl Pts',(80.3096882702464,50.8096219396349,47.1504412801714));
#35889=CARTESIAN_POINT('Ctrl Pts',(78.6760969413881,50.9867185116336,45.6700260240628));
#35890=CARTESIAN_POINT('Ctrl Pts',(76.404134753034,51.1638150836323,44.9197069006013));
#35891=CARTESIAN_POINT('Ctrl Pts',(74.2101800112119,51.340911655631,45.13606898387));
#35892=CARTESIAN_POINT('Ctrl Pts',(72.0162252693898,51.5180082276297,45.3524310671387));
#35893=CARTESIAN_POINT('Ctrl Pts',(69.9345925076899,51.6951047996284,46.5320903475076));
#35894=CARTESIAN_POINT('Ctrl Pts',(68.621646765655,51.8722013716271,48.3030853894862));
#35895=CARTESIAN_POINT('Ctrl Pts',(67.3087010236201,52.0492979436258,50.0740804314648));
#35896=CARTESIAN_POINT('Ctrl Pts',(66.7849774198232,52.2263945156246,52.4087119996504));
#35897=CARTESIAN_POINT('Ctrl Pts',(67.2156126057624,52.4034910876233,54.5708413428839));
#35898=CARTESIAN_POINT('Ctrl Pts',(67.6462477917015,52.580587659622,56.7329706861174));
#35899=CARTESIAN_POINT('Ctrl Pts',(69.024506420803,52.7576842316207,58.6887810357295));
#35900=CARTESIAN_POINT('Ctrl Pts',(70.9158061804539,52.9347808036194,59.8215807441442));
#35901=CARTESIAN_POINT('Ctrl Pts',(72.8071059401049,53.1118773756182,60.9543804525589));
#35902=CARTESIAN_POINT('Ctrl Pts',(75.1818659698187,53.2889739476169,61.2464519739651));
#35903=CARTESIAN_POINT('Ctrl Pts',(77.2912945088744,53.4660705196156,60.6057014773931));
#35904=CARTESIAN_POINT('Ctrl Pts',(79.4007230479302,53.6431670916144,59.9649509808211));
#35905=CARTESIAN_POINT('Ctrl Pts',(81.2118275942129,53.820263663613,58.4014001198713));
#35906=CARTESIAN_POINT('Ctrl Pts',(82.1535440633132,53.9973602356118,56.4080561826479));
#35907=CARTESIAN_POINT('Ctrl Pts',(82.6515697929938,54.091017564954,55.3538784110852));
#35908=CARTESIAN_POINT('Ctrl Pts',(82.9129498948705,54.1846748942964,54.188709927723));
#35909=CARTESIAN_POINT('Ctrl Pts',(82.9129498948689,54.2783322236387,53.0228109606247));
#35910=CARTESIAN_POINT('Ctrl Pts',(82.9253894869644,55.7216677763615,53.01900047654));
#35911=CARTESIAN_POINT('Ctrl Pts',(82.9135514667677,55.5219877680786,55.495166293122));
#35912=CARTESIAN_POINT('Ctrl Pts',(81.661333110683,55.3223077597958,57.983619928366));
#35913=CARTESIAN_POINT('Ctrl Pts',(79.6626107189349,55.1226277515129,59.4395147710704));
#35914=CARTESIAN_POINT('Ctrl Pts',(77.5390082086855,54.9104717419606,60.9863738823661));
#35915=CARTESIAN_POINT('Ctrl Pts',(74.5727043979174,54.6983157324083,61.3676148646698));
#35916=CARTESIAN_POINT('Ctrl Pts',(72.1180247786696,54.486159722856,60.420793407439));
#35917=CARTESIAN_POINT('Ctrl Pts',(70.8906849690454,54.3800817180798,59.9473826788236));
#35918=CARTESIAN_POINT('Ctrl Pts',(69.7912512073013,54.2740037133036,59.1419563403243));
#35919=CARTESIAN_POINT('Ctrl Pts',(68.9369188167712,54.1679257085274,58.1296728822003));
#35920=CARTESIAN_POINT('Ctrl Pts',(68.0825864262412,54.0618477037513,57.1173894240764));
#35921=CARTESIAN_POINT('Ctrl Pts',(67.473355406925,53.9557696989751,55.8982488463278));
#35922=CARTESIAN_POINT('Ctrl Pts',(67.2129117490884,53.849691694199,54.6088110512604));
#35923=CARTESIAN_POINT('Ctrl Pts',(66.6920244334152,53.6375356846467,52.0299354611254));
#35924=CARTESIAN_POINT('Ctrl Pts',(67.5662865636604,53.4253796750944,49.1698710017148));
#35925=CARTESIAN_POINT('Ctrl Pts',(69.4479899286966,53.2132236655421,47.3363898379861));
#35926=CARTESIAN_POINT('Ctrl Pts',(71.3296932937327,53.0010676559898,45.5029086742575));
#35927=CARTESIAN_POINT('Ctrl Pts',(74.2188378935599,52.7889116464374,44.6960108062107));
#35928=CARTESIAN_POINT('Ctrl Pts',(76.7805229565297,52.5767556368851,45.2890480326417));
#35929=CARTESIAN_POINT('Ctrl Pts',(79.3422080194998,52.3645996273328,45.8820852590727));
#35930=CARTESIAN_POINT('Ctrl Pts',(81.5764335456124,52.1524436177805,47.8750575799819));
#35931=CARTESIAN_POINT('Ctrl Pts',(82.4615658042492,51.9402876082282,50.3504320522876));
#35932=CARTESIAN_POINT('Ctrl Pts',(82.7655990892693,51.8674143309393,51.2006962078717));
#35933=CARTESIAN_POINT('Ctrl Pts',(82.9104599242351,51.7945410536505,52.1078764671829));
#35934=CARTESIAN_POINT('Ctrl Pts',(82.9045864038165,51.7216677763616,53.0169664367311));
#35935=CARTESIAN_POINT('Origin',(74.9879498948689,255.,53.0228109606356));
#35936=CARTESIAN_POINT('',(82.9132360241053,46.278332223639,53.0234054380586));
#35937=CARTESIAN_POINT('',(82.9030927965636,47.7216677763615,53.0278642989338));
#35938=CARTESIAN_POINT('',(82.9129498948689,255.,53.0228109606356));
#35939=CARTESIAN_POINT('Ctrl Pts',(82.9156681820723,46.2783322236388,53.0284586201259));
#35940=CARTESIAN_POINT('Ctrl Pts',(82.8956280895017,46.4600219600416,50.7712696112924));
#35941=CARTESIAN_POINT('Ctrl Pts',(81.8908844774418,46.6417116964444,48.5021875442689));
#35942=CARTESIAN_POINT('Ctrl Pts',(80.1917817852738,46.8234014328472,47.0272563351391));
#35943=CARTESIAN_POINT('Ctrl Pts',(78.2077685210858,47.0355574423995,45.3050042922422));
#35944=CARTESIAN_POINT('Ctrl Pts',(75.2770081084107,47.2477134519518,44.6655638402333));
#35945=CARTESIAN_POINT('Ctrl Pts',(72.7536601184849,47.4598694615041,45.4049138490338));
#35946=CARTESIAN_POINT('Ctrl Pts',(70.2303121285595,47.6720254710564,46.1442638578342));
#35947=CARTESIAN_POINT('Ctrl Pts',(68.1143765613833,47.8841814806087,48.2624043274435));
#35948=CARTESIAN_POINT('Ctrl Pts',(67.3730398495798,48.0963374901609,50.784577551699));
#35949=CARTESIAN_POINT('Ctrl Pts',(66.631703137776,48.3084934997133,53.3067507759554));
#35950=CARTESIAN_POINT('Ctrl Pts',(67.264965281346,48.5206495092656,56.2329567548582));
#35951=CARTESIAN_POINT('Ctrl Pts',(68.9869159785598,48.732805518818,58.2201178731734));
#35952=CARTESIAN_POINT('Ctrl Pts',(70.7088666757733,48.9449615283703,60.2072789914881));
#35953=CARTESIAN_POINT('Ctrl Pts',(73.5195059266301,49.1571175379227,61.2553952492156));
#35954=CARTESIAN_POINT('Ctrl Pts',(76.119892113975,49.369273547475,60.8806254419981));
#35955=CARTESIAN_POINT('Ctrl Pts',(78.72027830132,49.5814295570273,60.5058556347807));
#35956=CARTESIAN_POINT('Ctrl Pts',(81.1104114251532,49.7935855665796,58.7081997626184));
#35957=CARTESIAN_POINT('Ctrl Pts',(82.2071389034964,50.0057415761319,56.3167333206063));
#35958=CARTESIAN_POINT('Ctrl Pts',(82.6768524476174,50.0966051253008,55.2925005915961));
#35959=CARTESIAN_POINT('Ctrl Pts',(82.9093174951633,50.1874686744697,54.1593456034027));
#35960=CARTESIAN_POINT('Ctrl Pts',(82.9067025264445,50.2783322236387,53.0250076894748));
#35961=CARTESIAN_POINT('Ctrl Pts',(82.9045864038165,51.7216677763616,53.0169664367311));
#35962=CARTESIAN_POINT('Ctrl Pts',(82.8933603412276,51.5823850440982,54.7545105618576));
#35963=CARTESIAN_POINT('Ctrl Pts',(82.3314911796438,51.4431023118347,56.4990309914926));
#35964=CARTESIAN_POINT('Ctrl Pts',(81.2778946571288,51.3038195795713,57.8664668211942));
#35965=CARTESIAN_POINT('Ctrl Pts',(79.6730522602106,51.0916635700189,59.9493504940937));
#35966=CARTESIAN_POINT('Ctrl Pts',(76.9273284752132,50.8795075604666,61.1573412161903));
#35967=CARTESIAN_POINT('Ctrl Pts',(74.3096956074956,50.6673515509142,60.9327106270388));
#35968=CARTESIAN_POINT('Ctrl Pts',(71.6920627397786,50.4551955413619,60.7080800378874));
#35969=CARTESIAN_POINT('Ctrl Pts',(69.2025207893409,50.2430395318095,59.050828137488));
#35970=CARTESIAN_POINT('Ctrl Pts',(67.9701012205266,50.0308835222573,56.7263787593717));
#35971=CARTESIAN_POINT('Ctrl Pts',(67.3538914361195,49.9248055174811,55.5641540703134));
#35972=CARTESIAN_POINT('Ctrl Pts',(67.0519622471181,49.818727512705,54.2351300118258));
#35973=CARTESIAN_POINT('Ctrl Pts',(67.0707259166118,49.7126495079289,52.9106491483147));
#35974=CARTESIAN_POINT('Ctrl Pts',(67.0894895861055,49.6065715031527,51.5861682848033));
#35975=CARTESIAN_POINT('Ctrl Pts',(67.4289461140944,49.5004934983765,50.2662306162687));
#35976=CARTESIAN_POINT('Ctrl Pts',(68.0778320296788,49.3944154936003,49.1219282983418));
#35977=CARTESIAN_POINT('Ctrl Pts',(69.3756038608473,49.182259484048,46.8333236624885));
#35978=CARTESIAN_POINT('Ctrl Pts',(71.9110932423966,48.9701034744957,45.2472604290661));
#35979=CARTESIAN_POINT('Ctrl Pts',(74.5340389317533,48.7579474649434,45.0968721235974));
#35980=CARTESIAN_POINT('Ctrl Pts',(77.1569846211103,48.5457914553911,44.9464838181288));
#35981=CARTESIAN_POINT('Ctrl Pts',(79.8673866182743,48.3336354458388,46.2317704406142));
#35982=CARTESIAN_POINT('Ctrl Pts',(81.4125811705769,48.1214794362864,48.3592800902543));
#35983=CARTESIAN_POINT('Ctrl Pts',(82.3832297672811,47.9882088829781,49.6957229691272));
#35984=CARTESIAN_POINT('Ctrl Pts',(82.8940868239913,47.8549383296698,51.3645075476531));
#35985=CARTESIAN_POINT('Ctrl Pts',(82.9030927965636,47.7216677763615,53.0278642989338));
#35986=CARTESIAN_POINT('Origin',(74.9879498948689,255.,53.0228109606356));
#35987=CARTESIAN_POINT('',(82.9147244314983,42.2783322236387,53.0216046455403));
#35988=CARTESIAN_POINT('',(82.9169881471838,43.7216677763615,53.0246207943705));
#35989=CARTESIAN_POINT('',(82.9129498948689,255.,53.0228109606356));
#35990=CARTESIAN_POINT('Ctrl Pts',(82.9129498948689,42.2783322236387,53.0228109606242));
#35991=CARTESIAN_POINT('Ctrl Pts',(82.9129498948657,42.4554287956375,50.8182135007139));
#35992=CARTESIAN_POINT('Ctrl Pts',(81.9432795991039,42.6325253676363,48.6308565362786));
#35993=CARTESIAN_POINT('Ctrl Pts',(80.3096882702448,42.809621939635,47.15044128017));
#35994=CARTESIAN_POINT('Ctrl Pts',(78.6760969413857,42.9867185116338,45.6700260240614));
#35995=CARTESIAN_POINT('Ctrl Pts',(76.4041347530306,43.1638150836325,44.9197069006005));
#35996=CARTESIAN_POINT('Ctrl Pts',(74.210180011208,43.3409116556313,45.1360689838704));
#35997=CARTESIAN_POINT('Ctrl Pts',(72.0162252693853,43.5180082276301,45.3524310671402));
#35998=CARTESIAN_POINT('Ctrl Pts',(69.9345925076856,43.6951047996289,46.5320903475108));
#35999=CARTESIAN_POINT('Ctrl Pts',(68.6216467656516,43.8722013716276,48.3030853894908));
#36000=CARTESIAN_POINT('Ctrl Pts',(67.3087010236176,44.0492979436264,50.0740804314708));
#36001=CARTESIAN_POINT('Ctrl Pts',(66.7849774198225,44.2263945156251,52.4087119996576));
#36002=CARTESIAN_POINT('Ctrl Pts',(67.2156126057638,44.4034910876239,54.5708413428913));
#36003=CARTESIAN_POINT('Ctrl Pts',(67.6462477917051,44.5805876596227,56.732970686125));
#36004=CARTESIAN_POINT('Ctrl Pts',(69.0245064208091,44.7576842316215,58.6887810357363));
#36005=CARTESIAN_POINT('Ctrl Pts',(70.9158061804619,44.9347808036202,59.821580744149));
#36006=CARTESIAN_POINT('Ctrl Pts',(72.8071059401148,45.111877375619,60.9543804525618));
#36007=CARTESIAN_POINT('Ctrl Pts',(75.1818659698297,45.2889739476177,61.246451973965));
#36008=CARTESIAN_POINT('Ctrl Pts',(77.2912945088851,45.4660705196165,60.6057014773899));
#36009=CARTESIAN_POINT('Ctrl Pts',(79.4007230479405,45.6431670916153,59.9649509808147));
#36010=CARTESIAN_POINT('Ctrl Pts',(81.2118275942214,45.8202636636141,58.4014001198617));
#36011=CARTESIAN_POINT('Ctrl Pts',(82.1535440633187,45.9973602356128,56.4080561826362));
#36012=CARTESIAN_POINT('Ctrl Pts',(82.6515697929959,46.0910175649548,55.3538784110762));
#36013=CARTESIAN_POINT('Ctrl Pts',(82.9129498948707,46.1846748942968,54.1887099277178));
#36014=CARTESIAN_POINT('Ctrl Pts',(82.9129498948689,46.2783322236388,53.0228109606235));
#36015=CARTESIAN_POINT('Ctrl Pts',(82.9030927965636,47.7216677763615,53.0278642989338));
#36016=CARTESIAN_POINT('Ctrl Pts',(82.9084236084921,47.6427823201175,54.0124378072146));
#36017=CARTESIAN_POINT('Ctrl Pts',(82.7379214356189,47.5638968638735,54.9951095739316));
#36018=CARTESIAN_POINT('Ctrl Pts',(82.3828635408296,47.4850114076295,55.9058295106122));
#36019=CARTESIAN_POINT('Ctrl Pts',(81.4279642513385,47.2728553980772,58.3551366045373));
#36020=CARTESIAN_POINT('Ctrl Pts',(79.1381785649148,47.0606993885249,60.2840181155929));
#36021=CARTESIAN_POINT('Ctrl Pts',(76.5607220279737,46.8485433789726,60.8042500964981));
#36022=CARTESIAN_POINT('Ctrl Pts',(73.9832654910329,46.6363873694202,61.3244820774033));
#36023=CARTESIAN_POINT('Ctrl Pts',(71.1181381035746,46.424231359868,60.4360645281585));
#36024=CARTESIAN_POINT('Ctrl Pts',(69.2891286337702,46.2120753503157,58.550014398628));
#36025=CARTESIAN_POINT('Ctrl Pts',(67.4601191639658,45.9999193407634,56.6639642690976));
#36026=CARTESIAN_POINT('Ctrl Pts',(66.6672276118151,45.787763331211,53.7802815592815));
#36027=CARTESIAN_POINT('Ctrl Pts',(67.2609601088651,45.5756073216587,51.2171965768882));
#36028=CARTESIAN_POINT('Ctrl Pts',(67.5578263573901,45.4695293168826,49.9356540856916));
#36029=CARTESIAN_POINT('Ctrl Pts',(68.2013486182152,45.3634513121065,48.7342610263506));
#36030=CARTESIAN_POINT('Ctrl Pts',(69.0840140518336,45.2573733073303,47.7465852873577));
#36031=CARTESIAN_POINT('Ctrl Pts',(69.9666794854519,45.1512953025541,46.7589095483649));
#36032=CARTESIAN_POINT('Ctrl Pts',(71.0884880918636,45.045217297778,45.9849511297201));
#36033=CARTESIAN_POINT('Ctrl Pts',(72.3287460984796,44.9391392930018,45.5464983919242));
#36034=CARTESIAN_POINT('Ctrl Pts',(74.8092621117119,44.7269832834495,44.6695929163322));
#36035=CARTESIAN_POINT('Ctrl Pts',(77.763575725762,44.5148272738971,45.1347101641362));
#36036=CARTESIAN_POINT('Ctrl Pts',(79.8425066737505,44.3026712643448,46.7411057708388));
#36037=CARTESIAN_POINT('Ctrl Pts',(81.7402707053649,44.109003435017,48.2075132077443));
#36038=CARTESIAN_POINT('Ctrl Pts',(82.9085734707273,43.9153356056892,50.6249542772596));
#36039=CARTESIAN_POINT('Ctrl Pts',(82.9240047689655,43.7216677763615,53.0277654514659));
#36040=CARTESIAN_POINT('Origin',(74.9879498948689,255.,53.0228109606356));
#36041=CARTESIAN_POINT('',(82.9091845765454,38.2783322236387,53.0220737411109));
#36042=CARTESIAN_POINT('',(82.9140883333191,39.7216677763616,53.0196810260503));
#36043=CARTESIAN_POINT('',(82.9129498948689,255.,53.0228109606356));
#36044=CARTESIAN_POINT('Ctrl Pts',(82.9008833462252,38.2783322236387,53.0204484259995));
#36045=CARTESIAN_POINT('Ctrl Pts',(82.9050287911047,38.3686605025281,51.8911974838658));
#36046=CARTESIAN_POINT('Ctrl Pts',(82.6800224357425,38.4589887814175,50.763391042182));
#36047=CARTESIAN_POINT('Ctrl Pts',(82.2178821027084,38.5493170603068,49.7437123836101));
#36048=CARTESIAN_POINT('Ctrl Pts',(81.1324429676421,38.7614730698592,47.3487707563791));
#36049=CARTESIAN_POINT('Ctrl Pts',(78.7388555001831,38.9736290794115,45.5503154722348));
#36050=CARTESIAN_POINT('Ctrl Pts',(76.1377185459513,39.1857850889638,45.1694947286408));
#36051=CARTESIAN_POINT('Ctrl Pts',(73.5365815917197,39.3979410985161,44.7886739850468));
#36052=CARTESIAN_POINT('Ctrl Pts',(70.7278951507152,39.6100971080685,45.8254877820027));
#36053=CARTESIAN_POINT('Ctrl Pts',(69.0014620556514,39.8222531176208,47.8087558632373));
#36054=CARTESIAN_POINT('Ctrl Pts',(67.2750289605875,40.0344091271731,49.7920239444719));
#36055=CARTESIAN_POINT('Ctrl Pts',(66.6308492114644,40.2465651367254,52.7217463099852));
#36056=CARTESIAN_POINT('Ctrl Pts',(67.3660894765719,40.4587211462777,55.2440235517453));
#36057=CARTESIAN_POINT('Ctrl Pts',(68.1013297416796,40.67087715583,57.7663007935056));
#36058=CARTESIAN_POINT('Ctrl Pts',(70.2159900210182,40.8830331653824,59.8811329115127));
#36059=CARTESIAN_POINT('Ctrl Pts',(72.7374779153666,41.0951891749347,60.6321466954601));
#36060=CARTESIAN_POINT('Ctrl Pts',(73.9982218625407,41.2012671797108,61.0076535874338));
#36061=CARTESIAN_POINT('Ctrl Pts',(75.3606727134672,41.3073451844869,61.0422058958927));
#36062=CARTESIAN_POINT('Ctrl Pts',(76.6555752005181,41.4134231892631,60.7632270756768));
#36063=CARTESIAN_POINT('Ctrl Pts',(77.9504776875691,41.5195011940392,60.4842482554609));
#36064=CARTESIAN_POINT('Ctrl Pts',(79.1778318107445,41.6255791988154,59.8917383065703));
#36065=CARTESIAN_POINT('Ctrl Pts',(80.1721053878536,41.7316572035916,59.0304016824108));
#36066=CARTESIAN_POINT('Ctrl Pts',(81.880107999848,41.913882210274,57.5507634442628));
#36067=CARTESIAN_POINT('Ctrl Pts',(82.9002961680271,42.0961072169563,55.2778248931831));
#36068=CARTESIAN_POINT('Ctrl Pts',(82.9205917520382,42.2783322236387,53.017616090358));
#36069=CARTESIAN_POINT('Ctrl Pts',(82.9129498948689,43.7216677763615,53.0228109606371));
#36070=CARTESIAN_POINT('Ctrl Pts',(82.9129498948685,43.5445712043628,55.2274084205465));
#36071=CARTESIAN_POINT('Ctrl Pts',(81.9432795991102,43.3674746323642,57.4147653849821));
#36072=CARTESIAN_POINT('Ctrl Pts',(80.3096882702541,43.1903780603655,58.8951806410927));
#36073=CARTESIAN_POINT('Ctrl Pts',(78.676096941398,43.0132814883668,60.3755958972033));
#36074=CARTESIAN_POINT('Ctrl Pts',(76.4041347530453,42.8361849163681,61.1259150206678));
#36075=CARTESIAN_POINT('Ctrl Pts',(74.2101800112232,42.6590883443694,60.9095529374023));
#36076=CARTESIAN_POINT('Ctrl Pts',(72.016225269401,42.4819917723707,60.6931908541367));
#36077=CARTESIAN_POINT('Ctrl Pts',(69.9345925076997,42.304895200372,59.513531573771));
#36078=CARTESIAN_POINT('Ctrl Pts',(68.6216467656623,42.1277986283733,57.7425365317947));
#36079=CARTESIAN_POINT('Ctrl Pts',(67.3087010236248,41.9507020563746,55.9715414898185));
#36080=CARTESIAN_POINT('Ctrl Pts',(66.7849774198243,41.7736054843759,53.6369099216341));
#36081=CARTESIAN_POINT('Ctrl Pts',(67.2156126057598,41.5965089123772,51.4747805784001));
#36082=CARTESIAN_POINT('Ctrl Pts',(67.6462477916953,41.4194123403785,49.3126512351662));
#36083=CARTESIAN_POINT('Ctrl Pts',(69.0245064207932,41.2423157683798,47.356840885552));
#36084=CARTESIAN_POINT('Ctrl Pts',(70.9158061804419,41.0652191963811,46.2240411771341));
#36085=CARTESIAN_POINT('Ctrl Pts',(72.8071059400906,40.8881226243824,45.0912414687162));
#36086=CARTESIAN_POINT('Ctrl Pts',(75.1818659698035,40.7110260523838,44.7991699473057));
#36087=CARTESIAN_POINT('Ctrl Pts',(77.2912945088602,40.5339294803851,45.4399204438737));
#36088=CARTESIAN_POINT('Ctrl Pts',(79.4007230479168,40.3568329083864,46.0806709404416));
#36089=CARTESIAN_POINT('Ctrl Pts',(81.2118275942023,40.1797363363876,47.6442218013876));
#36090=CARTESIAN_POINT('Ctrl Pts',(82.1535440633064,40.0026397643889,49.6375657386089));
#36091=CARTESIAN_POINT('Ctrl Pts',(82.65156979299,39.9089824350465,50.6917435101726));
#36092=CARTESIAN_POINT('Ctrl Pts',(82.9129498948691,39.815325105704,51.8569119935366));
#36093=CARTESIAN_POINT('Ctrl Pts',(82.9129498948689,39.7216677763615,53.0228109606369));
#36094=CARTESIAN_POINT('Origin',(74.9879498948689,255.,53.0228109606356));
#36095=CARTESIAN_POINT('',(82.9122935305125,34.2783322236387,53.0239510175697));
#36096=CARTESIAN_POINT('',(82.9072011753408,35.7216677763615,53.0231373687424));
#36097=CARTESIAN_POINT('',(82.9129498948689,255.,53.0228109606356));
#36098=CARTESIAN_POINT('Ctrl Pts',(82.9129498948689,34.2783322236387,53.0228109606238));
#36099=CARTESIAN_POINT('Ctrl Pts',(82.9129498948656,34.4554287956374,50.8182135007142));
#36100=CARTESIAN_POINT('Ctrl Pts',(81.9432795991043,34.6325253676362,48.6308565362795));
#36101=CARTESIAN_POINT('Ctrl Pts',(80.3096882702459,34.8096219396349,47.150441280171));
#36102=CARTESIAN_POINT('Ctrl Pts',(78.6760969413875,34.9867185116336,45.6700260240625));
#36103=CARTESIAN_POINT('Ctrl Pts',(76.4041347530333,35.1638150836323,44.9197069006012));
#36104=CARTESIAN_POINT('Ctrl Pts',(74.2101800112112,35.340911655631,45.1360689838701));
#36105=CARTESIAN_POINT('Ctrl Pts',(72.0162252693891,35.5180082276298,45.352431067139));
#36106=CARTESIAN_POINT('Ctrl Pts',(69.9345925076894,35.6951047996285,46.5320903475081));
#36107=CARTESIAN_POINT('Ctrl Pts',(68.6216467656546,35.8722013716272,48.3030853894867));
#36108=CARTESIAN_POINT('Ctrl Pts',(67.3087010236198,36.0492979436259,50.0740804314654));
#36109=CARTESIAN_POINT('Ctrl Pts',(66.7849774198232,36.2263945156246,52.4087119996511));
#36110=CARTESIAN_POINT('Ctrl Pts',(67.2156126057625,36.4034910876234,54.5708413428845));
#36111=CARTESIAN_POINT('Ctrl Pts',(67.6462477917018,36.5805876596221,56.732970686118));
#36112=CARTESIAN_POINT('Ctrl Pts',(69.0245064208034,36.7576842316208,58.6887810357301));
#36113=CARTESIAN_POINT('Ctrl Pts',(70.9158061804545,36.9347808036195,59.8215807441446));
#36114=CARTESIAN_POINT('Ctrl Pts',(72.8071059401056,37.1118773756182,60.9543804525591));
#36115=CARTESIAN_POINT('Ctrl Pts',(75.1818659698194,37.288973947617,61.2464519739651));
#36116=CARTESIAN_POINT('Ctrl Pts',(77.2912945088751,37.4660705196157,60.6057014773929));
#36117=CARTESIAN_POINT('Ctrl Pts',(79.4007230479308,37.6431670916144,59.9649509808207));
#36118=CARTESIAN_POINT('Ctrl Pts',(81.2118275942134,37.8202636636131,58.4014001198708));
#36119=CARTESIAN_POINT('Ctrl Pts',(82.1535440633135,37.9973602356118,56.4080561826473));
#36120=CARTESIAN_POINT('Ctrl Pts',(82.651569792994,38.0910175649541,55.3538784110845));
#36121=CARTESIAN_POINT('Ctrl Pts',(82.9129498948706,38.1846748942964,54.1887099277223));
#36122=CARTESIAN_POINT('Ctrl Pts',(82.9129498948689,38.2783322236387,53.022810960624));
#36123=CARTESIAN_POINT('Ctrl Pts',(82.9163423979736,39.7216677763616,53.0134838750938));
#36124=CARTESIAN_POINT('Ctrl Pts',(82.8967122734635,39.5514208626041,55.1304071046395));
#36125=CARTESIAN_POINT('Ctrl Pts',(82.0220163137799,39.3811739488467,57.264215047829));
#36126=CARTESIAN_POINT('Ctrl Pts',(80.5052432378788,39.2109270350893,58.731040228542));
#36127=CARTESIAN_POINT('Ctrl Pts',(78.6150913633022,38.998771025537,60.5589487067788));
#36128=CARTESIAN_POINT('Ctrl Pts',(75.7278379817599,38.7866150159847,61.3510789260064));
#36129=CARTESIAN_POINT('Ctrl Pts',(73.1689413445864,38.5744590064323,60.7485958194524));
#36130=CARTESIAN_POINT('Ctrl Pts',(70.610044707413,38.36230299688,60.1461127128985));
#36131=CARTESIAN_POINT('Ctrl Pts',(68.3795048146082,38.1501469873277,58.1490162805631));
#36132=CARTESIAN_POINT('Ctrl Pts',(67.5034469430443,37.9379909777754,55.6698135620572));
#36133=CARTESIAN_POINT('Ctrl Pts',(66.6273890714801,37.725834968223,53.1906108435509));
#36134=CARTESIAN_POINT('Ctrl Pts',(67.1058132211573,37.5136789586706,50.2293018388738));
#36135=CARTESIAN_POINT('Ctrl Pts',(68.7171389828885,37.3015229491183,48.1541897885691));
#36136=CARTESIAN_POINT('Ctrl Pts',(70.3284647446191,37.089366939566,46.079077738265));
#36137=CARTESIAN_POINT('Ctrl Pts',(73.0726921184028,36.8772109300138,44.8901626423325));
#36138=CARTESIAN_POINT('Ctrl Pts',(75.6936668597371,36.6650549204615,45.1191043604828));
#36139=CARTESIAN_POINT('Ctrl Pts',(77.0041542304044,36.5589769156853,45.2335752195579));
#36140=CARTESIAN_POINT('Ctrl Pts',(78.2838284429594,36.4528989109092,45.7025102821538));
#36141=CARTESIAN_POINT('Ctrl Pts',(79.3853815208773,36.346820906133,46.4381613200989));
#36142=CARTESIAN_POINT('Ctrl Pts',(80.4869345987952,36.2407429013569,47.1738123580439));
#36143=CARTESIAN_POINT('Ctrl Pts',(81.410366542076,36.1346648965807,48.1761793713381));
#36144=CARTESIAN_POINT('Ctrl Pts',(82.0181869354863,36.0285868918046,49.3428134594782));
#36145=CARTESIAN_POINT('Ctrl Pts',(82.6043961057642,35.9262805199903,50.4679675481548));
#36146=CARTESIAN_POINT('Ctrl Pts',(82.8970380499207,35.8239741481759,51.7459152514041));
#36147=CARTESIAN_POINT('Ctrl Pts',(82.8972143917247,35.7216677763616,53.0237044110371));
#36148=CARTESIAN_POINT('Origin',(74.9879498948689,255.,53.0228109606356));
#36149=CARTESIAN_POINT('',(82.9249771640168,30.2783322236387,53.0230473193048));
#36150=CARTESIAN_POINT('',(82.9129498948689,31.7216677763616,53.0228109606366));
#36151=CARTESIAN_POINT('',(82.9129498948689,255.,53.0228109606356));
#36152=CARTESIAN_POINT('Ctrl Pts',(82.9249771640168,30.2783322236387,53.0230473193048));
#36153=CARTESIAN_POINT('Ctrl Pts',(82.9238427714935,30.489455054567,50.4069753398425));
#36154=CARTESIAN_POINT('Ctrl Pts',(81.5070197109814,30.7005778854952,47.7898361564491));
#36155=CARTESIAN_POINT('Ctrl Pts',(79.3122628451038,30.9117007164234,46.3651293279602));
#36156=CARTESIAN_POINT('Ctrl Pts',(77.1067654265869,31.1238567259758,44.9334503655986));
#36157=CARTESIAN_POINT('Ctrl Pts',(74.115701572633,31.3360127355282,44.7059032047884));
#36158=CARTESIAN_POINT('Ctrl Pts',(71.7212446046575,31.5481687450805,45.7871231457241));
#36159=CARTESIAN_POINT('Ctrl Pts',(69.3267876366829,31.7603247546328,46.8683430866595));
#36160=CARTESIAN_POINT('Ctrl Pts',(67.5289375546867,31.972480764185,49.2583301293398));
#36161=CARTESIAN_POINT('Ctrl Pts',(67.1384391261447,32.1846367737373,51.8601437049917));
#36162=CARTESIAN_POINT('Ctrl Pts',(66.9431899118737,32.2907147785135,53.1610504928182));
#36163=CARTESIAN_POINT('Ctrl Pts',(67.0997786109667,32.3967927832898,54.5149139138883));
#36164=CARTESIAN_POINT('Ctrl Pts',(67.5573491443184,32.5028707880659,55.7579870574282));
#36165=CARTESIAN_POINT('Ctrl Pts',(68.01491967767,32.6089487928421,57.0010602009678));
#36166=CARTESIAN_POINT('Ctrl Pts',(68.7734720452802,32.7150267976183,58.1333430669779));
#36167=CARTESIAN_POINT('Ctrl Pts',(69.7655608529922,32.8211048023944,58.9971952093159));
#36168=CARTESIAN_POINT('Ctrl Pts',(71.7497384684161,33.0332608119467,60.7248994939919));
#36169=CARTESIAN_POINT('Ctrl Pts',(74.6680618442466,33.245416821499,61.3788808839789));
#36170=CARTESIAN_POINT('Ctrl Pts',(77.1920771926515,33.4575728310514,60.6496297251194));
#36171=CARTESIAN_POINT('Ctrl Pts',(79.7160925410564,33.6697288406037,59.9203785662599));
#36172=CARTESIAN_POINT('Ctrl Pts',(81.8457998620355,33.881884850156,57.8078948585541));
#36173=CARTESIAN_POINT('Ctrl Pts',(82.5967259301963,34.0940408597083,55.2879675671467));
#36174=CARTESIAN_POINT('Ctrl Pts',(82.8141589874456,34.1554713143518,54.5583145184003));
#36175=CARTESIAN_POINT('Ctrl Pts',(82.9159935570133,34.2169017689953,53.7945009659517));
#36176=CARTESIAN_POINT('Ctrl Pts',(82.9093304898678,34.2783322236387,53.0290976027477));
#36177=CARTESIAN_POINT('Ctrl Pts',(82.9129498948689,35.7216677763615,53.0228109606377));
#36178=CARTESIAN_POINT('Ctrl Pts',(82.9129498948683,35.5445712043628,55.2274084205473));
#36179=CARTESIAN_POINT('Ctrl Pts',(81.9432795991096,35.3674746323641,57.4147653849832));
#36180=CARTESIAN_POINT('Ctrl Pts',(80.309688270253,35.1903780603654,58.8951806410937));
#36181=CARTESIAN_POINT('Ctrl Pts',(78.6760969413964,35.0132814883666,60.3755958972042));
#36182=CARTESIAN_POINT('Ctrl Pts',(76.4041347530432,34.836184916368,61.1259150206682));
#36183=CARTESIAN_POINT('Ctrl Pts',(74.2101800112208,34.6590883443692,60.909552937402));
#36184=CARTESIAN_POINT('Ctrl Pts',(72.0162252693984,34.4819917723705,60.6931908541358));
#36185=CARTESIAN_POINT('Ctrl Pts',(69.9345925076972,34.3048952003718,59.5135315737692));
#36186=CARTESIAN_POINT('Ctrl Pts',(68.6216467656603,34.127798628373,57.7425365317921));
#36187=CARTESIAN_POINT('Ctrl Pts',(67.3087010236234,33.9507020563743,55.9715414898151));
#36188=CARTESIAN_POINT('Ctrl Pts',(66.7849774198239,33.7736054843756,53.63690992163));
#36189=CARTESIAN_POINT('Ctrl Pts',(67.2156126057606,33.5965089123769,51.4747805783961));
#36190=CARTESIAN_POINT('Ctrl Pts',(67.6462477916973,33.4194123403782,49.3126512351621));
#36191=CARTESIAN_POINT('Ctrl Pts',(69.0245064207966,33.2423157683794,47.3568408855483));
#36192=CARTESIAN_POINT('Ctrl Pts',(70.9158061804463,33.0652191963807,46.2240411771315));
#36193=CARTESIAN_POINT('Ctrl Pts',(72.8071059400959,32.888122624382,45.0912414687147));
#36194=CARTESIAN_POINT('Ctrl Pts',(75.1818659698094,32.7110260523833,44.7991699473058));
#36195=CARTESIAN_POINT('Ctrl Pts',(77.2912945088659,32.5339294803846,45.4399204438754));
#36196=CARTESIAN_POINT('Ctrl Pts',(79.4007230479224,32.3568329083859,46.080670940445));
#36197=CARTESIAN_POINT('Ctrl Pts',(81.2118275942068,32.1797363363871,47.6442218013928));
#36198=CARTESIAN_POINT('Ctrl Pts',(82.1535440633094,32.0026397643884,49.6375657386152));
#36199=CARTESIAN_POINT('Ctrl Pts',(82.651569792991,31.9089824350461,50.691743510177));
#36200=CARTESIAN_POINT('Ctrl Pts',(82.9129498948691,31.8153251057038,51.8569119935386));
#36201=CARTESIAN_POINT('Ctrl Pts',(82.9129498948689,31.7216677763616,53.0228109606366));
#36202=CARTESIAN_POINT('Origin',(74.9879498948689,255.,53.0228109606356));
#36203=CARTESIAN_POINT('',(82.911855653882,26.278332223639,53.0203857348343));
#36204=CARTESIAN_POINT('',(82.9155439867214,27.7216677763616,53.0225420064449));
#36205=CARTESIAN_POINT('',(82.9129498948689,255.,53.0228109606356));
#36206=CARTESIAN_POINT('Ctrl Pts',(82.9100720036525,26.2783322236389,53.0164325339422));
#36207=CARTESIAN_POINT('Ctrl Pts',(82.9166505231298,26.3376963210343,52.2769432483488));
#36208=CARTESIAN_POINT('Ctrl Pts',(82.8216651276326,26.3970604184296,51.5389728574951));
#36209=CARTESIAN_POINT('Ctrl Pts',(82.6184217847882,26.456424515825,50.8318508162249));
#36210=CARTESIAN_POINT('Ctrl Pts',(81.892068677812,26.6685805253773,48.3047309386457));
#36211=CARTESIAN_POINT('Ctrl Pts',(79.7830322414838,26.8807365349295,46.1716098366969));
#36212=CARTESIAN_POINT('Ctrl Pts',(77.2662375055457,27.0928925444818,45.4178161108577));
#36213=CARTESIAN_POINT('Ctrl Pts',(74.7494427696069,27.3050485540342,44.6640223850185));
#36214=CARTESIAN_POINT('Ctrl Pts',(71.8248897340578,27.5172045635866,45.2895560352895));
#36215=CARTESIAN_POINT('Ctrl Pts',(69.8239829670763,27.7293605731389,46.9978578318098));
#36216=CARTESIAN_POINT('Ctrl Pts',(68.8235295835859,27.8354385779151,47.8520087300698));
#36217=CARTESIAN_POINT('Ctrl Pts',(68.0539877672371,27.9415165826912,48.9768516648921));
#36218=CARTESIAN_POINT('Ctrl Pts',(67.5843347182215,28.0475945874674,50.2154103675274));
#36219=CARTESIAN_POINT('Ctrl Pts',(67.114681669206,28.1536725922435,51.4539690701625));
#36220=CARTESIAN_POINT('Ctrl Pts',(66.9449173875235,28.2597505970196,52.80624354061));
#36221=CARTESIAN_POINT('Ctrl Pts',(67.1274899938208,28.3658286017957,54.108989854011));
#36222=CARTESIAN_POINT('Ctrl Pts',(67.4926352064155,28.577984611348,56.714482480814));
#36223=CARTESIAN_POINT('Ctrl Pts',(69.2671279709314,28.7901406209003,59.1218624794284));
#36224=CARTESIAN_POINT('Ctrl Pts',(71.6509432294986,29.0022966304527,60.2263467700827));
#36225=CARTESIAN_POINT('Ctrl Pts',(74.0347584880657,29.214452640005,61.3308310607369));
#36226=CARTESIAN_POINT('Ctrl Pts',(77.0278962406845,29.4266086495573,61.1324196434312));
#36227=CARTESIAN_POINT('Ctrl Pts',(79.2472298230731,29.6387646591097,59.7222842001146));
#36228=CARTESIAN_POINT('Ctrl Pts',(81.4665634054615,29.850920668662,58.3121487567983));
#36229=CARTESIAN_POINT('Ctrl Pts',(82.9120928176202,30.0630766782143,55.6902892874712));
#36230=CARTESIAN_POINT('Ctrl Pts',(82.9248920321598,30.2752326877666,53.0614541708519));
#36231=CARTESIAN_POINT('Ctrl Pts',(82.9249543630591,30.2762658663907,53.0486520058115));
#36232=CARTESIAN_POINT('Ctrl Pts',(82.9249827154302,30.2772990450147,53.0358496753372));
#36233=CARTESIAN_POINT('Ctrl Pts',(82.9249771640168,30.2783322236387,53.0230473193048));
#36234=CARTESIAN_POINT('Ctrl Pts',(82.9129498948689,31.7216677763616,53.0228109606366));
#36235=CARTESIAN_POINT('Ctrl Pts',(82.9129498948686,31.5445712043628,55.2274084205469));
#36236=CARTESIAN_POINT('Ctrl Pts',(81.9432795991097,31.3674746323641,57.4147653849834));
#36237=CARTESIAN_POINT('Ctrl Pts',(80.3096882702525,31.1903780603653,58.8951806410942));
#36238=CARTESIAN_POINT('Ctrl Pts',(78.6760969413953,31.0132814883665,60.3755958972049));
#36239=CARTESIAN_POINT('Ctrl Pts',(76.4041347530412,30.8361849163677,61.1259150206688));
#36240=CARTESIAN_POINT('Ctrl Pts',(74.2101800112183,30.659088344369,60.9095529374018));
#36241=CARTESIAN_POINT('Ctrl Pts',(72.0162252693954,30.4819917723702,60.6931908541348));
#36242=CARTESIAN_POINT('Ctrl Pts',(69.934592507694,30.3048952003715,59.5135315737669));
#36243=CARTESIAN_POINT('Ctrl Pts',(68.6216467656577,30.1277986283727,57.7425365317886));
#36244=CARTESIAN_POINT('Ctrl Pts',(67.3087010236215,29.9507020563739,55.9715414898104));
#36245=CARTESIAN_POINT('Ctrl Pts',(66.7849774198233,29.7736054843751,53.6369099216243));
#36246=CARTESIAN_POINT('Ctrl Pts',(67.2156126057618,29.5965089123764,51.47478057839));
#36247=CARTESIAN_POINT('Ctrl Pts',(67.6462477917003,29.4194123403776,49.3126512351558));
#36248=CARTESIAN_POINT('Ctrl Pts',(69.0245064208017,29.2423157683789,47.3568408855427));
#36249=CARTESIAN_POINT('Ctrl Pts',(70.915806180453,29.0652191963801,46.2240411771274));
#36250=CARTESIAN_POINT('Ctrl Pts',(72.8071059401044,28.8881226243813,45.0912414687122));
#36251=CARTESIAN_POINT('Ctrl Pts',(75.1818659698189,28.7110260523825,44.7991699473058));
#36252=CARTESIAN_POINT('Ctrl Pts',(77.2912945088752,28.5339294803838,45.4399204438782));
#36253=CARTESIAN_POINT('Ctrl Pts',(79.4007230479315,28.356832908385,46.0806709404506));
#36254=CARTESIAN_POINT('Ctrl Pts',(81.2118275942144,28.1797363363863,47.6442218014013));
#36255=CARTESIAN_POINT('Ctrl Pts',(82.1535440633143,28.0026397643875,49.6375657386256));
#36256=CARTESIAN_POINT('Ctrl Pts',(82.6515697929927,27.9089824350455,50.6917435101847));
#36257=CARTESIAN_POINT('Ctrl Pts',(82.912949894869,27.8153251057035,51.8569119935424));
#36258=CARTESIAN_POINT('Ctrl Pts',(82.9129498948689,27.7216677763616,53.0228109606364));
#36259=CARTESIAN_POINT('Origin',(74.9879498948689,255.,53.0228109606356));
#36260=CARTESIAN_POINT('',(82.9129498948689,22.2783322236388,53.0228109606233));
#36261=CARTESIAN_POINT('',(82.9107744051909,23.7216677763616,53.0210350023561));
#36262=CARTESIAN_POINT('',(82.9129498948689,255.,53.0228109606356));
#36263=CARTESIAN_POINT('Ctrl Pts',(82.9129498948689,22.2783322236388,53.0228109606233));
#36264=CARTESIAN_POINT('Ctrl Pts',(82.9129498948655,22.4554287956375,50.8182135007137));
#36265=CARTESIAN_POINT('Ctrl Pts',(81.943279599104,22.6325253676362,48.630856536279));
#36266=CARTESIAN_POINT('Ctrl Pts',(80.3096882702455,22.8096219396349,47.1504412801706));
#36267=CARTESIAN_POINT('Ctrl Pts',(78.676096941387,22.9867185116336,45.6700260240622));
#36268=CARTESIAN_POINT('Ctrl Pts',(76.4041347530328,23.1638150836324,44.9197069006011));
#36269=CARTESIAN_POINT('Ctrl Pts',(74.2101800112107,23.3409116556311,45.1360689838701));
#36270=CARTESIAN_POINT('Ctrl Pts',(72.0162252693886,23.5180082276298,45.3524310671391));
#36271=CARTESIAN_POINT('Ctrl Pts',(69.9345925076889,23.6951047996285,46.5320903475084));
#36272=CARTESIAN_POINT('Ctrl Pts',(68.6216467656543,23.8722013716272,48.3030853894872));
#36273=CARTESIAN_POINT('Ctrl Pts',(67.3087010236196,24.0492979436259,50.0740804314659));
#36274=CARTESIAN_POINT('Ctrl Pts',(66.7849774198231,24.2263945156247,52.4087119996516));
#36275=CARTESIAN_POINT('Ctrl Pts',(67.2156126057626,24.4034910876234,54.570841342885));
#36276=CARTESIAN_POINT('Ctrl Pts',(67.6462477917021,24.5805876596221,56.7329706861185));
#36277=CARTESIAN_POINT('Ctrl Pts',(69.0245064208038,24.7576842316208,58.6887810357304));
#36278=CARTESIAN_POINT('Ctrl Pts',(70.915806180455,24.9347808036195,59.8215807441448));
#36279=CARTESIAN_POINT('Ctrl Pts',(72.8071059401061,25.1118773756182,60.9543804525592));
#36280=CARTESIAN_POINT('Ctrl Pts',(75.1818659698199,25.288973947617,61.2464519739651));
#36281=CARTESIAN_POINT('Ctrl Pts',(77.2912945088756,25.4660705196157,60.6057014773928));
#36282=CARTESIAN_POINT('Ctrl Pts',(79.4007230479312,25.6431670916144,59.9649509808204));
#36283=CARTESIAN_POINT('Ctrl Pts',(81.2118275942137,25.8202636636131,58.4014001198704));
#36284=CARTESIAN_POINT('Ctrl Pts',(82.1535440633137,25.9973602356119,56.4080561826468));
#36285=CARTESIAN_POINT('Ctrl Pts',(82.6515697929942,26.0910175649542,55.3538784110837));
#36286=CARTESIAN_POINT('Ctrl Pts',(82.9129498948708,26.1846748942965,54.1887099277212));
#36287=CARTESIAN_POINT('Ctrl Pts',(82.9129498948689,26.2783322236388,53.0228109606226));
#36288=CARTESIAN_POINT('Ctrl Pts',(82.9230491389377,27.7216677763615,53.0217638758786));
#36289=CARTESIAN_POINT('Ctrl Pts',(82.9208703146659,27.6265346858863,54.2018633476581));
#36290=CARTESIAN_POINT('Ctrl Pts',(82.6384364768388,27.531401595411,55.3842255652826));
#36291=CARTESIAN_POINT('Ctrl Pts',(82.123537086314,27.4362685049358,56.4547799592356));
#36292=CARTESIAN_POINT('Ctrl Pts',(81.5493993206381,27.3301905001596,57.6484999734551));
#36293=CARTESIAN_POINT('Ctrl Pts',(80.6862294529177,27.2241124953835,58.703205626511));
#36294=CARTESIAN_POINT('Ctrl Pts',(79.6162123658362,27.1180344906073,59.4684142012732));
#36295=CARTESIAN_POINT('Ctrl Pts',(77.4761781916732,26.905878481055,60.9988313507976));
#36296=CARTESIAN_POINT('Ctrl Pts',(74.5087551400656,26.6937224715027,61.3712601871467));
#36297=CARTESIAN_POINT('Ctrl Pts',(72.0658749947129,26.4815664619504,60.4044110161784));
#36298=CARTESIAN_POINT('Ctrl Pts',(69.6229948493599,26.2694104523981,59.4375618452099));
#36299=CARTESIAN_POINT('Ctrl Pts',(67.7046576102617,26.0572544428458,57.1314346669236));
#36300=CARTESIAN_POINT('Ctrl Pts',(67.197698117,25.8450984332934,54.5513347107468));
#36301=CARTESIAN_POINT('Ctrl Pts',(66.6907386237383,25.6329424237411,51.9712347545703));
#36302=CARTESIAN_POINT('Ctrl Pts',(67.5951568763126,25.4207864141888,49.1171620205034));
#36303=CARTESIAN_POINT('Ctrl Pts',(69.4917218674496,25.2086304046365,47.2967283534847));
#36304=CARTESIAN_POINT('Ctrl Pts',(71.3882868585865,24.9964743950842,45.4762946864661));
#36305=CARTESIAN_POINT('Ctrl Pts',(74.276998588286,24.7843183855319,44.6895000864957));
#36306=CARTESIAN_POINT('Ctrl Pts',(76.8341764136125,24.5721623759795,45.3016807310096));
#36307=CARTESIAN_POINT('Ctrl Pts',(79.3913542389393,24.3600063664272,45.9138613755236));
#36308=CARTESIAN_POINT('Ctrl Pts',(81.6169981598929,24.1478503568749,47.9250172645221));
#36309=CARTESIAN_POINT('Ctrl Pts',(82.4830085759959,23.9356943473226,50.4054382966083));
#36310=CARTESIAN_POINT('Ctrl Pts',(82.7742238946445,23.8643521570022,51.2395351940708));
#36311=CARTESIAN_POINT('Ctrl Pts',(82.9116931305271,23.7930099666819,52.1266961542172));
#36312=CARTESIAN_POINT('Ctrl Pts',(82.9044091330798,23.7216677763616,53.0158387204223));
#36313=CARTESIAN_POINT('Origin',(74.9879498948689,255.,53.0228109606356));
#36314=CARTESIAN_POINT('',(82.9129498948689,18.2783322236388,53.0228109606232));
#36315=CARTESIAN_POINT('',(82.9101799821405,19.7216677763616,53.0246693339172));
#36316=CARTESIAN_POINT('',(82.9129498948689,255.,53.0228109606356));
#36317=CARTESIAN_POINT('Ctrl Pts',(82.9129498948689,18.2783322236388,53.0228109606232));
#36318=CARTESIAN_POINT('Ctrl Pts',(82.9129498948655,18.4554287956375,50.8182135007132));
#36319=CARTESIAN_POINT('Ctrl Pts',(81.9432795991037,18.6325253676362,48.6308565362783));
#36320=CARTESIAN_POINT('Ctrl Pts',(80.3096882702447,18.809621939635,47.1504412801699));
#36321=CARTESIAN_POINT('Ctrl Pts',(78.6760969413858,18.9867185116337,45.6700260240615));
#36322=CARTESIAN_POINT('Ctrl Pts',(76.4041347530311,19.1638150836325,44.9197069006007));
#36323=CARTESIAN_POINT('Ctrl Pts',(74.2101800112087,19.3409116556312,45.1360689838703));
#36324=CARTESIAN_POINT('Ctrl Pts',(72.0162252693864,19.51800822763,45.3524310671399));
#36325=CARTESIAN_POINT('Ctrl Pts',(69.9345925076868,19.6951047996287,46.53209034751));
#36326=CARTESIAN_POINT('Ctrl Pts',(68.6216467656526,19.8722013716274,48.3030853894895));
#36327=CARTESIAN_POINT('Ctrl Pts',(67.3087010236184,20.0492979436262,50.0740804314689));
#36328=CARTESIAN_POINT('Ctrl Pts',(66.7849774198228,20.226394515625,52.4087119996552));
#36329=CARTESIAN_POINT('Ctrl Pts',(67.2156126057633,20.4034910876237,54.5708413428887));
#36330=CARTESIAN_POINT('Ctrl Pts',(67.6462477917039,20.5805876596225,56.7329706861223));
#36331=CARTESIAN_POINT('Ctrl Pts',(69.0245064208069,20.7576842316212,58.6887810357338));
#36332=CARTESIAN_POINT('Ctrl Pts',(70.915806180459,20.9347808036199,59.8215807441473));
#36333=CARTESIAN_POINT('Ctrl Pts',(72.807105940111,21.1118773756186,60.9543804525607));
#36334=CARTESIAN_POINT('Ctrl Pts',(75.1818659698254,21.2889739476174,61.2464519739651));
#36335=CARTESIAN_POINT('Ctrl Pts',(77.2912945088809,21.4660705196162,60.6057014773912));
#36336=CARTESIAN_POINT('Ctrl Pts',(79.4007230479364,21.6431670916149,59.9649509808173));
#36337=CARTESIAN_POINT('Ctrl Pts',(81.211827594218,21.8202636636136,58.4014001198656));
#36338=CARTESIAN_POINT('Ctrl Pts',(82.1535440633165,21.9973602356124,56.408056182641));
#36339=CARTESIAN_POINT('Ctrl Pts',(82.6515697929951,22.0910175649545,55.3538784110796));
#36340=CARTESIAN_POINT('Ctrl Pts',(82.9129498948707,22.1846748942966,54.1887099277195));
#36341=CARTESIAN_POINT('Ctrl Pts',(82.9129498948689,22.2783322236388,53.0228109606233));
#36342=CARTESIAN_POINT('Ctrl Pts',(82.9129498948689,23.7216677763616,53.0228109606362));
#36343=CARTESIAN_POINT('Ctrl Pts',(82.9129498948687,23.5445712043629,55.2274084205459));
#36344=CARTESIAN_POINT('Ctrl Pts',(81.9432795991104,23.3674746323642,57.414765384982));
#36345=CARTESIAN_POINT('Ctrl Pts',(80.3096882702541,23.1903780603655,58.8951806410928));
#36346=CARTESIAN_POINT('Ctrl Pts',(78.6760969413977,23.0132814883668,60.3755958972035));
#36347=CARTESIAN_POINT('Ctrl Pts',(76.4041347530446,22.8361849163681,61.125915020668));
#36348=CARTESIAN_POINT('Ctrl Pts',(74.2101800112222,22.6590883443694,60.9095529374022));
#36349=CARTESIAN_POINT('Ctrl Pts',(72.0162252693998,22.4819917723706,60.6931908541363));
#36350=CARTESIAN_POINT('Ctrl Pts',(69.9345925076984,22.3048952003719,59.5135315737701));
#36351=CARTESIAN_POINT('Ctrl Pts',(68.6216467656612,22.1277986283732,57.7425365317933));
#36352=CARTESIAN_POINT('Ctrl Pts',(67.308701023624,21.9507020563744,55.9715414898164));
#36353=CARTESIAN_POINT('Ctrl Pts',(66.784977419824,21.7736054843758,53.6369099216315));
#36354=CARTESIAN_POINT('Ctrl Pts',(67.2156126057603,21.596508912377,51.4747805783974));
#36355=CARTESIAN_POINT('Ctrl Pts',(67.6462477916966,21.4194123403783,49.3126512351634));
#36356=CARTESIAN_POINT('Ctrl Pts',(69.0245064207955,21.2423157683796,47.3568408855494));
#36357=CARTESIAN_POINT('Ctrl Pts',(70.915806180445,21.0652191963808,46.2240411771322));
#36358=CARTESIAN_POINT('Ctrl Pts',(72.8071059400945,20.8881226243821,45.0912414687151));
#36359=CARTESIAN_POINT('Ctrl Pts',(75.1818659698079,20.7110260523834,44.7991699473057));
#36360=CARTESIAN_POINT('Ctrl Pts',(77.2912945088645,20.5339294803847,45.439920443875));
#36361=CARTESIAN_POINT('Ctrl Pts',(79.4007230479211,20.356832908386,46.0806709404443));
#36362=CARTESIAN_POINT('Ctrl Pts',(81.2118275942059,20.1797363363872,47.6442218013917));
#36363=CARTESIAN_POINT('Ctrl Pts',(82.1535440633088,20.0026397643885,49.6375657386139));
#36364=CARTESIAN_POINT('Ctrl Pts',(82.6515697929907,19.9089824350462,50.6917435101759));
#36365=CARTESIAN_POINT('Ctrl Pts',(82.912949894869,19.8153251057039,51.8569119935378));
#36366=CARTESIAN_POINT('Ctrl Pts',(82.9129498948689,19.7216677763616,53.0228109606361));
#36367=CARTESIAN_POINT('Origin',(74.9879498948689,255.,53.0228109606356));
#36368=CARTESIAN_POINT('',(82.9129498948689,15.,53.0228109606356));
#36369=CARTESIAN_POINT('',(82.922834243019,15.7216677763616,53.0299163294501));
#36370=CARTESIAN_POINT('',(82.9129498948689,255.,53.0228109606356));
#36371=CARTESIAN_POINT('',(78.3434537325876,15.,45.8432414056375));
#36372=CARTESIAN_POINT('Origin',(74.9879498948689,15.,53.0228109606356));
#36373=CARTESIAN_POINT('Ctrl Pts',(78.3434537325868,15.0000000000001,45.8432414056371));
#36374=CARTESIAN_POINT('Ctrl Pts',(76.3462220853698,15.1770965719988,44.9097984734794));
#36375=CARTESIAN_POINT('Ctrl Pts',(73.9540436795002,15.3541931439975,44.8621177977932));
#36376=CARTESIAN_POINT('Ctrl Pts',(71.9212025091824,15.5312897159962,45.7152336964265));
#36377=CARTESIAN_POINT('Ctrl Pts',(69.8883613388645,15.7083862879949,46.5683495950599));
#36378=CARTESIAN_POINT('Ctrl Pts',(68.2466520420155,15.8854828599937,48.3089189148464));
#36379=CARTESIAN_POINT('Ctrl Pts',(67.51372624642,16.0625794319924,50.3881182170757));
#36380=CARTESIAN_POINT('Ctrl Pts',(66.7808004508245,16.2396760039911,52.4673175193051));
#36381=CARTESIAN_POINT('Ctrl Pts',(66.968121477194,16.4167725759898,54.8526271020265));
#36382=CARTESIAN_POINT('Ctrl Pts',(68.0166246455609,16.5938691479885,56.7919287975254));
#36383=CARTESIAN_POINT('Ctrl Pts',(69.0651278139278,16.7709657199872,58.7312304930242));
#36384=CARTESIAN_POINT('Ctrl Pts',(70.9584140179181,16.948062291986,60.1941926668765));
#36385=CARTESIAN_POINT('Ctrl Pts',(73.0995062609109,17.1251588639847,60.7195249114956));
#36386=CARTESIAN_POINT('Ctrl Pts',(75.2405985039036,17.3022554359834,61.2448571561147));
#36387=CARTESIAN_POINT('Ctrl Pts',(77.5960090478467,17.4793520079821,60.8243430162519));
#36388=CARTESIAN_POINT('Ctrl Pts',(79.4230472686975,17.6564485799808,59.5905758989277));
#36389=CARTESIAN_POINT('Ctrl Pts',(81.2500854895483,17.8335451519795,58.3568087816034));
#36390=CARTESIAN_POINT('Ctrl Pts',(82.5201756089623,18.0106417239783,56.3290854126722));
#36391=CARTESIAN_POINT('Ctrl Pts',(82.832842208417,18.187738295977,54.1467725208472));
#36392=CARTESIAN_POINT('Ctrl Pts',(82.8861571784615,18.2179362718643,53.7746510769253));
#36393=CARTESIAN_POINT('Ctrl Pts',(82.9129498948695,18.2481342477515,53.3987323022059));
#36394=CARTESIAN_POINT('Ctrl Pts',(82.9129498948689,18.2783322236388,53.0228109606232));
#36395=CARTESIAN_POINT('Ctrl Pts',(82.9030122912126,19.7216677763617,53.0294782382423));
#36396=CARTESIAN_POINT('Ctrl Pts',(82.9086579729621,19.6412512331491,54.0339957391183));
#36397=CARTESIAN_POINT('Ctrl Pts',(82.7316773075948,19.5608346899366,55.0362729807911));
#36398=CARTESIAN_POINT('Ctrl Pts',(82.3629950679762,19.480418146724,55.9613819431945));
#36399=CARTESIAN_POINT('Ctrl Pts',(81.390332607921,19.2682621371717,58.4020168924711));
#36400=CARTESIAN_POINT('Ctrl Pts',(79.0833945161164,19.0561061276194,60.3055474649299));
#36401=CARTESIAN_POINT('Ctrl Pts',(76.501790689728,18.8439501180671,60.8122568728204));
#36402=CARTESIAN_POINT('Ctrl Pts',(75.2109887765338,18.7378721132909,61.0656115767657));
#36403=CARTESIAN_POINT('Ctrl Pts',(73.8515204296936,18.6317941085148,60.9697609895688));
#36404=CARTESIAN_POINT('Ctrl Pts',(72.5891317440186,18.5257161037386,60.5685453417559));
#36405=CARTESIAN_POINT('Ctrl Pts',(71.3267430583433,18.4196380989624,60.1673296939429));
#36406=CARTESIAN_POINT('Ctrl Pts',(70.1614340338332,18.3135600941862,59.4607489855137));
#36407=CARTESIAN_POINT('Ctrl Pts',(69.253909830781,18.2074820894101,58.5084666850121));
#36408=CARTESIAN_POINT('Ctrl Pts',(67.4388614246767,17.9953260798577,56.6039020840091));
#36409=CARTESIAN_POINT('Ctrl Pts',(66.6549523044037,17.7831700703054,53.7165311147166));
#36410=CARTESIAN_POINT('Ctrl Pts',(67.2700601338688,17.5710140607531,51.1626732511785));
#36411=CARTESIAN_POINT('Ctrl Pts',(67.8851679633337,17.3588580512008,48.608815387641));
#36412=CARTESIAN_POINT('Ctrl Pts',(69.8992927425361,17.1467020416485,46.3884706298577));
#36413=CARTESIAN_POINT('Ctrl Pts',(72.3832175225222,16.9345460320962,45.5243909463029));
#36414=CARTESIAN_POINT('Ctrl Pts',(74.8671423025088,16.7223900225439,44.6603112627479));
#36415=CARTESIAN_POINT('Ctrl Pts',(77.8208670832794,16.5102340129916,45.152496653422));
#36416=CARTESIAN_POINT('Ctrl Pts',(79.8884469946644,16.2980780034393,46.7770485682758));
#36417=CARTESIAN_POINT('Ctrl Pts',(81.7609278618296,16.1059412610801,48.2483060328749));
#36418=CARTESIAN_POINT('Ctrl Pts',(82.9066087649531,15.9138045187209,50.648310000996));
#36419=CARTESIAN_POINT('Ctrl Pts',(82.922834243019,15.7216677763616,53.0299163294501));
#36420=CARTESIAN_POINT('Origin',(74.9879498948689,416.,53.0228109606356));
#36421=CARTESIAN_POINT('',(70.1710194129307,439.948460488314,53.0227057148971));
#36422=CARTESIAN_POINT('',(70.1715766354573,438.426539511686,53.0228415555562));
#36423=CARTESIAN_POINT('',(70.1711998948689,416.,53.0228109606356));
#36424=CARTESIAN_POINT('',(70.1716517717484,438.198460488314,53.0228096900326));
#36425=CARTESIAN_POINT('Ctrl Pts',(70.1716517717486,438.198460488314,53.0228096900326));
#36426=CARTESIAN_POINT('Ctrl Pts',(70.171762094604,438.224019932922,53.464926508948));
#36427=CARTESIAN_POINT('Ctrl Pts',(70.3403863287184,438.295435847886,54.7004002781471));
#36428=CARTESIAN_POINT('Ctrl Pts',(71.3835049550069,438.412708233207,56.5125746552081));
#36429=CARTESIAN_POINT('Ctrl Pts',(73.4687602399829,438.550277644276,57.8043411146894));
#36430=CARTESIAN_POINT('Ctrl Pts',(75.9171988302832,438.687847055345,57.9530481846181));
#36431=CARTESIAN_POINT('Ctrl Pts',(78.1434978095446,438.825416466414,56.9232374758342));
#36432=CARTESIAN_POINT('Ctrl Pts',(79.6154836096685,438.962985877483,54.9610361557711));
#36433=CARTESIAN_POINT('Ctrl Pts',(79.9812781097431,439.100555288552,52.5355178274692));
#36434=CARTESIAN_POINT('Ctrl Pts',(79.1534426071904,439.238124699621,50.2264819254732));
#36435=CARTESIAN_POINT('Ctrl Pts',(77.3298657797079,439.37569411069,48.5858962981143));
#36436=CARTESIAN_POINT('Ctrl Pts',(74.946465455023,439.513263521759,48.0059331744372));
#36437=CARTESIAN_POINT('Ctrl Pts',(72.5729817051559,439.650832932828,48.6252307671089));
#36438=CARTESIAN_POINT('Ctrl Pts',(70.7767845007438,439.788402343897,50.2957485891607));
#36439=CARTESIAN_POINT('Ctrl Pts',(70.2074030943593,439.887611529059,51.9705707881673));
#36440=CARTESIAN_POINT('Ctrl Pts',(70.170895409116,439.940964243864,52.8930801168023));
#36441=CARTESIAN_POINT('Ctrl Pts',(70.1710194129309,439.948460488314,53.0227057148971));
#36442=CARTESIAN_POINT('',(70.1711998948689,416.,53.0228109606356));
#36443=CARTESIAN_POINT('',(70.1711998948689,416.,53.0228109606356));
#36444=CARTESIAN_POINT('Origin',(74.9879498948689,416.,53.0228109606356));
#36445=CARTESIAN_POINT('',(71.3431312258735,438.,49.8737829466856));
#36446=CARTESIAN_POINT('Ctrl Pts',(71.3431312258736,438.,49.8737829466856));
#36447=CARTESIAN_POINT('Ctrl Pts',(70.8246667948602,438.045856470356,50.4738756829193));
#36448=CARTESIAN_POINT('Ctrl Pts',(70.2950910214935,438.112009966461,51.5275346151049));
#36449=CARTESIAN_POINT('Ctrl Pts',(70.1715641632004,438.178163462565,52.6717200402042));
#36450=CARTESIAN_POINT('Ctrl Pts',(70.1716517717486,438.198460488314,53.0228096900326));
#36451=CARTESIAN_POINT('',(74.7983630544234,438.,48.2104548970639));
#36452=CARTESIAN_POINT('Origin',(74.9879498948689,438.,53.0228109606356));
#36453=CARTESIAN_POINT('Ctrl Pts',(70.1715766354573,438.426539511686,53.0228415555562));
#36454=CARTESIAN_POINT('Ctrl Pts',(70.1716376521608,438.402395353675,52.6052026582204));
#36455=CARTESIAN_POINT('Ctrl Pts',(70.2254319475252,438.378251195664,52.1875501723899));
#36456=CARTESIAN_POINT('Ctrl Pts',(70.3327672197935,438.354107037653,51.7841487615086));
#36457=CARTESIAN_POINT('Ctrl Pts',(70.5366266801429,438.308250583211,51.0179775655125));
#36458=CARTESIAN_POINT('Ctrl Pts',(70.9336220846199,438.262394128769,50.3032136275511));
#36459=CARTESIAN_POINT('Ctrl Pts',(71.4763794327931,438.216537674328,49.7252773752126));
#36460=CARTESIAN_POINT('Ctrl Pts',(72.0191367809662,438.170681219886,49.1473411228741));
#36461=CARTESIAN_POINT('Ctrl Pts',(72.7076560728355,438.124824765444,48.7062325561585));
#36462=CARTESIAN_POINT('Ctrl Pts',(73.4594632851625,438.078968311002,48.4547383628616));
#36463=CARTESIAN_POINT('Ctrl Pts',(73.8910197329203,438.052645540668,48.3103743039495));
#36464=CARTESIAN_POINT('Ctrl Pts',(74.3434298781826,438.026322770334,48.2284891629282));
#36465=CARTESIAN_POINT('Ctrl Pts',(74.7983630544234,438.,48.2104548970639));
#36466=CARTESIAN_POINT('Origin',(74.9879498948689,416.,53.0228109606356));
#36467=CARTESIAN_POINT('',(70.1709154736136,441.698460488314,53.0228942458375));
#36468=CARTESIAN_POINT('',(70.1712218667098,440.176539511686,53.0226919906017));
#36469=CARTESIAN_POINT('',(70.1711998948689,416.,53.0228109606356));
#36470=CARTESIAN_POINT('Ctrl Pts',(70.1710194129309,439.948460488314,53.0227057148971));
#36471=CARTESIAN_POINT('Ctrl Pts',(70.1716539725937,439.986820714221,53.6860334998797));
#36472=CARTESIAN_POINT('Ctrl Pts',(70.4750683395013,440.071037410484,55.1428772890645));
#36473=CARTESIAN_POINT('Ctrl Pts',(71.8973337884151,440.201110577104,56.9748832301599));
#36474=CARTESIAN_POINT('Ctrl Pts',(74.1403626764107,440.338679988173,57.967745644851));
#36475=CARTESIAN_POINT('Ctrl Pts',(76.5860032023106,440.476249399242,57.7785452633612));
#36476=CARTESIAN_POINT('Ctrl Pts',(78.6496367890598,440.613818810311,56.4525095214311));
#36477=CARTESIAN_POINT('Ctrl Pts',(79.8379617752664,440.75138822138,54.3066208723653));
#36478=CARTESIAN_POINT('Ctrl Pts',(79.8669148016947,440.888957632449,51.8538436524662));
#36479=CARTESIAN_POINT('Ctrl Pts',(78.729574786843,441.026527043518,49.6805024325154));
#36480=CARTESIAN_POINT('Ctrl Pts',(76.6978173786037,441.164096454587,48.3061239541028));
#36481=CARTESIAN_POINT('Ctrl Pts',(74.257324391025,441.301665865656,48.0592467671762));
#36482=CARTESIAN_POINT('Ctrl Pts',(71.9914839080614,441.439235276725,48.9988856731345));
#36483=CARTESIAN_POINT('Ctrl Pts',(70.5016832392066,441.571500150944,50.8271031133775));
#36484=CARTESIAN_POINT('Ctrl Pts',(70.1714871278914,441.657908554807,52.3217110697681));
#36485=CARTESIAN_POINT('Ctrl Pts',(70.1709154736138,441.698460488314,53.0228942458375));
#36486=CARTESIAN_POINT('Ctrl Pts',(70.1712218667098,440.176539511686,53.0226919906017));
#36487=CARTESIAN_POINT('Ctrl Pts',(70.1710294008066,440.165195928084,52.8265141535113));
#36488=CARTESIAN_POINT('Ctrl Pts',(70.1827930416903,440.153852344482,52.6303592478741));
#36489=CARTESIAN_POINT('Ctrl Pts',(70.2066969022817,440.14250876088,52.4356951053063));
#36490=CARTESIAN_POINT('Ctrl Pts',(70.3033282960843,440.096652306438,51.6487650047139));
#36491=CARTESIAN_POINT('Ctrl Pts',(70.5983529615977,440.050795851997,50.886196684207));
#36492=CARTESIAN_POINT('Ctrl Pts',(71.056508807961,440.004939397555,50.2391342229322));
#36493=CARTESIAN_POINT('Ctrl Pts',(71.5146646543244,439.959082943113,49.5920717616573));
#36494=CARTESIAN_POINT('Ctrl Pts',(72.1359516815378,439.913226488672,49.0605151596145));
#36495=CARTESIAN_POINT('Ctrl Pts',(72.8461121117878,439.86737003423,48.7079973939007));
#36496=CARTESIAN_POINT('Ctrl Pts',(73.5562725420377,439.821513579788,48.3554796281869));
#36497=CARTESIAN_POINT('Ctrl Pts',(74.3553063753243,439.775657125346,48.1820006988021));
#36498=CARTESIAN_POINT('Ctrl Pts',(75.1477110700954,439.729800670905,48.2082952456863));
#36499=CARTESIAN_POINT('Ctrl Pts',(75.9401157648664,439.683944216463,48.2345897925705));
#36500=CARTESIAN_POINT('Ctrl Pts',(76.7258913211219,439.638087762021,48.4606578157238));
#36501=CARTESIAN_POINT('Ctrl Pts',(77.4111199028447,439.592231307579,48.8594790915802));
#36502=CARTESIAN_POINT('Ctrl Pts',(78.0963484845675,439.546374853138,49.2583003674367));
#36503=CARTESIAN_POINT('Ctrl Pts',(78.6810300917576,439.500518398696,49.8298748959963));
#36504=CARTESIAN_POINT('Ctrl Pts',(79.0952820469545,439.454661944254,50.5058866713264));
#36505=CARTESIAN_POINT('Ctrl Pts',(79.5095340021513,439.408805489813,51.1818984466564));
#36506=CARTESIAN_POINT('Ctrl Pts',(79.7533563053549,439.362949035371,51.9623474687568));
#36507=CARTESIAN_POINT('Ctrl Pts',(79.7976068454851,439.317092580929,52.7539524829401));
#36508=CARTESIAN_POINT('Ctrl Pts',(79.8418573856152,439.271236126487,53.5455574971234));
#36509=CARTESIAN_POINT('Ctrl Pts',(79.6865361626719,439.225379672046,54.3483185033896));
#36510=CARTESIAN_POINT('Ctrl Pts',(79.3502072440678,439.179523217604,55.0662875695242));
#36511=CARTESIAN_POINT('Ctrl Pts',(79.0138783254638,439.133666763162,55.7842566356588));
#36512=CARTESIAN_POINT('Ctrl Pts',(78.496541711199,439.08781030872,56.4174337616619));
#36513=CARTESIAN_POINT('Ctrl Pts',(77.8600314557391,439.041953854279,56.8901398913939));
#36514=CARTESIAN_POINT('Ctrl Pts',(77.2235212002792,438.996097399837,57.3628460211258));
#36515=CARTESIAN_POINT('Ctrl Pts',(76.4678373036241,438.950240945395,57.6750811545867));
#36516=CARTESIAN_POINT('Ctrl Pts',(75.6832994784698,438.904384490954,57.7895265539831));
#36517=CARTESIAN_POINT('Ctrl Pts',(74.8987616533154,438.858528036512,57.9039719533795));
#36518=CARTESIAN_POINT('Ctrl Pts',(74.0853698996618,438.81267158207,57.8206276187115));
#36519=CARTESIAN_POINT('Ctrl Pts',(73.3403461325011,438.766815127628,57.5494544577645));
#36520=CARTESIAN_POINT('Ctrl Pts',(72.5953223653404,438.720958673187,57.2782812968174));
#36521=CARTESIAN_POINT('Ctrl Pts',(71.9186665846726,438.675102218745,56.8192793095913));
#36522=CARTESIAN_POINT('Ctrl Pts',(71.391247014838,438.629245764303,56.2273115731785));
#36523=CARTESIAN_POINT('Ctrl Pts',(70.8638274450034,438.583389309861,55.6353438367656));
#36524=CARTESIAN_POINT('Ctrl Pts',(70.485644086002,438.53753285542,54.9104103511661));
#36525=CARTESIAN_POINT('Ctrl Pts',(70.3019141646122,438.491676400978,54.1391543813509));
#36526=CARTESIAN_POINT('Ctrl Pts',(70.2149209906975,438.469964104547,53.7739770373049));
#36527=CARTESIAN_POINT('Ctrl Pts',(70.1715217645128,438.448251808117,53.3984147909377));
#36528=CARTESIAN_POINT('Ctrl Pts',(70.1715766354573,438.426539511686,53.0228415555562));
#36529=CARTESIAN_POINT('Origin',(74.9879498948689,416.,53.0228109606356));
#36530=CARTESIAN_POINT('',(70.1715080739194,443.448460488314,53.0228810481615));
#36531=CARTESIAN_POINT('',(70.170796016094,441.926539511687,53.0228364485998));
#36532=CARTESIAN_POINT('',(70.1711998948689,416.,53.0228109606356));
#36533=CARTESIAN_POINT('Ctrl Pts',(70.1709154736138,441.698460488314,53.0228942458375));
#36534=CARTESIAN_POINT('Ctrl Pts',(70.1708406963857,441.703765025163,53.1146149524511));
#36535=CARTESIAN_POINT('Ctrl Pts',(70.1955986940716,441.754926032369,53.9991991984498));
#36536=CARTESIAN_POINT('Ctrl Pts',(70.713585383041,441.851943509931,55.6497085889238));
#36537=CARTESIAN_POINT('Ctrl Pts',(72.4698494135181,441.989512921,57.3621603468108));
#36538=CARTESIAN_POINT('Ctrl Pts',(74.828053225208,442.127082332069,58.0373115523705));
#36539=CARTESIAN_POINT('Ctrl Pts',(77.2244795649762,442.264651743138,57.5137705645742));
#36540=CARTESIAN_POINT('Ctrl Pts',(79.0862742686079,442.402221154207,55.9166873327523));
#36541=CARTESIAN_POINT('Ctrl Pts',(79.9683842872405,442.539790565276,53.6278369045098));
#36542=CARTESIAN_POINT('Ctrl Pts',(79.6599454732541,442.677359976345,51.194357940996));
#36543=CARTESIAN_POINT('Ctrl Pts',(78.2346886382596,442.814929387414,49.1979618575147));
#36544=CARTESIAN_POINT('Ctrl Pts',(76.0333145580138,442.952498798483,48.1158775139168));
#36545=CARTESIAN_POINT('Ctrl Pts',(73.5820510943691,443.090068209552,48.2067719562013));
#36546=CARTESIAN_POINT('Ctrl Pts',(71.466860961653,443.227637620621,49.4489173061093));
#36547=CARTESIAN_POINT('Ctrl Pts',(70.3609725105829,443.347101713542,51.2694715578199));
#36548=CARTESIAN_POINT('Ctrl Pts',(70.1717606038319,443.420709336106,52.542866079208));
#36549=CARTESIAN_POINT('Ctrl Pts',(70.1715080739196,443.448460488314,53.0228810481615));
#36550=CARTESIAN_POINT('Ctrl Pts',(70.170796016094,441.926539511687,53.0228364485998));
#36551=CARTESIAN_POINT('Ctrl Pts',(70.1710241501999,441.882140048052,52.2551809390674));
#36552=CARTESIAN_POINT('Ctrl Pts',(70.3579454689711,441.837740584417,51.4874182485368));
#36553=CARTESIAN_POINT('Ctrl Pts',(70.7112275018185,441.793341120782,50.805891752147));
#36554=CARTESIAN_POINT('Ctrl Pts',(71.0761026628707,441.747484666341,50.1020006198204));
#36555=CARTESIAN_POINT('Ctrl Pts',(71.6184361063414,441.701628211899,49.4900983141799));
#36556=CARTESIAN_POINT('Ctrl Pts',(72.2734067786708,441.655771757457,49.0433209336992));
#36557=CARTESIAN_POINT('Ctrl Pts',(72.9283774510002,441.609915303015,48.5965435532186));
#36558=CARTESIAN_POINT('Ctrl Pts',(73.6959853521882,441.564058848574,48.3148910978977));
#36559=CARTESIAN_POINT('Ctrl Pts',(74.4844840604079,441.518202394132,48.2320273756972));
#36560=CARTESIAN_POINT('Ctrl Pts',(75.2729827686276,441.47234593969,48.1491636534967));
#36561=CARTESIAN_POINT('Ctrl Pts',(76.082372283879,441.426489485249,48.2650886644164));
#36562=CARTESIAN_POINT('Ctrl Pts',(76.8159123410153,441.380633030807,48.5659467603638));
#36563=CARTESIAN_POINT('Ctrl Pts',(77.5494523981515,441.334776576365,48.8668048563111));
#36564=CARTESIAN_POINT('Ctrl Pts',(78.2071429971726,441.288920121923,49.3525960372861));
#36565=CARTESIAN_POINT('Ctrl Pts',(78.7103753079263,441.243063667482,49.9652573227733));
#36566=CARTESIAN_POINT('Ctrl Pts',(79.21360761868,441.19720721304,50.5779186082605));
#36567=CARTESIAN_POINT('Ctrl Pts',(79.5623816411664,441.151350758598,51.3174499982598));
#36568=CARTESIAN_POINT('Ctrl Pts',(79.7150110293437,441.105494304157,52.0954608459898));
#36569=CARTESIAN_POINT('Ctrl Pts',(79.8676404175208,441.059637849715,52.8734716937199));
#36570=CARTESIAN_POINT('Ctrl Pts',(79.8241251713888,441.013781395273,53.6899619991806));
#36571=CARTESIAN_POINT('Ctrl Pts',(79.5896663423308,440.967924940831,54.4473427929661));
#36572=CARTESIAN_POINT('Ctrl Pts',(79.3552075132728,440.92206848639,55.2047235867516));
#36573=CARTESIAN_POINT('Ctrl Pts',(78.9298051012887,440.876212031948,55.9029948688619));
#36574=CARTESIAN_POINT('Ctrl Pts',(78.3643042697189,440.830355577506,56.4586975041123));
#36575=CARTESIAN_POINT('Ctrl Pts',(77.7988034381491,440.784499123064,57.0144001393626));
#36576=CARTESIAN_POINT('Ctrl Pts',(77.0932041869936,440.738642668623,57.427534127753));
#36577=CARTESIAN_POINT('Ctrl Pts',(76.3318415087392,440.692786214181,57.6487206586682));
#36578=CARTESIAN_POINT('Ctrl Pts',(75.5704788304848,440.646929759739,57.8699071895835));
#36579=CARTESIAN_POINT('Ctrl Pts',(74.7533527251315,440.601073305297,57.8991462630236));
#36580=CARTESIAN_POINT('Ctrl Pts',(73.9781281543607,440.555216850856,57.7329431516146));
#36581=CARTESIAN_POINT('Ctrl Pts',(73.2029035835899,440.509360396414,57.5667400402056));
#36582=CARTESIAN_POINT('Ctrl Pts',(72.4695805474015,440.463503941972,57.2050947439475));
#36583=CARTESIAN_POINT('Ctrl Pts',(71.8658076548209,440.41764748753,56.691232015746));
#36584=CARTESIAN_POINT('Ctrl Pts',(71.2620347622404,440.371791033089,56.1773692875446));
#36585=CARTESIAN_POINT('Ctrl Pts',(70.7878120132677,440.325934578647,55.5112891273998));
#36586=CARTESIAN_POINT('Ctrl Pts',(70.4998196998274,440.280078124205,54.7726031069883));
#36587=CARTESIAN_POINT('Ctrl Pts',(70.2830685000765,440.245565253366,54.2166470147902));
#36588=CARTESIAN_POINT('Ctrl Pts',(70.1718074445211,440.211052382526,53.6195633665776));
#36589=CARTESIAN_POINT('Ctrl Pts',(70.1712218667098,440.176539511686,53.0226919906017));
#36590=CARTESIAN_POINT('Origin',(74.9879498948689,416.,53.0228109606356));
#36591=CARTESIAN_POINT('',(70.1713954601516,445.198460488314,53.0227079586499));
#36592=CARTESIAN_POINT('',(70.1713650637522,443.676539511686,53.0229190193667));
#36593=CARTESIAN_POINT('',(70.1711998948689,416.,53.0228109606356));
#36594=CARTESIAN_POINT('Ctrl Pts',(70.1715080739196,443.448460488314,53.0228810481615));
#36595=CARTESIAN_POINT('Ctrl Pts',(70.1713433191603,443.466565806462,53.3360508821162));
#36596=CARTESIAN_POINT('Ctrl Pts',(70.2776498508399,443.530527594967,54.4422951112801));
#36597=CARTESIAN_POINT('Ctrl Pts',(71.1151991800427,443.640345853828,56.2122599773613));
#36598=CARTESIAN_POINT('Ctrl Pts',(73.090160210338,443.777915264897,57.6670738130985));
#36599=CARTESIAN_POINT('Ctrl Pts',(75.5187787161611,443.915484675966,58.0116990022701));
#36600=CARTESIAN_POINT('Ctrl Pts',(77.8205051511885,444.053054087035,57.1637545547184));
#36601=CARTESIAN_POINT('Ctrl Pts',(79.4451229069195,444.190623498104,55.3259375029962));
#36602=CARTESIAN_POINT('Ctrl Pts',(80.004274940543,444.328192909173,52.9375691538648));
#36603=CARTESIAN_POINT('Ctrl Pts',(79.3642986538913,444.465762320242,50.569577447722));
#36604=CARTESIAN_POINT('Ctrl Pts',(77.6781772931937,444.603331731311,48.7880193866875));
#36605=CARTESIAN_POINT('Ctrl Pts',(75.3489700415422,444.74090114238,48.0187678370029));
#36606=CARTESIAN_POINT('Ctrl Pts',(72.9334626641764,444.878470553449,48.4457086733363));
#36607=CARTESIAN_POINT('Ctrl Pts',(71.0090705553659,445.016039964518,49.9667837468897));
#36608=CARTESIAN_POINT('Ctrl Pts',(70.2544612753753,445.12270327614,51.7125461193628));
#36609=CARTESIAN_POINT('Ctrl Pts',(70.1711887931693,445.183510117405,52.7641269590152));
#36610=CARTESIAN_POINT('Ctrl Pts',(70.1713954601518,445.198460488314,53.0227079586499));
#36611=CARTESIAN_POINT('Ctrl Pts',(70.1713650637522,443.676539511686,53.0229190193667));
#36612=CARTESIAN_POINT('Ctrl Pts',(70.1718277712569,443.644940622461,52.4763958288777));
#36613=CARTESIAN_POINT('Ctrl Pts',(70.2647396080943,443.613341733235,51.9297192730009));
#36614=CARTESIAN_POINT('Ctrl Pts',(70.447118527273,443.58174284401,51.4147264805034));
#36615=CARTESIAN_POINT('Ctrl Pts',(70.7117876597462,443.535886389568,50.6673665540712));
#36616=CARTESIAN_POINT('Ctrl Pts',(71.1648740101699,443.490029935126,49.9867324713112));
#36617=CARTESIAN_POINT('Ctrl Pts',(71.7522235614141,443.444173480685,49.454175325106));
#36618=CARTESIAN_POINT('Ctrl Pts',(72.3395731126582,443.398317026243,48.9216181789009));
#36619=CARTESIAN_POINT('Ctrl Pts',(73.0611858647228,443.352460571801,48.5371379692506));
#36620=CARTESIAN_POINT('Ctrl Pts',(73.8308128513784,443.306604117359,48.3466887352477));
#36621=CARTESIAN_POINT('Ctrl Pts',(74.600439838034,443.260747662918,48.1562395012448));
#36622=CARTESIAN_POINT('Ctrl Pts',(75.4180810592806,443.214891208476,48.1598212428892));
#36623=CARTESIAN_POINT('Ctrl Pts',(76.1860099853732,443.169034754034,48.3570058614351));
#36624=CARTESIAN_POINT('Ctrl Pts',(76.9539389114658,443.123178299593,48.554190479981));
#36625=CARTESIAN_POINT('Ctrl Pts',(77.6721555424045,443.077321845151,48.9449779754284));
#36626=CARTESIAN_POINT('Ctrl Pts',(78.2548168248756,443.031465390709,49.4826604460651));
#36627=CARTESIAN_POINT('Ctrl Pts',(78.8374781073467,442.985608936267,50.0203429167019));
#36628=CARTESIAN_POINT('Ctrl Pts',(79.2845840413502,442.939752481826,50.7049203625279));
#36629=CARTESIAN_POINT('Ctrl Pts',(79.5426954041279,442.893896027384,51.4545703700153));
#36630=CARTESIAN_POINT('Ctrl Pts',(79.8008067669057,442.848039572942,52.2042203775027));
#36631=CARTESIAN_POINT('Ctrl Pts',(79.8699235584575,442.8021831185,53.0189429466516));
#36632=CARTESIAN_POINT('Ctrl Pts',(79.7417847664839,442.756326664059,53.8013603923367));
#36633=CARTESIAN_POINT('Ctrl Pts',(79.6136459745102,442.710470209617,54.5837778380218));
#36634=CARTESIAN_POINT('Ctrl Pts',(79.2882515990109,442.664613755175,55.3338901602431));
#36635=CARTESIAN_POINT('Ctrl Pts',(78.8044935919692,442.618757300734,55.9620420526576));
#36636=CARTESIAN_POINT('Ctrl Pts',(78.3207355849274,442.572900846292,56.590193945072));
#36637=CARTESIAN_POINT('Ctrl Pts',(77.6786139463432,442.52704439185,57.0963854076795));
#36638=CARTESIAN_POINT('Ctrl Pts',(76.9548766651661,442.481187937408,57.4201151671322));
#36639=CARTESIAN_POINT('Ctrl Pts',(76.231139383989,442.435331482967,57.7438449265848));
#36640=CARTESIAN_POINT('Ctrl Pts',(75.4257864602191,442.389475028525,57.8851129828826));
#36641=CARTESIAN_POINT('Ctrl Pts',(74.6350756954628,442.343618574083,57.8270346235782));
#36642=CARTESIAN_POINT('Ctrl Pts',(73.8443649307066,442.297762119641,57.7689562642738));
#36643=CARTESIAN_POINT('Ctrl Pts',(73.0682963249641,442.2519056652,57.5115314893672));
#36644=CARTESIAN_POINT('Ctrl Pts',(72.3996275446939,442.206049210758,57.0855283536829));
#36645=CARTESIAN_POINT('Ctrl Pts',(71.7309587644238,442.160192756316,56.6595252179985));
#36646=CARTESIAN_POINT('Ctrl Pts',(71.169689809626,442.114336301875,56.0649437215364));
#36647=CARTESIAN_POINT('Ctrl Pts',(70.7829049536723,442.068479847433,55.3728497362095));
#36648=CARTESIAN_POINT('Ctrl Pts',(70.3961200977185,442.022623392991,54.6807557508826));
#36649=CARTESIAN_POINT('Ctrl Pts',(70.1838193406088,441.976766938549,53.8911492766908));
#36650=CARTESIAN_POINT('Ctrl Pts',(70.1713774013708,441.930910484108,53.0984060600886));
#36651=CARTESIAN_POINT('Ctrl Pts',(70.1709820853501,441.929453493301,53.0732183391237));
#36652=CARTESIAN_POINT('Ctrl Pts',(70.1707885297582,441.927996502494,53.0480274515711));
#36653=CARTESIAN_POINT('Ctrl Pts',(70.170796016094,441.926539511687,53.0228364485998));
#36654=CARTESIAN_POINT('Origin',(74.9879498948689,416.,53.0228109606356));
#36655=CARTESIAN_POINT('',(70.1708091458864,446.948460488314,53.022773765229));
#36656=CARTESIAN_POINT('',(70.1715262232373,445.426539511687,53.0227498862744));
#36657=CARTESIAN_POINT('',(70.1711998948689,416.,53.0228109606356));
#36658=CARTESIAN_POINT('Ctrl Pts',(70.1713954601518,445.198460488314,53.0227079586499));
#36659=CARTESIAN_POINT('Ctrl Pts',(70.1718226917137,445.229366587761,53.5572585820871));
#36660=CARTESIAN_POINT('Ctrl Pts',(70.3923929886614,445.306129157565,54.8852847418079));
#36661=CARTESIAN_POINT('Ctrl Pts',(71.5903202847087,445.428748197725,56.7142735653008));
#36662=CARTESIAN_POINT('Ctrl Pts',(73.7464922800195,445.566317608794,57.8838361734905));
#36663=CARTESIAN_POINT('Ctrl Pts',(76.1994287335407,445.703887019863,57.891394137796));
#36664=CARTESIAN_POINT('Ctrl Pts',(78.3627670107798,445.841456430932,56.7351407632842));
#36665=CARTESIAN_POINT('Ctrl Pts',(79.7193715252362,445.979025842001,54.691472845252));
#36666=CARTESIAN_POINT('Ctrl Pts',(79.9449525074299,446.11659525307,52.2489193477191));
#36667=CARTESIAN_POINT('Ctrl Pts',(78.9855859110121,446.254164664139,49.9913609096016));
#36668=CARTESIAN_POINT('Ctrl Pts',(77.0706036960962,446.391734075208,48.4584559926568));
#36669=CARTESIAN_POINT('Ctrl Pts',(74.6577731297195,446.529303486277,48.0166381276987));
#36670=CARTESIAN_POINT('Ctrl Pts',(72.3238697273887,446.666872897346,48.7715217455012));
#36671=CARTESIAN_POINT('Ctrl Pts',(70.6268018465247,446.804442308415,50.54265555625));
#36672=CARTESIAN_POINT('Ctrl Pts',(70.1802031047041,446.898304838737,52.155596267003));
#36673=CARTESIAN_POINT('Ctrl Pts',(70.1707936064121,446.946310898704,52.9856076092154));
#36674=CARTESIAN_POINT('Ctrl Pts',(70.1708091458866,446.948460488314,53.022773765229));
#36675=CARTESIAN_POINT('Ctrl Pts',(70.1715262232373,445.426539511687,53.0227498862744));
#36676=CARTESIAN_POINT('Ctrl Pts',(70.1713779019995,445.40774119687,52.6975896937802));
#36677=CARTESIAN_POINT('Ctrl Pts',(70.2038342589014,445.388942882054,52.3724587093238));
#36678=CARTESIAN_POINT('Ctrl Pts',(70.2691946807472,445.370144567237,52.0540827049399));
#36679=CARTESIAN_POINT('Ctrl Pts',(70.4286343558419,445.324288112796,51.2774389002736));
#36680=CARTESIAN_POINT('Ctrl Pts',(70.7838740194541,445.278431658354,50.5409914975681));
#36681=CARTESIAN_POINT('Ctrl Pts',(71.2924545359011,445.232575203912,49.9327625377089));
#36682=CARTESIAN_POINT('Ctrl Pts',(71.801035052348,445.18671874947,49.3245335778497));
#36683=CARTESIAN_POINT('Ctrl Pts',(72.4629564216298,445.140862295029,48.8445230608368));
#36684=CARTESIAN_POINT('Ctrl Pts',(73.1991041413178,445.095005840587,48.550103047728));
#36685=CARTESIAN_POINT('Ctrl Pts',(73.9352518610058,445.049149386145,48.2556830346191));
#36686=CARTESIAN_POINT('Ctrl Pts',(74.7456259311001,445.003292931703,48.1468535254144));
#36687=CARTESIAN_POINT('Ctrl Pts',(75.5333684099903,444.957436477262,48.2366220960433));
#36688=CARTESIAN_POINT('Ctrl Pts',(76.3211108888805,444.91158002282,48.3263906666722));
#36689=CARTESIAN_POINT('Ctrl Pts',(77.0862217765667,444.865723568378,48.6147573171347));
#36690=CARTESIAN_POINT('Ctrl Pts',(77.7372531005387,444.819867113937,49.0672557420249));
#36691=CARTESIAN_POINT('Ctrl Pts',(78.3882844245107,444.774010659495,49.5197541669151));
#36692=CARTESIAN_POINT('Ctrl Pts',(78.9252361847685,444.728154205053,50.1363843662331));
#36693=CARTESIAN_POINT('Ctrl Pts',(79.2839305600295,444.682297750611,50.8434451517932));
#36694=CARTESIAN_POINT('Ctrl Pts',(79.6426249352905,444.63644129617,51.5505059373534));
#36695=CARTESIAN_POINT('Ctrl Pts',(79.8230619255547,444.590584841728,52.3479973091559));
#36696=CARTESIAN_POINT('Ctrl Pts',(79.8036752491352,444.544728387286,53.1406010980052));
#36697=CARTESIAN_POINT('Ctrl Pts',(79.7842885727157,444.498871932844,53.9332048868545));
#36698=CARTESIAN_POINT('Ctrl Pts',(79.5650782296126,444.453015478403,54.7209210927507));
#36699=CARTESIAN_POINT('Ctrl Pts',(79.1722447899035,444.407159023961,55.4095998988477));
#36700=CARTESIAN_POINT('Ctrl Pts',(78.7794113501945,444.361302569519,56.0982787049447));
#36701=CARTESIAN_POINT('Ctrl Pts',(78.2129548138795,444.315446115077,56.6879201112425));
#36702=CARTESIAN_POINT('Ctrl Pts',(77.5405794870857,444.269589660636,57.1080486977965));
#36703=CARTESIAN_POINT('Ctrl Pts',(76.8682041602919,444.223733206194,57.5281772843504));
#36704=CARTESIAN_POINT('Ctrl Pts',(76.0899100430193,444.177876751752,57.7787930511605));
#36705=CARTESIAN_POINT('Ctrl Pts',(75.2987208004472,444.132020297311,57.8299417731297));
#36706=CARTESIAN_POINT('Ctrl Pts',(74.5075315578751,444.086163842869,57.8810904950989));
#36707=CARTESIAN_POINT('Ctrl Pts',(73.7034471900036,444.040307388427,57.7327721722273));
#36708=CARTESIAN_POINT('Ctrl Pts',(72.9825738774559,443.994450933985,57.4027141825081));
#36709=CARTESIAN_POINT('Ctrl Pts',(72.2617005649083,443.948594479544,57.0726561927889));
#36710=CARTESIAN_POINT('Ctrl Pts',(71.6240383076847,443.902738025102,56.560858536222));
#36711=CARTESIAN_POINT('Ctrl Pts',(71.1458020982885,443.85688157066,55.9284925525201));
#36712=CARTESIAN_POINT('Ctrl Pts',(70.6675658888923,443.811025116218,55.2961265688183));
#36713=CARTESIAN_POINT('Ctrl Pts',(70.3487557273236,443.765168661777,54.5431922579814));
#36714=CARTESIAN_POINT('Ctrl Pts',(70.2274766038005,443.719312207335,53.7596822175107));
#36715=CARTESIAN_POINT('Ctrl Pts',(70.1897688256036,443.705054642119,53.5160753875562));
#36716=CARTESIAN_POINT('Ctrl Pts',(70.1711562879823,443.690797076903,53.2695128149553));
#36717=CARTESIAN_POINT('Ctrl Pts',(70.1713650637522,443.676539511686,53.0229190193667));
#36718=CARTESIAN_POINT('Origin',(74.9879498948689,416.,53.0228109606356));
#36719=CARTESIAN_POINT('',(70.1711854681807,448.698460488313,53.022929878907));
#36720=CARTESIAN_POINT('',(70.1709464687216,447.176539511687,53.0227197042782));
#36721=CARTESIAN_POINT('',(70.1711998948689,416.,53.0228109606356));
#36722=CARTESIAN_POINT('Ctrl Pts',(70.1708091458866,446.948460488314,53.022773765229));
#36723=CARTESIAN_POINT('Ctrl Pts',(70.1711251047822,446.99216736906,53.7784606838785));
#36724=CARTESIAN_POINT('Ctrl Pts',(70.5418769104653,447.081730720163,55.3272999181237));
#36725=CARTESIAN_POINT('Ctrl Pts',(72.1299305918756,447.217150541622,57.1462208108926));
#36726=CARTESIAN_POINT('Ctrl Pts',(74.4263880163468,447.354719952691,58.0083331385092));
#36727=CARTESIAN_POINT('Ctrl Pts',(76.8570841007916,447.49228936376,57.6786804229088));
#36728=CARTESIAN_POINT('Ctrl Pts',(78.8409726637322,447.629858774829,56.236064556619));
#36729=CARTESIAN_POINT('Ctrl Pts',(79.9038147078087,447.767428185898,54.0253359081455));
#36730=CARTESIAN_POINT('Ctrl Pts',(79.7915429659626,447.904997596967,51.5749585037809));
#36731=CARTESIAN_POINT('Ctrl Pts',(78.5309954568607,448.042567008036,49.4706832496531));
#36732=CARTESIAN_POINT('Ctrl Pts',(76.423499985909,448.180136419105,48.2155270013095));
#36733=CARTESIAN_POINT('Ctrl Pts',(73.9728431859633,448.317705830174,48.1095288092612));
#36734=CARTESIAN_POINT('Ctrl Pts',(71.7648427513183,448.455275241243,49.1780270303383));
#36735=CARTESIAN_POINT('Ctrl Pts',(70.4386102196623,448.582193460623,51.0117160323741));
#36736=CARTESIAN_POINT('Ctrl Pts',(70.171791438985,448.663255209646,52.414097135008));
#36737=CARTESIAN_POINT('Ctrl Pts',(70.1711854681809,448.698460488314,53.022929878907));
#36738=CARTESIAN_POINT('Ctrl Pts',(70.1709464687216,447.176539511687,53.0227197042782));
#36739=CARTESIAN_POINT('Ctrl Pts',(70.1708561265147,447.170541771279,52.9190108868649));
#36740=CARTESIAN_POINT('Ctrl Pts',(70.1741384060741,447.164544030872,52.8153077803593));
#36741=CARTESIAN_POINT('Ctrl Pts',(70.1808329626729,447.158546290465,52.7118254233847));
#36742=CARTESIAN_POINT('Ctrl Pts',(70.2320170101361,447.112689836023,51.9206384653235));
#36743=CARTESIAN_POINT('Ctrl Pts',(70.4826675264911,447.066833381581,51.1423555384866));
#36744=CARTESIAN_POINT('Ctrl Pts',(70.9028261332883,447.020976927139,50.4699989705443));
#36745=CARTESIAN_POINT('Ctrl Pts',(71.3229847400855,446.975120472698,49.797642402602));
#36746=CARTESIAN_POINT('Ctrl Pts',(71.9126514373248,446.929264018256,49.2312121935544));
#36747=CARTESIAN_POINT('Ctrl Pts',(72.6013477822247,446.883407563814,48.8384095028275));
#36748=CARTESIAN_POINT('Ctrl Pts',(73.2900441271247,446.837551109372,48.4456068121006));
#36749=CARTESIAN_POINT('Ctrl Pts',(74.0777701196853,446.791694654931,48.2264316396944));
#36750=CARTESIAN_POINT('Ctrl Pts',(74.8703747733338,446.745838200489,48.2070803519968));
#36751=CARTESIAN_POINT('Ctrl Pts',(75.6629794269824,446.699981746047,48.1877290642992));
#36752=CARTESIAN_POINT('Ctrl Pts',(76.4604627417188,446.654125291606,48.3682016613101));
#36753=CARTESIAN_POINT('Ctrl Pts',(77.1675075113485,446.608268837164,48.726927605535));
#36754=CARTESIAN_POINT('Ctrl Pts',(77.8745522809783,446.562412382722,49.08565354976));
#36755=CARTESIAN_POINT('Ctrl Pts',(78.4911585055014,446.51655592828,49.6226328411989));
#36756=CARTESIAN_POINT('Ctrl Pts',(78.9436278622599,446.470699473839,50.2736843679735));
#36757=CARTESIAN_POINT('Ctrl Pts',(79.3960972190183,446.424843019397,50.924735894748));
#36758=CARTESIAN_POINT('Ctrl Pts',(79.6844297080122,446.378986564955,51.689859656858));
#36759=CARTESIAN_POINT('Ctrl Pts',(79.7741631069001,446.333130110513,52.4776061430101));
#36760=CARTESIAN_POINT('Ctrl Pts',(79.863896505788,446.287273656072,53.2653526291621));
#36761=CARTESIAN_POINT('Ctrl Pts',(79.7550308145699,446.24141720163,54.0757218393561));
#36762=CARTESIAN_POINT('Ctrl Pts',(79.4605779337402,446.195560747188,54.8118564128493));
#36763=CARTESIAN_POINT('Ctrl Pts',(79.1661250529105,446.149704292747,55.5479909863425));
#36764=CARTESIAN_POINT('Ctrl Pts',(78.6860849824693,446.103847838305,56.2098909231348));
#36765=CARTESIAN_POINT('Ctrl Pts',(78.0778333157743,446.057991383863,56.7184442824626));
#36766=CARTESIAN_POINT('Ctrl Pts',(77.4695816490793,446.012134929421,57.2269976417904));
#36767=CARTESIAN_POINT('Ctrl Pts',(76.7331183861305,445.96627847498,57.5822044236538));
#36768=CARTESIAN_POINT('Ctrl Pts',(75.9564674634694,445.920422020538,57.7416094224791));
#36769=CARTESIAN_POINT('Ctrl Pts',(75.1798165408083,445.874565566096,57.9010144213044));
#36770=CARTESIAN_POINT('Ctrl Pts',(74.3629779584348,445.828709111654,57.8646176370917));
#36771=CARTESIAN_POINT('Ctrl Pts',(73.6035823126826,445.782852657213,57.6367693047883));
#36772=CARTESIAN_POINT('Ctrl Pts',(72.8441866669304,445.736996202771,57.4089209724848));
#36773=CARTESIAN_POINT('Ctrl Pts',(72.1422339577995,445.691139748329,56.9896210920906));
#36774=CARTESIAN_POINT('Ctrl Pts',(71.5816233338722,445.645283293888,56.4289854370875));
#36775=CARTESIAN_POINT('Ctrl Pts',(71.0210127099449,445.599426839446,55.8683497820844));
#36776=CARTESIAN_POINT('Ctrl Pts',(70.6017441712213,445.553570385004,55.1663783524725));
#36777=CARTESIAN_POINT('Ctrl Pts',(70.3739297451482,445.507713930562,54.4069725343529));
#36778=CARTESIAN_POINT('Ctrl Pts',(70.2395051668771,445.480655790937,53.9588762105293));
#36779=CARTESIAN_POINT('Ctrl Pts',(70.1717397156061,445.453597651312,53.4907827910848));
#36780=CARTESIAN_POINT('Ctrl Pts',(70.1715262232373,445.426539511687,53.0227498862744));
#36781=CARTESIAN_POINT('Origin',(74.9879498948689,416.,53.0228109606356));
#36782=CARTESIAN_POINT('',(70.1715765014012,450.448460488314,53.022802847649));
#36783=CARTESIAN_POINT('',(70.1709848060094,448.926539511687,53.0229103046436));
#36784=CARTESIAN_POINT('',(70.1711998948689,416.,53.0228109606356));
#36785=CARTESIAN_POINT('Ctrl Pts',(70.1711854681809,448.698460488314,53.022929878907));
#36786=CARTESIAN_POINT('Ctrl Pts',(70.1710021345605,448.709111680003,53.2071293656684));
#36787=CARTESIAN_POINT('Ctrl Pts',(70.2260079845499,448.765619342048,54.1842522303751));
#36788=CARTESIAN_POINT('Ctrl Pts',(70.8718703381808,448.86798347445,55.8913771900424));
#36789=CARTESIAN_POINT('Ctrl Pts',(72.7237879497012,449.005552885519,57.4999030766785));
#36790=CARTESIAN_POINT('Ctrl Pts',(75.116942559506,449.143122296588,58.0382016754203));
#36791=CARTESIAN_POINT('Ctrl Pts',(77.4792620946565,449.280691707657,57.377595301182));
#36792=CARTESIAN_POINT('Ctrl Pts',(79.246045458165,449.418261118726,55.6759987231803));
#36793=CARTESIAN_POINT('Ctrl Pts',(79.9949516040101,449.555830529795,53.3401704006032));
#36794=CARTESIAN_POINT('Ctrl Pts',(79.5469581282337,449.693399940864,50.9284788337772));
#36795=CARTESIAN_POINT('Ctrl Pts',(78.0091557116053,449.830969351933,49.0174272658571));
#36796=CARTESIAN_POINT('Ctrl Pts',(75.7491486086294,449.968538763002,48.0638433616641));
#36797=CARTESIAN_POINT('Ctrl Pts',(73.3071806225934,450.10610817407,48.2956767566116));
#36798=CARTESIAN_POINT('Ctrl Pts',(71.2669924287125,450.24367758514,49.6575087952225));
#36799=CARTESIAN_POINT('Ctrl Pts',(70.3124472381403,450.35779502322,51.4545042986814));
#36800=CARTESIAN_POINT('Ctrl Pts',(70.1715533307098,450.426055990945,52.6352538315714));
#36801=CARTESIAN_POINT('Ctrl Pts',(70.1715765014014,450.448460488314,53.022802847649));
#36802=CARTESIAN_POINT('Ctrl Pts',(70.1709848060094,448.926539511687,53.0229103046436));
#36803=CARTESIAN_POINT('Ctrl Pts',(70.1716080264492,448.887485891247,52.3476063104968));
#36804=CARTESIAN_POINT('Ctrl Pts',(70.3150017485599,448.848432270807,51.672045946135));
#36805=CARTESIAN_POINT('Ctrl Pts',(70.5907335134134,448.809378650367,51.0556878585283));
#36806=CARTESIAN_POINT('Ctrl Pts',(70.9144955864482,448.763522195925,50.3319650321748));
#36807=CARTESIAN_POINT('Ctrl Pts',(71.4207157184263,448.717665741483,49.6898659950046));
#36808=CARTESIAN_POINT('Ctrl Pts',(72.0488892093647,448.671809287042,49.2061360345896));
#36809=CARTESIAN_POINT('Ctrl Pts',(72.6770627003032,448.6259528326,48.7224060741746));
#36810=CARTESIAN_POINT('Ctrl Pts',(73.4271895502019,448.580096378158,48.3970451905149));
#36811=CARTESIAN_POINT('Ctrl Pts',(74.2096127163334,448.534239923716,48.2689413325648));
#36812=CARTESIAN_POINT('Ctrl Pts',(74.9920358824648,448.488383469275,48.1408374746147));
#36813=CARTESIAN_POINT('Ctrl Pts',(75.806755364829,448.442527014833,48.2099906423743));
#36814=CARTESIAN_POINT('Ctrl Pts',(76.556393847241,448.396670560391,48.4681354757682));
#36815=CARTESIAN_POINT('Ctrl Pts',(77.306032329653,448.350814105949,48.7262803091621));
#36816=CARTESIAN_POINT('Ctrl Pts',(77.9905898121127,448.304957651508,49.1734168081904));
#36817=CARTESIAN_POINT('Ctrl Pts',(78.528246267164,448.259101197066,49.7561020968862));
#36818=CARTESIAN_POINT('Ctrl Pts',(79.0659027222152,448.213244742624,50.338787385582));
#36819=CARTESIAN_POINT('Ctrl Pts',(79.4566581498581,448.167388288183,51.0570214639455));
#36820=CARTESIAN_POINT('Ctrl Pts',(79.6538084812046,448.121531833741,51.824959193303));
#36821=CARTESIAN_POINT('Ctrl Pts',(79.8509588125512,448.075675379299,52.5928969226606));
#36822=CARTESIAN_POINT('Ctrl Pts',(79.8545040476015,448.029818924857,53.4105383030122));
#36823=CARTESIAN_POINT('Ctrl Pts',(79.6640204509694,447.983962470416,54.1801567855962));
#36824=CARTESIAN_POINT('Ctrl Pts',(79.4735368543374,447.938106015974,54.9497752681803));
#36825=CARTESIAN_POINT('Ctrl Pts',(79.089024426023,447.892249561532,55.6713708529968));
#36826=CARTESIAN_POINT('Ctrl Pts',(78.5564410559742,447.846393107091,56.2586966256889));
#36827=CARTESIAN_POINT('Ctrl Pts',(78.0238576859255,447.800536652649,56.846022398381));
#36828=CARTESIAN_POINT('Ctrl Pts',(77.3432033741424,447.754680198207,57.2990783589487));
#36829=CARTESIAN_POINT('Ctrl Pts',(76.5958316313312,447.708823743765,57.5637141225336));
#36830=CARTESIAN_POINT('Ctrl Pts',(75.8484598885199,447.662967289324,57.8283498861185));
#36831=CARTESIAN_POINT('Ctrl Pts',(75.0343707146806,447.617110834882,57.9045654527207));
#36832=CARTESIAN_POINT('Ctrl Pts',(74.2508660899421,447.57125438044,57.7832513466397));
#36833=CARTESIAN_POINT('Ctrl Pts',(73.4673614652036,447.525397925998,57.6619372405587));
#36834=CARTESIAN_POINT('Ctrl Pts',(72.7144413895659,447.479541471557,57.3430934617945));
#36835=CARTESIAN_POINT('Ctrl Pts',(72.0820967591035,447.433685017115,56.8648290185769));
#36836=CARTESIAN_POINT('Ctrl Pts',(71.4497521286412,447.387828562673,56.3865645753592));
#36837=CARTESIAN_POINT('Ctrl Pts',(70.9379829433542,447.341972108232,55.7488794676881));
#36838=CARTESIAN_POINT('Ctrl Pts',(70.6079571399963,447.29611565379,55.0279914192098));
#36839=CARTESIAN_POINT('Ctrl Pts',(70.3210966689862,447.256256939755,54.4013910654555));
#36840=CARTESIAN_POINT('Ctrl Pts',(70.1715468488558,447.216398225721,53.7119292757795));
#36841=CARTESIAN_POINT('Ctrl Pts',(70.1709464687216,447.176539511687,53.0227197042782));
#36842=CARTESIAN_POINT('Origin',(74.9879498948689,416.,53.0228109606356));
#36843=CARTESIAN_POINT('',(70.1711297808101,452.198460488313,53.0226941375257));
#36844=CARTESIAN_POINT('',(70.1715440079096,450.676539511686,53.0228609587722));
#36845=CARTESIAN_POINT('',(70.1711998948689,416.,53.0228109606356));
#36846=CARTESIAN_POINT('Ctrl Pts',(70.1715765014014,450.448460488314,53.022802847649));
#36847=CARTESIAN_POINT('Ctrl Pts',(70.1716007553904,450.471912461302,53.4284709109444));
#36848=CARTESIAN_POINT('Ctrl Pts',(70.3214916941221,450.541220904646,54.6273736565593));
#36849=CARTESIAN_POINT('Ctrl Pts',(71.3051976181603,450.656385818346,56.4298799059135));
#36850=CARTESIAN_POINT('Ctrl Pts',(73.3606205623162,450.793955229416,57.7686072450216));
#36851=CARTESIAN_POINT('Ctrl Pts',(75.8050487386511,450.931524640484,57.972874860119));
#36852=CARTESIAN_POINT('Ctrl Pts',(78.0541533753186,451.069094051554,56.9938535625169));
#36853=CARTESIAN_POINT('Ctrl Pts',(79.5702968510455,451.206663462622,55.065573673899));
#36854=CARTESIAN_POINT('Ctrl Pts',(79.9910523767396,451.344232873691,52.6489812060971));
#36855=CARTESIAN_POINT('Ctrl Pts',(79.2158403722948,451.48180228476,50.3217509390201));
#36856=CARTESIAN_POINT('Ctrl Pts',(77.4299715303552,451.619371695829,48.6401960492725));
#36857=CARTESIAN_POINT('Ctrl Pts',(75.0603491885598,451.756941106898,48.0062841270851));
#36858=CARTESIAN_POINT('Ctrl Pts',(72.6734201446142,451.894510517967,48.571548761583));
#36859=CARTESIAN_POINT('Ctrl Pts',(70.8397682799635,452.032079929036,50.2008661668549));
#36860=CARTESIAN_POINT('Ctrl Pts',(70.2196188326656,452.133396585818,51.8976271012186));
#36861=CARTESIAN_POINT('Ctrl Pts',(70.170963356447,452.188856772244,52.8566150075112));
#36862=CARTESIAN_POINT('Ctrl Pts',(70.1711297808103,452.198460488313,53.0226941375257));
#36863=CARTESIAN_POINT('Ctrl Pts',(70.1715440079096,450.676539511686,53.0228609587722));
#36864=CARTESIAN_POINT('Ctrl Pts',(70.1717127698825,450.650286465656,52.5687492006864));
#36865=CARTESIAN_POINT('Ctrl Pts',(70.2354503645211,450.624033419625,52.1145910364302));
#36866=CARTESIAN_POINT('Ctrl Pts',(70.3621002044194,450.597780373594,51.6787128073921));
#36867=CARTESIAN_POINT('Ctrl Pts',(70.5833207289459,450.551923919152,50.9173600055655));
#36868=CARTESIAN_POINT('Ctrl Pts',(70.9964862209847,450.50606746471,50.2117792010199));
#36869=CARTESIAN_POINT('Ctrl Pts',(71.5522141045377,450.460211010269,49.6463031814024));
#36870=CARTESIAN_POINT('Ctrl Pts',(72.1079419880908,450.414354555827,49.0808271617849));
#36871=CARTESIAN_POINT('Ctrl Pts',(72.8062322631582,450.368498101386,48.6554559270955));
#36872=CARTESIAN_POINT('Ctrl Pts',(73.5636235244637,450.322641646944,48.4210309143108));
#36873=CARTESIAN_POINT('Ctrl Pts',(74.3210147857691,450.276785192502,48.1866059015262));
#36874=CARTESIAN_POINT('Ctrl Pts',(75.1375070333125,450.23092873806,48.1431271106463));
#36875=CARTESIAN_POINT('Ctrl Pts',(75.915511065568,450.185072283619,48.29579123582));
#36876=CARTESIAN_POINT('Ctrl Pts',(76.6935150978235,450.139215829177,48.4484553609936));
#36877=CARTESIAN_POINT('Ctrl Pts',(77.4330309147911,450.093359374735,48.7972624022208));
#36878=CARTESIAN_POINT('Ctrl Pts',(78.045669731016,450.047502920294,49.3005220669819));
#36879=CARTESIAN_POINT('Ctrl Pts',(78.6583085472408,450.001646465852,49.8037817317431));
#36880=CARTESIAN_POINT('Ctrl Pts',(79.1440703627228,449.95579001141,50.4614940200382));
#36881=CARTESIAN_POINT('Ctrl Pts',(79.4448957067846,449.909933556968,51.1950475093565));
#36882=CARTESIAN_POINT('Ctrl Pts',(79.7457210508463,449.864077102526,51.9286009986747));
#36883=CARTESIAN_POINT('Ctrl Pts',(79.8616099234878,449.818220648085,52.7379956890161));
#36884=CARTESIAN_POINT('Ctrl Pts',(79.7787109959537,449.772364193643,53.526490696695));
#36885=CARTESIAN_POINT('Ctrl Pts',(79.6958120684197,449.726507739201,54.3149857043739));
#36886=CARTESIAN_POINT('Ctrl Pts',(79.4141253407101,449.68065128476,55.0825810293903));
#36887=CARTESIAN_POINT('Ctrl Pts',(78.9673187171074,449.634794830318,55.7375317530525));
#36888=CARTESIAN_POINT('Ctrl Pts',(78.5205120935046,449.588938375876,56.3924824767147));
#36889=CARTESIAN_POINT('Ctrl Pts',(77.9085855740088,449.543081921434,56.9347885990226));
#36890=CARTESIAN_POINT('Ctrl Pts',(77.2046781511943,449.497225466993,57.2996323319104));
#36891=CARTESIAN_POINT('Ctrl Pts',(76.5007707283798,449.451369012551,57.6644760647982));
#36892=CARTESIAN_POINT('Ctrl Pts',(75.7048824022466,449.405512558109,57.8518574082658));
#36893=CARTESIAN_POINT('Ctrl Pts',(74.9121397419505,449.359656103667,57.8393800741124));
#36894=CARTESIAN_POINT('Ctrl Pts',(74.1193970816544,449.313799649226,57.826902739959));
#36895=CARTESIAN_POINT('Ctrl Pts',(73.3298000871955,449.267943194784,57.6145667281844));
#36896=CARTESIAN_POINT('Ctrl Pts',(72.6377233719866,449.222086740342,57.2277509715424));
#36897=CARTESIAN_POINT('Ctrl Pts',(71.9456466567777,449.1762302859,56.8409352149004));
#36898=CARTESIAN_POINT('Ctrl Pts',(71.3510902208188,449.130373831459,56.2796397133909));
#36899=CARTESIAN_POINT('Ctrl Pts',(70.9251169407287,449.084517377017,55.6109519133151));
#36900=CARTESIAN_POINT('Ctrl Pts',(70.4991436606386,449.038660922575,54.9422641132394));
#36901=CARTESIAN_POINT('Ctrl Pts',(70.2417535364173,448.992804468134,54.1661840145974));
#36902=CARTESIAN_POINT('Ctrl Pts',(70.1837104813523,448.946948013692,53.375470657508));
#36903=CARTESIAN_POINT('Ctrl Pts',(70.1750997574451,448.94014517969,53.2581678311825));
#36904=CARTESIAN_POINT('Ctrl Pts',(70.1708762459027,448.933342345689,53.1405429574215));
#36905=CARTESIAN_POINT('Ctrl Pts',(70.1709848060094,448.926539511687,53.0229103046436));
#36906=CARTESIAN_POINT('Origin',(74.9879498948689,416.,53.0228109606356));
#36907=CARTESIAN_POINT('',(70.1708368207108,453.948460488313,53.0228652461544));
#36908=CARTESIAN_POINT('',(70.1713277050038,452.426539511687,53.0226981617181));
#36909=CARTESIAN_POINT('',(70.1711998948689,416.,53.0228109606356));
#36910=CARTESIAN_POINT('Ctrl Pts',(70.1711297808103,452.198460488313,53.0226941375257));
#36911=CARTESIAN_POINT('Ctrl Pts',(70.1717580107066,452.2347132426,53.6496208239294));
#36912=CARTESIAN_POINT('Ctrl Pts',(70.4504739081369,452.316822467244,55.0700956568864));
#36913=CARTESIAN_POINT('Ctrl Pts',(71.808425912791,452.444788162243,56.9037142545098));
#36914=CARTESIAN_POINT('Ctrl Pts',(74.0283409358903,452.582357573312,57.9472331376422));
#36915=CARTESIAN_POINT('Ctrl Pts',(76.4776458542147,452.719926984381,57.8135926372266));
#36916=CARTESIAN_POINT('Ctrl Pts',(78.5708461358004,452.85749639545,56.5347388738669));
#36917=CARTESIAN_POINT('Ctrl Pts',(79.8075723404659,452.995065806519,54.4163756677902));
#36918=CARTESIAN_POINT('Ctrl Pts',(79.8921910382349,453.132635217588,51.9648875470652));
#36919=CARTESIAN_POINT('Ctrl Pts',(78.8044745207126,453.270204628657,49.7662908954556));
#36920=CARTESIAN_POINT('Ctrl Pts',(76.8044362136501,453.407774039726,48.3461497189478));
#36921=CARTESIAN_POINT('Ctrl Pts',(74.3701755523407,453.545343450795,48.0439417574817));
#36922=CARTESIAN_POINT('Ctrl Pts',(72.0835909843443,453.682912861864,48.9319087309295));
#36923=CARTESIAN_POINT('Ctrl Pts',(70.5282839091672,453.817285207704,50.7544233060067));
#36924=CARTESIAN_POINT('Ctrl Pts',(70.1712626194858,453.905801083187,52.2852768041585));
#36925=CARTESIAN_POINT('Ctrl Pts',(70.170836820711,453.948460488313,53.0228652461544));
#36926=CARTESIAN_POINT('Ctrl Pts',(70.1713277050038,452.426539511687,53.0226981617181));
#36927=CARTESIAN_POINT('Ctrl Pts',(70.1711195125453,452.413087040065,52.7900341625413));
#36928=CARTESIAN_POINT('Ctrl Pts',(70.1876817062971,452.399634568443,52.5573995506344));
#36929=CARTESIAN_POINT('Ctrl Pts',(70.2212656740082,452.386182096821,52.327248783187));
#36930=CARTESIAN_POINT('Ctrl Pts',(70.3357458772472,452.34032564238,51.5427165069643));
#36931=CARTESIAN_POINT('Ctrl Pts',(70.648014834751,452.294469187938,50.7870458818604));
#36932=CARTESIAN_POINT('Ctrl Pts',(71.1207493774869,452.248612733496,50.1505565564186));
#36933=CARTESIAN_POINT('Ctrl Pts',(71.5934839202227,452.202756279055,49.5140672309767));
#36934=CARTESIAN_POINT('Ctrl Pts',(72.2266840481906,452.156899824613,48.996759205197));
#36935=CARTESIAN_POINT('Ctrl Pts',(72.944668093738,452.111043370171,48.6604624319896));
#36936=CARTESIAN_POINT('Ctrl Pts',(73.6626521392853,452.06518691573,48.3241656587821));
#36937=CARTESIAN_POINT('Ctrl Pts',(74.4654201024121,452.019330461288,48.1688801381469));
#36938=CARTESIAN_POINT('Ctrl Pts',(75.2570231425062,451.973474006846,48.213165985009));
#36939=CARTESIAN_POINT('Ctrl Pts',(76.0486261826002,451.927617552404,48.2574518318711));
#36940=CARTESIAN_POINT('Ctrl Pts',(76.8290642996615,451.881761097963,48.5013090462306));
#36941=CARTESIAN_POINT('Ctrl Pts',(77.5050575722715,451.835904643521,48.9155912021425));
#36942=CARTESIAN_POINT('Ctrl Pts',(78.1810508448815,451.790048189079,49.3298733580543));
#36943=CARTESIAN_POINT('Ctrl Pts',(78.7525992730403,451.744191734637,49.9145804555185));
#36944=CARTESIAN_POINT('Ctrl Pts',(79.1513899549379,451.698335280196,50.5998268355549));
#36945=CARTESIAN_POINT('Ctrl Pts',(79.5501806368354,451.652478825754,51.2850732155913));
#36946=CARTESIAN_POINT('Ctrl Pts',(79.7762135724718,451.606622371312,52.0708588781999));
#36947=CARTESIAN_POINT('Ctrl Pts',(79.8024727383945,451.560765916871,52.8632647499131));
#36948=CARTESIAN_POINT('Ctrl Pts',(79.8287319043172,451.514909462429,53.6556706216263));
#36949=CARTESIAN_POINT('Ctrl Pts',(79.6552173005262,451.469053007987,54.454696702444));
#36950=CARTESIAN_POINT('Ctrl Pts',(79.3026678277135,451.423196553545,55.1648413908988));
#36951=CARTESIAN_POINT('Ctrl Pts',(78.9501183549008,451.377340099104,55.8749860793536));
#36952=CARTESIAN_POINT('Ctrl Pts',(78.4185340130663,451.331483644662,56.4962493754455));
#36953=CARTESIAN_POINT('Ctrl Pts',(77.7714510961788,451.28562719022,56.9543763316412));
#36954=CARTESIAN_POINT('Ctrl Pts',(77.1243681792913,451.239770735778,57.4125032878369));
#36955=CARTESIAN_POINT('Ctrl Pts',(76.3617866873508,451.193914281337,57.7074939041364));
#36956=CARTESIAN_POINT('Ctrl Pts',(75.5748522731433,451.148057826895,57.8040901621213));
#36957=CARTESIAN_POINT('Ctrl Pts',(74.7879178589357,451.102201372453,57.9006864201062));
#36958=CARTESIAN_POINT('Ctrl Pts',(73.9766305224611,451.056344918012,57.7988883197764));
#36959=CARTESIAN_POINT('Ctrl Pts',(73.2379573612182,451.01048846357,57.5108630254351));
#36960=CARTESIAN_POINT('Ctrl Pts',(72.4992841999754,450.964632009128,57.2228377310937));
#36961=CARTESIAN_POINT('Ctrl Pts',(71.8332252139645,450.918775554686,56.7485852427409));
#36962=CARTESIAN_POINT('Ctrl Pts',(71.3193894439442,450.872919100245,56.1447894074054));
#36963=CARTESIAN_POINT('Ctrl Pts',(70.8055536739239,450.827062645803,55.5409935720698));
#36964=CARTESIAN_POINT('Ctrl Pts',(70.4439411198943,450.781206191361,54.8076543897516));
#36965=CARTESIAN_POINT('Ctrl Pts',(70.2777726213865,450.735349736919,54.0324223990388));
#36966=CARTESIAN_POINT('Ctrl Pts',(70.2067364067263,450.715746328508,53.7010145413626));
#36967=CARTESIAN_POINT('Ctrl Pts',(70.17141799168,450.696142920097,53.361950687542));
#36968=CARTESIAN_POINT('Ctrl Pts',(70.1715440079096,450.676539511686,53.0228609587722));
#36969=CARTESIAN_POINT('Origin',(74.9879498948689,416.,53.0228109606356));
#36970=CARTESIAN_POINT('',(70.1711998948689,455.,53.0228109606356));
#36971=CARTESIAN_POINT('',(70.170785177935,454.176539511687,53.0227998720929));
#36972=CARTESIAN_POINT('',(70.1711998948689,416.,53.0228109606356));
#36973=CARTESIAN_POINT('',(78.8686068361682,455.,50.1705810192547));
#36974=CARTESIAN_POINT('Origin',(74.9879498948689,455.,53.0228109606356));
#36975=CARTESIAN_POINT('Ctrl Pts',(70.170836820711,453.948460488313,53.0228652461544));
#36976=CARTESIAN_POINT('Ctrl Pts',(70.1708049096598,453.951657553543,53.0781430531125));
#36977=CARTESIAN_POINT('Ctrl Pts',(70.1851065053738,454.000711089129,53.9262705456493));
#36978=CARTESIAN_POINT('Ctrl Pts',(70.6550604420902,454.095621095071,55.5520112648156));
#36979=CARTESIAN_POINT('Ctrl Pts',(72.3720044217823,454.23319050614,57.3038901381464));
#36980=CARTESIAN_POINT('Ctrl Pts',(74.714270628573,454.370759917209,58.0323860252404));
#36981=CARTESIAN_POINT('Ctrl Pts',(77.1219697739619,454.508329328278,57.5633975942407));
#36982=CARTESIAN_POINT('Ctrl Pts',(79.0195060859316,454.645898739347,56.0089503824907));
#36983=CARTESIAN_POINT('Ctrl Pts',(79.9533662831374,454.783468150416,53.7408355040756));
#36984=CARTESIAN_POINT('Ctrl Pts',(79.7360467608705,454.901501903967,51.6473349742381));
#36985=CARTESIAN_POINT('Ctrl Pts',(79.1381333147689,454.973679187162,50.53747892867));
#36986=CARTESIAN_POINT('Ctrl Pts',(78.8686068361681,455.,50.1705810192548));
#36987=CARTESIAN_POINT('Ctrl Pts',(70.170785177935,454.176539511687,53.0227998720929));
#36988=CARTESIAN_POINT('Ctrl Pts',(70.1707835943913,454.175887614474,53.011528810388));
#36989=CARTESIAN_POINT('Ctrl Pts',(70.1708223389548,454.175235717261,53.0002577591952));
#36990=CARTESIAN_POINT('Ctrl Pts',(70.1709014783631,454.174583820049,52.9889869912234));
#36991=CARTESIAN_POINT('Ctrl Pts',(70.176468387687,454.128727365607,52.1961665157228));
#36992=CARTESIAN_POINT('Ctrl Pts',(70.3819149747748,454.082870911166,51.4047474592887));
#36993=CARTESIAN_POINT('Ctrl Pts',(70.7626840229485,454.037014456724,50.7093250836825));
#36994=CARTESIAN_POINT('Ctrl Pts',(71.1434530711222,453.991158002282,50.0139027080763));
#36995=CARTESIAN_POINT('Ctrl Pts',(71.6995445803816,453.94530154784,49.4144770132978));
#36996=CARTESIAN_POINT('Ctrl Pts',(72.3644939934935,453.899445093399,48.9826915707525));
#36997=CARTESIAN_POINT('Ctrl Pts',(73.0294434066053,453.853588638957,48.5509061282073));
#36998=CARTESIAN_POINT('Ctrl Pts',(73.8032507235696,453.807732184515,48.2867609378952));
#36999=CARTESIAN_POINT('Ctrl Pts',(74.593428185032,453.761875730073,48.221827889203));
#37000=CARTESIAN_POINT('Ctrl Pts',(75.3836056464944,453.716019275632,48.1568948405108));
#37001=CARTESIAN_POINT('Ctrl Pts',(76.1901532524549,453.67016282119,48.2911739334386));
#37002=CARTESIAN_POINT('Ctrl Pts',(76.9166705917121,453.624306366748,48.6086155257678));
#37003=CARTESIAN_POINT('Ctrl Pts',(77.6431879309693,453.578449912306,48.926057118097));
#37004=CARTESIAN_POINT('Ctrl Pts',(78.2896750035234,453.532593457865,49.4266612098278));
#37005=CARTESIAN_POINT('Ctrl Pts',(78.7788619752273,453.486737003423,50.0505944670632));
#37006=CARTESIAN_POINT('Ctrl Pts',(79.2680489469312,453.440880548981,50.6745277242986));
#37007=CARTESIAN_POINT('Ctrl Pts',(79.5999358177851,453.39502409454,51.4217901470387));
#37008=CARTESIAN_POINT('Ctrl Pts',(79.7348546736815,453.349167640098,52.2030670004071));
#37009=CARTESIAN_POINT('Ctrl Pts',(79.869773529578,453.303311185656,52.9843438537755));
#37010=CARTESIAN_POINT('Ctrl Pts',(79.8077243705171,453.257454731214,53.7996351377721));
#37011=CARTESIAN_POINT('Ctrl Pts',(79.5561234513778,453.211598276773,54.5514952184914));
#37012=CARTESIAN_POINT('Ctrl Pts',(79.3045225322384,453.165741822331,55.3033552992107));
#37013=CARTESIAN_POINT('Ctrl Pts',(78.8633698530205,453.119885367889,55.9917841766527));
#37014=CARTESIAN_POINT('Ctrl Pts',(78.2853930961865,453.074028913447,56.5344990929728));
#37015=CARTESIAN_POINT('Ctrl Pts',(77.7074163393524,453.028172459006,57.0772140092928));
#37016=CARTESIAN_POINT('Ctrl Pts',(76.9926155049022,452.982316004564,57.474214964491));
#37017=CARTESIAN_POINT('Ctrl Pts',(76.2264253781918,452.936459550122,57.6780514138309));
#37018=CARTESIAN_POINT('Ctrl Pts',(75.4602352514814,452.890603095681,57.8818878631709));
#37019=CARTESIAN_POINT('Ctrl Pts',(74.6426558325109,452.844746641239,57.8925598066526));
#37020=CARTESIAN_POINT('Ctrl Pts',(73.8714062658395,452.798890186797,57.7087917044262));
#37021=CARTESIAN_POINT('Ctrl Pts',(73.1001566991681,452.753033732355,57.5250236021999));
#37022=CARTESIAN_POINT('Ctrl Pts',(72.3752369847958,452.707177277914,57.1468154542655));
#37023=CARTESIAN_POINT('Ctrl Pts',(71.7832913446759,452.661320823472,56.6193716482587));
#37024=CARTESIAN_POINT('Ctrl Pts',(71.191345704556,452.61546436903,56.0919278422518));
#37025=CARTESIAN_POINT('Ctrl Pts',(70.7323741386884,452.569607914589,55.4152483781723));
#37026=CARTESIAN_POINT('Ctrl Pts',(70.4612340802417,452.523751460147,54.6702116824618));
#37027=CARTESIAN_POINT('Ctrl Pts',(70.2696358002897,452.491347477327,54.143739311625));
#37028=CARTESIAN_POINT('Ctrl Pts',(70.1718291938781,452.458943494507,53.583133481278));
#37029=CARTESIAN_POINT('Ctrl Pts',(70.1713277050038,452.426539511687,53.0226981617181));
#37030=CARTESIAN_POINT('Origin',(74.9879498948689,433.764859435991,53.0228109606356));
#37031=CARTESIAN_POINT('',(70.0693291699032,453.889859435991,53.0228663900751));
#37032=CARTESIAN_POINT('',(70.0692764388954,454.235140564009,53.0227996384331));
#37033=CARTESIAN_POINT('',(70.0696998948689,433.764859435991,53.0228109606359));
#37034=CARTESIAN_POINT('',(78.2551164949133,455.,49.3465621292785));
#37035=CARTESIAN_POINT('Ctrl Pts',(70.069329169903,453.88985943599,53.0228663900751));
#37036=CARTESIAN_POINT('Ctrl Pts',(70.0692965864127,453.89305650122,53.079309027553));
#37037=CARTESIAN_POINT('Ctrl Pts',(70.0838995496389,453.942110036806,53.9453085168704));
#37038=CARTESIAN_POINT('Ctrl Pts',(70.5637564965961,454.037020042748,55.6053073318474));
#37039=CARTESIAN_POINT('Ctrl Pts',(72.3168804345463,454.174589453817,57.394102321988));
#37040=CARTESIAN_POINT('Ctrl Pts',(74.708503577028,454.312158864886,58.1379492928087));
#37041=CARTESIAN_POINT('Ctrl Pts',(77.1669384806062,454.449728275955,57.6590781969942));
#37042=CARTESIAN_POINT('Ctrl Pts',(79.104460246599,454.587297687024,56.0718752075947));
#37043=CARTESIAN_POINT('Ctrl Pts',(80.0579990258397,454.724867098093,53.7559659325096));
#37044=CARTESIAN_POINT('Ctrl Pts',(79.7993775020766,454.862434535752,51.2645915204101));
#37045=CARTESIAN_POINT('Ctrl Pts',(78.8603576798458,454.954145503054,49.884454297563));
#37046=CARTESIAN_POINT('Ctrl Pts',(78.2551164948972,455.,49.3465621292932));
#37047=CARTESIAN_POINT('',(79.5259634688001,455.,54.9172708347097));
#37048=CARTESIAN_POINT('Origin',(74.9879498948689,455.,53.0228109606356));
#37049=CARTESIAN_POINT('Ctrl Pts',(70.0692764388952,454.23514056401,53.0227996384331));
#37050=CARTESIAN_POINT('Ctrl Pts',(70.0693885605861,454.280345121239,53.8208391932592));
#37051=CARTESIAN_POINT('Ctrl Pts',(70.4684746883736,454.37140613291,55.4285308409564));
#37052=CARTESIAN_POINT('Ctrl Pts',(72.1379853470107,454.508323599022,57.2796485035691));
#37053=CARTESIAN_POINT('Ctrl Pts',(74.4967427405941,454.645892962347,58.121944651965));
#37054=CARTESIAN_POINT('Ctrl Pts',(76.9728107558315,454.783462325672,57.745441606262));
#37055=CARTESIAN_POINT('Ctrl Pts',(78.6902915766538,454.90149800489,56.4535249040052));
#37056=CARTESIAN_POINT('Ctrl Pts',(79.3467648647433,454.973677229666,55.3462294167141));
#37057=CARTESIAN_POINT('Ctrl Pts',(79.5259634688003,455.,54.9172708347098));
#37058=CARTESIAN_POINT('Origin',(74.9879498948689,433.764859435991,53.0228109606356));
#37059=CARTESIAN_POINT('',(70.0696283033456,452.139859435991,53.0226916757941));
#37060=CARTESIAN_POINT('',(70.0698303982574,452.485140564009,53.0226957847854));
#37061=CARTESIAN_POINT('',(70.0696998948689,433.764859435991,53.0228109606359));
#37062=CARTESIAN_POINT('Ctrl Pts',(70.0696283033454,452.139859435991,53.0226916757941));
#37063=CARTESIAN_POINT('Ctrl Pts',(70.0702697714904,452.176112190277,53.6628291492784));
#37064=CARTESIAN_POINT('Ctrl Pts',(70.3548588538668,452.258221414921,55.1132366537557));
#37065=CARTESIAN_POINT('Ctrl Pts',(71.7414260302598,452.38618710992,56.9854938121638));
#37066=CARTESIAN_POINT('Ctrl Pts',(74.0081197682281,452.523756520989,58.0510020380353));
#37067=CARTESIAN_POINT('Ctrl Pts',(76.509037174062,452.661325932058,57.9145454249311));
#37068=CARTESIAN_POINT('Ctrl Pts',(78.646345999496,452.798895343127,56.6087432716859));
#37069=CARTESIAN_POINT('Ctrl Pts',(79.9091328695011,452.936464754196,54.4457412810724));
#37070=CARTESIAN_POINT('Ctrl Pts',(79.9955346778371,453.074034165265,51.9425946677425));
#37071=CARTESIAN_POINT('Ctrl Pts',(78.884897471774,453.211603576334,49.6976685283788));
#37072=CARTESIAN_POINT('Ctrl Pts',(76.842713757919,453.349172987403,48.2476017112594));
#37073=CARTESIAN_POINT('Ctrl Pts',(74.357157626194,453.486742398472,47.9390255330312));
#37074=CARTESIAN_POINT('Ctrl Pts',(72.0223894626918,453.624311809541,48.8457040127446));
#37075=CARTESIAN_POINT('Ctrl Pts',(70.4343084905653,453.75868415538,50.7066231613146));
#37076=CARTESIAN_POINT('Ctrl Pts',(70.0697639412373,453.847200030864,52.2697352633099));
#37077=CARTESIAN_POINT('Ctrl Pts',(70.069329169903,453.88985943599,53.0228663900751));
#37078=CARTESIAN_POINT('Ctrl Pts',(70.0698303982571,452.485140564009,53.0226957847854));
#37079=CARTESIAN_POINT('Ctrl Pts',(70.0703424546553,452.517544546829,53.5949407654106));
#37080=CARTESIAN_POINT('Ctrl Pts',(70.3115375997815,452.595804984091,54.9774179780456));
#37081=CARTESIAN_POINT('Ctrl Pts',(71.5799856751815,452.719921875795,56.8475398498696));
#37082=CARTESIAN_POINT('Ctrl Pts',(73.8005719949271,452.85749123912,58.0060734400985));
#37083=CARTESIAN_POINT('Ctrl Pts',(76.304995087688,452.995060602445,57.9733829624763));
#37084=CARTESIAN_POINT('Ctrl Pts',(78.4945850834537,453.13262996577,56.7572829274506));
#37085=CARTESIAN_POINT('Ctrl Pts',(79.8459314256328,453.270199329095,54.6484759560617));
#37086=CARTESIAN_POINT('Ctrl Pts',(80.0360014582592,453.407768692421,52.1510619170208));
#37087=CARTESIAN_POINT('Ctrl Pts',(79.0193599867834,453.545338055746,49.8620350354254));
#37088=CARTESIAN_POINT('Ctrl Pts',(77.0390298609172,453.682907419071,48.3285761217461));
#37089=CARTESIAN_POINT('Ctrl Pts',(74.5683996041992,453.820476782396,47.9172501350589));
#37090=CARTESIAN_POINT('Ctrl Pts',(72.1980599540245,453.958046145721,48.726384145908));
#37091=CARTESIAN_POINT('Ctrl Pts',(70.4946310452694,454.095615509047,50.562555064065));
#37092=CARTESIAN_POINT('Ctrl Pts',(70.0720972254101,454.187980315143,52.1902351426901));
#37093=CARTESIAN_POINT('Ctrl Pts',(70.0692748219826,454.234488666797,53.0112910695366));
#37094=CARTESIAN_POINT('Ctrl Pts',(70.0692764388952,454.23514056401,53.0227996384331));
#37095=CARTESIAN_POINT('Origin',(74.9879498948689,433.764859435991,53.0228109606356));
#37096=CARTESIAN_POINT('',(70.0700844373669,450.389859435991,53.0228026766897));
#37097=CARTESIAN_POINT('',(70.0700512591628,450.735140564009,53.0228620123491));
#37098=CARTESIAN_POINT('',(70.0696998948689,433.764859435991,53.0228109606359));
#37099=CARTESIAN_POINT('Ctrl Pts',(70.0700844373667,450.389859435991,53.0228026766897));
#37100=CARTESIAN_POINT('Ctrl Pts',(70.070109202443,450.413311408979,53.4370190990291));
#37101=CARTESIAN_POINT('Ctrl Pts',(70.2231586879711,450.482619852323,54.6611854827153));
#37102=CARTESIAN_POINT('Ctrl Pts',(71.2275935581432,450.597784766023,56.5016746841243));
#37103=CARTESIAN_POINT('Ctrl Pts',(73.326328990768,450.735354177093,57.8686120870556));
#37104=CARTESIAN_POINT('Ctrl Pts',(75.8222668904432,450.872923588161,58.0771840905751));
#37105=CARTESIAN_POINT('Ctrl Pts',(78.1187653342674,451.01049299923,57.0775325626919));
#37106=CARTESIAN_POINT('Ctrl Pts',(79.6668574398354,451.148062410299,55.1086193821872));
#37107=CARTESIAN_POINT('Ctrl Pts',(80.096479252104,451.285631821368,52.6411037534401));
#37108=CARTESIAN_POINT('Ctrl Pts',(79.304931747903,451.423201232437,50.2648333925011));
#37109=CARTESIAN_POINT('Ctrl Pts',(77.4814305423453,451.560770643506,48.547844274008));
#37110=CARTESIAN_POINT('Ctrl Pts',(75.0618748081809,451.698340054575,47.9005743697575));
#37111=CARTESIAN_POINT('Ctrl Pts',(72.6246476798502,451.835909465644,48.4777504300927));
#37112=CARTESIAN_POINT('Ctrl Pts',(70.7523565534021,451.973478876713,50.1414013001772));
#37113=CARTESIAN_POINT('Ctrl Pts',(70.1191391310378,452.074795533495,51.8739168896172));
#37114=CARTESIAN_POINT('Ctrl Pts',(70.069458372038,452.130255719921,52.8531128765635));
#37115=CARTESIAN_POINT('Ctrl Pts',(70.0696283033454,452.139859435991,53.0226916757941));
#37116=CARTESIAN_POINT('Ctrl Pts',(70.0700512591626,450.735140564009,53.0228620123491));
#37117=CARTESIAN_POINT('Ctrl Pts',(70.0699225874812,450.75474397242,53.3690971415379));
#37118=CARTESIAN_POINT('Ctrl Pts',(70.1903433030529,450.820203835273,54.5251601145759));
#37119=CARTESIAN_POINT('Ctrl Pts',(71.0866535291021,450.931520152567,56.3428497963907));
#37120=CARTESIAN_POINT('Ctrl Pts',(73.1269366710226,451.069089515892,57.7955880332776));
#37121=CARTESIAN_POINT('Ctrl Pts',(75.6120857503499,451.206658879218,58.1074176945308));
#37122=CARTESIAN_POINT('Ctrl Pts',(77.9480382636025,451.344228242543,57.2037974535288));
#37123=CARTESIAN_POINT('Ctrl Pts',(79.5763964029459,451.481797605868,55.300733225987));
#37124=CARTESIAN_POINT('Ctrl Pts',(80.1079092695645,451.619366969193,52.8531430321954));
#37125=CARTESIAN_POINT('Ctrl Pts',(79.4155213613108,451.756936332518,50.4461111112164));
#37126=CARTESIAN_POINT('Ctrl Pts',(77.6647445573712,451.894505695844,48.6550264490875));
#37127=CARTESIAN_POINT('Ctrl Pts',(75.2740933282832,452.032075059169,47.9080389090301));
#37128=CARTESIAN_POINT('Ctrl Pts',(72.8150409373668,452.169644422494,48.3837121400662));
#37129=CARTESIAN_POINT('Ctrl Pts',(70.8754116046977,452.307213785819,49.96833882681));
#37130=CARTESIAN_POINT('Ctrl Pts',(70.1441754893215,452.412379166324,51.7378828020483));
#37131=CARTESIAN_POINT('Ctrl Pts',(70.0696178187047,452.471688092388,52.7851290200683));
#37132=CARTESIAN_POINT('Ctrl Pts',(70.0698303982571,452.485140564009,53.0226957847854));
#37133=CARTESIAN_POINT('Origin',(74.9879498948689,433.764859435991,53.0228109606356));
#37134=CARTESIAN_POINT('',(70.0696851641772,448.639859435991,53.0229323847884));
#37135=CARTESIAN_POINT('',(70.0694802735924,448.985140564009,53.0229123980504));
#37136=CARTESIAN_POINT('',(70.0696998948689,433.764859435991,53.0228109606359));
#37137=CARTESIAN_POINT('Ctrl Pts',(70.0696851641769,448.639859435991,53.0229323847884));
#37138=CARTESIAN_POINT('Ctrl Pts',(70.0694979672956,448.65051062768,53.2110133783555));
#37139=CARTESIAN_POINT('Ctrl Pts',(70.125662917046,448.707018289725,54.2087264689964));
#37140=CARTESIAN_POINT('Ctrl Pts',(70.7851350758139,448.809382422127,55.9518244775881));
#37141=CARTESIAN_POINT('Ctrl Pts',(72.6760768504256,448.946951833196,57.594245703923));
#37142=CARTESIAN_POINT('Ctrl Pts',(75.1196607316056,449.084521244265,58.1438874921126));
#37143=CARTESIAN_POINT('Ctrl Pts',(77.5317597721941,449.222090655334,57.469360622315));
#37144=CARTESIAN_POINT('Ctrl Pts',(79.3357733243977,449.359660066403,55.7319074911046));
#37145=CARTESIAN_POINT('Ctrl Pts',(80.1004606450606,449.497229477472,53.3468578938625));
#37146=CARTESIAN_POINT('Ctrl Pts',(79.6430269164599,449.634798888541,50.8843464393459));
#37147=CARTESIAN_POINT('Ctrl Pts',(78.0728194662947,449.77236829961,48.9330246198776));
#37148=CARTESIAN_POINT('Ctrl Pts',(75.7651888161234,449.909937710679,47.9593465097831));
#37149=CARTESIAN_POINT('Ctrl Pts',(73.2717629486147,450.047507121747,48.1960651675296));
#37150=CARTESIAN_POINT('Ctrl Pts',(71.1885832974899,450.185076532817,49.586594139118));
#37151=CARTESIAN_POINT('Ctrl Pts',(70.2139236445014,450.299193970897,51.4214564705422));
#37152=CARTESIAN_POINT('Ctrl Pts',(70.0700607784154,450.367454938622,52.627087111563));
#37153=CARTESIAN_POINT('Ctrl Pts',(70.0700844373667,450.389859435991,53.0228026766897));
#37154=CARTESIAN_POINT('Ctrl Pts',(70.0694802735922,448.985140564009,53.0229123980504));
#37155=CARTESIAN_POINT('Ctrl Pts',(70.0693694258745,448.991943398011,53.1430238413523));
#37156=CARTESIAN_POINT('Ctrl Pts',(70.102751651847,449.044602686455,54.0727194457198));
#37157=CARTESIAN_POINT('Ctrl Pts',(70.6673681160653,449.14311842934,55.7751452966382));
#37158=CARTESIAN_POINT('Ctrl Pts',(72.4886234383188,449.280687792665,57.4945151623977));
#37159=CARTESIAN_POINT('Ctrl Pts',(74.9073302954306,449.41825715599,58.1449464220086));
#37160=CARTESIAN_POINT('Ctrl Pts',(77.3453088660466,449.555826519316,57.5709567240733));
#37161=CARTESIAN_POINT('Ctrl Pts',(79.2197725217338,449.693395882641,55.9097554455925));
#37162=CARTESIAN_POINT('Ctrl Pts',(80.0826400663797,449.830965245966,53.5584444741309));
#37163=CARTESIAN_POINT('Ctrl Pts',(79.7276473132564,449.968534609291,51.0790929804237));
#37164=CARTESIAN_POINT('Ctrl Pts',(78.2396535110072,450.106103972616,49.0643775840001));
#37165=CARTESIAN_POINT('Ctrl Pts',(75.9743561631267,450.243673335941,47.9959059606967));
#37166=CARTESIAN_POINT('Ctrl Pts',(73.4732633122539,450.381242699267,48.1290909276837));
#37167=CARTESIAN_POINT('Ctrl Pts',(71.3342487410075,450.518812062591,49.4320952822867));
#37168=CARTESIAN_POINT('Ctrl Pts',(70.2489813568954,450.636778017506,51.2854539213402));
#37169=CARTESIAN_POINT('Ctrl Pts',(70.0702235773382,450.708887517979,52.5591810751596));
#37170=CARTESIAN_POINT('Ctrl Pts',(70.0700512591626,450.735140564009,53.0228620123491));
#37171=CARTESIAN_POINT('Origin',(74.9879498948689,433.764859435991,53.0228109606356));
#37172=CARTESIAN_POINT('',(70.0693009119067,446.889859435991,53.0227729814362));
#37173=CARTESIAN_POINT('',(70.0694411284499,447.235140564009,53.0227177812969));
#37174=CARTESIAN_POINT('',(70.0696998948689,433.764859435991,53.0228109606359));
#37175=CARTESIAN_POINT('Ctrl Pts',(70.0693009119065,446.889859435991,53.0227729814362));
#37176=CARTESIAN_POINT('Ctrl Pts',(70.0696235287826,446.933566316737,53.7943839613808));
#37177=CARTESIAN_POINT('Ctrl Pts',(70.4481879276617,447.02312966784,55.3758608002924));
#37178=CARTESIAN_POINT('Ctrl Pts',(72.069705552325,447.158549489299,57.2331105394031));
#37179=CARTESIAN_POINT('Ctrl Pts',(74.4145546160935,447.296118900368,58.1133895564375));
#37180=CARTESIAN_POINT('Ctrl Pts',(76.8964710571215,447.433688311437,57.7767902999883));
#37181=CARTESIAN_POINT('Ctrl Pts',(78.9221647146049,447.571257722506,56.3037751996861));
#37182=CARTESIAN_POINT('Ctrl Pts',(80.0074032848607,447.708827133575,54.0464614143837));
#37183=CARTESIAN_POINT('Ctrl Pts',(79.8927657192128,447.846396544644,51.5444489227623));
#37184=CARTESIAN_POINT('Ctrl Pts',(78.605655575103,447.983965955713,49.3958317496446));
#37185=CARTESIAN_POINT('Ctrl Pts',(76.4537503277871,448.121535366782,48.1142264725559));
#37186=CARTESIAN_POINT('Ctrl Pts',(73.9514525530772,448.259104777851,48.0059946548279));
#37187=CARTESIAN_POINT('Ctrl Pts',(71.6969244713428,448.39667418892,49.0970085907417));
#37188=CARTESIAN_POINT('Ctrl Pts',(70.3427451701921,448.5235924083,50.969337637145));
#37189=CARTESIAN_POINT('Ctrl Pts',(70.0703039041795,448.604654157323,52.4012701347896));
#37190=CARTESIAN_POINT('Ctrl Pts',(70.0696851641769,448.639859435991,53.0229323847884));
#37191=CARTESIAN_POINT('Ctrl Pts',(70.0694411284497,447.235140564009,53.0227177812969));
#37192=CARTESIAN_POINT('Ctrl Pts',(70.0700541599741,447.274999278044,53.7264505835051));
#37193=CARTESIAN_POINT('Ctrl Pts',(70.3984342289788,447.36071444652,55.2403642068889));
#37194=CARTESIAN_POINT('Ctrl Pts',(71.8977475035859,447.492286069438,57.1085691993689));
#37195=CARTESIAN_POINT('Ctrl Pts',(74.204105003148,447.629855432763,58.0852568507357));
#37196=CARTESIAN_POINT('Ctrl Pts',(76.6978367180401,447.767424796088,57.8517920391255));
#37197=CARTESIAN_POINT('Ctrl Pts',(78.7828285085176,447.904994159413,56.463983364358));
#37198=CARTESIAN_POINT('Ctrl Pts',(79.9606734769448,448.042563522738,54.2535795744433));
#37199=CARTESIAN_POINT('Ctrl Pts',(79.9498136530265,448.180132886064,51.7489666805328));
#37200=CARTESIAN_POINT('Ctrl Pts',(78.7528450235537,448.317702249389,49.5488599139924));
#37201=CARTESIAN_POINT('Ctrl Pts',(76.6558969746985,448.455271612714,48.1791838338476));
#37202=CARTESIAN_POINT('Ctrl Pts',(74.1602344880813,448.592840976039,47.9673526817221));
#37203=CARTESIAN_POINT('Ctrl Pts',(71.8624332448065,448.730410339365,48.9640036389398));
#37204=CARTESIAN_POINT('Ctrl Pts',(70.3884517474718,448.861176868688,50.833629203903));
#37205=CARTESIAN_POINT('Ctrl Pts',(70.07011662672,448.946086943569,52.3333781956913));
#37206=CARTESIAN_POINT('Ctrl Pts',(70.0694802735922,448.985140564009,53.0229123980504));
#37207=CARTESIAN_POINT('Origin',(74.9879498948689,433.764859435991,53.0228109606356));
#37208=CARTESIAN_POINT('',(70.0698995811618,445.139859435991,53.0227057881612));
#37209=CARTESIAN_POINT('',(70.0700330997265,445.485140564009,53.0227485992971));
#37210=CARTESIAN_POINT('',(70.0696998948689,433.764859435991,53.0228109606359));
#37211=CARTESIAN_POINT('Ctrl Pts',(70.0698995811616,445.139859435991,53.0227057881612));
#37212=CARTESIAN_POINT('Ctrl Pts',(70.0703358154751,445.170765535438,53.5685206225869));
#37213=CARTESIAN_POINT('Ctrl Pts',(70.2955540358443,445.247528105242,54.9245313476707));
#37214=CARTESIAN_POINT('Ctrl Pts',(71.5187244149973,445.370147145402,56.7920611719599));
#37215=CARTESIAN_POINT('Ctrl Pts',(73.7203319129862,445.507716556471,57.9862691540494));
#37216=CARTESIAN_POINT('Ctrl Pts',(76.2249573788151,445.64528596754,57.9939863820444));
#37217=CARTESIAN_POINT('Ctrl Pts',(78.4338821687736,445.782855378609,56.813368089795));
#37218=CARTESIAN_POINT('Ctrl Pts',(79.8190734602514,445.920424789678,54.7266353887282));
#37219=CARTESIAN_POINT('Ctrl Pts',(80.0494079525281,446.057994200747,52.2326116716488));
#37220=CARTESIAN_POINT('Ctrl Pts',(79.0698252955847,446.195563611816,49.927481285336));
#37221=CARTESIAN_POINT('Ctrl Pts',(77.1144900013488,446.333133022885,48.3622745364359));
#37222=CARTESIAN_POINT('Ctrl Pts',(74.6508155459415,446.470702433954,47.9111465529761));
#37223=CARTESIAN_POINT('Ctrl Pts',(72.2677314314422,446.608271845023,48.6819373046774));
#37224=CARTESIAN_POINT('Ctrl Pts',(70.5349024274333,446.745841256092,50.4903929780497));
#37225=CARTESIAN_POINT('Ctrl Pts',(70.0788928230404,446.839703786414,52.1373220589989));
#37226=CARTESIAN_POINT('Ctrl Pts',(70.0692850449795,446.887709846381,52.9848236490411));
#37227=CARTESIAN_POINT('Ctrl Pts',(70.0693009119065,446.889859435991,53.0227729814362));
#37228=CARTESIAN_POINT('Ctrl Pts',(70.0700330997263,445.485140564009,53.0227485992971));
#37229=CARTESIAN_POINT('Ctrl Pts',(70.0702510908703,445.512198703635,53.500644033788));
#37230=CARTESIAN_POINT('Ctrl Pts',(70.2567092353932,445.585113297702,54.7886134756791));
#37231=CARTESIAN_POINT('Ctrl Pts',(71.3655237114099,445.70388434621,56.6450754112051));
#37232=CARTESIAN_POINT('Ctrl Pts',(73.5157571125727,445.841453709536,57.9294818907289));
#37233=CARTESIAN_POINT('Ctrl Pts',(76.0179108621497,445.979023072861,58.0409731352117));
#37234=CARTESIAN_POINT('Ctrl Pts',(78.2738575749735,446.116592436186,56.95289771824));
#37235=CARTESIAN_POINT('Ctrl Pts',(79.7443244311198,446.254161799511,54.9253546461714));
#37236=CARTESIAN_POINT('Ctrl Pts',(80.0778036562199,446.391731162836,52.4430179867826));
#37237=CARTESIAN_POINT('Ctrl Pts',(79.1945787032988,446.529300526162,50.0992779485839));
#37238=CARTESIAN_POINT('Ctrl Pts',(77.3057800960881,446.666869889487,48.4543939084407));
#37239=CARTESIAN_POINT('Ctrl Pts',(74.8629157294284,446.804439252812,47.9015671994052));
#37240=CARTESIAN_POINT('Ctrl Pts',(72.4499401569502,446.942008616137,48.5729482914402));
#37241=CARTESIAN_POINT('Ctrl Pts',(70.643663164976,447.079577979463,50.308046880104));
#37242=CARTESIAN_POINT('Ctrl Pts',(70.0983242060101,447.177288628753,52.0013527917544));
#37243=CARTESIAN_POINT('Ctrl Pts',(70.0693488825247,447.229142823602,52.9168235805925));
#37244=CARTESIAN_POINT('Ctrl Pts',(70.0694411284497,447.235140564009,53.0227177812969));
#37245=CARTESIAN_POINT('Origin',(74.9879498948689,433.764859435991,53.0228109606356));
#37246=CARTESIAN_POINT('',(70.0700145679607,443.389859435991,53.0228825250668));
#37247=CARTESIAN_POINT('',(70.0698685442404,443.735140564009,53.0229212964126));
#37248=CARTESIAN_POINT('',(70.0696998948689,433.764859435991,53.0228109606359));
#37249=CARTESIAN_POINT('Ctrl Pts',(70.0700145679605,443.389859435991,53.0228825250668));
#37250=CARTESIAN_POINT('Ctrl Pts',(70.0698463414395,443.407964754139,53.342651567647));
#37251=CARTESIAN_POINT('Ctrl Pts',(70.178392996224,443.471926542644,54.4722069068458));
#37252=CARTESIAN_POINT('Ctrl Pts',(71.0335914159785,443.581744801505,56.279469003198));
#37253=CARTESIAN_POINT('Ctrl Pts',(73.0501694171724,443.719314212574,57.7649391122166));
#37254=CARTESIAN_POINT('Ctrl Pts',(75.5299645002191,443.856883623643,58.1168263466887));
#37255=CARTESIAN_POINT('Ctrl Pts',(77.8801936047136,443.994453034712,57.2510137595351));
#37256=CARTESIAN_POINT('Ctrl Pts',(79.5390457928333,444.132022445781,55.3744696759449));
#37257=CARTESIAN_POINT('Ctrl Pts',(80.1099804457359,444.26959185685,52.9357729129582));
#37258=CARTESIAN_POINT('Ctrl Pts',(79.4565183869152,444.407161267919,50.5178821756897));
#37259=CARTESIAN_POINT('Ctrl Pts',(77.7348665714272,444.544730678988,48.6987825891046));
#37260=CARTESIAN_POINT('Ctrl Pts',(75.3565775663022,444.682300090057,47.9133211401532));
#37261=CARTESIAN_POINT('Ctrl Pts',(72.8901698933421,444.819869501126,48.3492586017812));
#37262=CARTESIAN_POINT('Ctrl Pts',(70.9252264171065,444.957438912195,49.9023862252835));
#37263=CARTESIAN_POINT('Ctrl Pts',(70.1547157841456,445.064102223817,51.6849358258267));
#37264=CARTESIAN_POINT('Ctrl Pts',(70.0696885592305,445.124909065082,52.7586758921829));
#37265=CARTESIAN_POINT('Ctrl Pts',(70.0698995811616,445.139859435991,53.0227057881612));
#37266=CARTESIAN_POINT('Ctrl Pts',(70.0698685442402,443.735140564009,53.0229212964126));
#37267=CARTESIAN_POINT('Ctrl Pts',(70.0696553690848,443.749398129226,53.2747113903876));
#37268=CARTESIAN_POINT('Ctrl Pts',(70.1497848787881,443.809512148883,54.336196850122));
#37269=CARTESIAN_POINT('Ctrl Pts',(70.9020536867909,443.915482622983,56.1128309251798));
#37270=CARTESIAN_POINT('Ctrl Pts',(72.8553514892035,444.053051986308,57.6805781558292));
#37271=CARTESIAN_POINT('Ctrl Pts',(75.3184363133803,444.190621349633,58.1349093489344));
#37272=CARTESIAN_POINT('Ctrl Pts',(77.7025200060835,444.328190712959,57.3672188967954));
#37273=CARTESIAN_POINT('Ctrl Pts',(79.4376992408775,444.465760076284,55.5610193764604));
#37274=CARTESIAN_POINT('Ctrl Pts',(80.1091880683859,444.603329439609,53.1480737826581));
#37275=CARTESIAN_POINT('Ctrl Pts',(79.5564704305387,444.740898802934,50.7051847354578));
#37276=CARTESIAN_POINT('Ctrl Pts',(77.9116707243749,444.878468166259,48.8163126882502));
#37277=CARTESIAN_POINT('Ctrl Pts',(75.567970123329,445.016037529584,47.9329830913412));
#37278=CARTESIAN_POINT('Ctrl Pts',(73.0856185770117,445.15360689291,48.2663514830863));
#37279=CARTESIAN_POINT('Ctrl Pts',(71.0580098525792,445.291176256235,49.7367278106718));
#37280=CARTESIAN_POINT('Ctrl Pts',(70.1838640833086,445.401687479935,51.5489195429218));
#37281=CARTESIAN_POINT('Ctrl Pts',(70.0698816530189,445.466342249193,52.6907365337478));
#37282=CARTESIAN_POINT('Ctrl Pts',(70.0700330997263,445.485140564009,53.0227485992971));
#37283=CARTESIAN_POINT('Origin',(74.9879498948689,433.764859435991,53.0228109606356));
#37284=CARTESIAN_POINT('',(70.0694094802036,441.639859435991,53.0228960008483));
#37285=CARTESIAN_POINT('',(70.0692875054394,441.985140564009,53.0228369856911));
#37286=CARTESIAN_POINT('',(70.0696998948689,433.764859435991,53.0228109606359));
#37287=CARTESIAN_POINT('Ctrl Pts',(70.0694094802034,441.639859435991,53.0228960008483));
#37288=CARTESIAN_POINT('Ctrl Pts',(70.0693331272471,441.64516397284,53.1165494736883));
#37289=CARTESIAN_POINT('Ctrl Pts',(70.0946128328825,441.696324980046,54.0197739441058));
#37290=CARTESIAN_POINT('Ctrl Pts',(70.6235146926476,441.793342457608,55.7050633632576));
#37291=CARTESIAN_POINT('Ctrl Pts',(72.4167872452805,441.930911868677,57.4536004179581));
#37292=CARTESIAN_POINT('Ctrl Pts',(74.8246838346499,442.068481279746,58.1429786121231));
#37293=CARTESIAN_POINT('Ctrl Pts',(77.2716083886679,442.206050690815,57.608405411681));
#37294=CARTESIAN_POINT('Ctrl Pts',(79.1726353884369,442.343620101884,55.9776679632129));
#37295=CARTESIAN_POINT('Ctrl Pts',(80.0733334938275,442.481189512953,53.6405861925782));
#37296=CARTESIAN_POINT('Ctrl Pts',(79.7583951646866,442.618758924023,51.1558282308192));
#37297=CARTESIAN_POINT('Ctrl Pts',(78.3031048903914,442.756328335091,49.1173634905726));
#37298=CARTESIAN_POINT('Ctrl Pts',(76.0553427955826,442.89389774616,48.0124771412913));
#37299=CARTESIAN_POINT('Ctrl Pts',(73.5524255733744,443.031467157229,48.1052869385125));
#37300=CARTESIAN_POINT('Ctrl Pts',(71.3926635200745,443.169036568298,49.3736071476132));
#37301=CARTESIAN_POINT('Ctrl Pts',(70.2634714560322,443.288500661219,51.232524664295));
#37302=CARTESIAN_POINT('Ctrl Pts',(70.0702724192588,443.362108283783,52.5327525367852));
#37303=CARTESIAN_POINT('Ctrl Pts',(70.0700145679605,443.389859435991,53.0228825250668));
#37304=CARTESIAN_POINT('Ctrl Pts',(70.0692875054392,441.985140564009,53.0228369856911));
#37305=CARTESIAN_POINT('Ctrl Pts',(70.0692798613491,441.986597554817,53.0485588210285));
#37306=CARTESIAN_POINT('Ctrl Pts',(70.0756977175085,442.033911000065,53.8838304412508));
#37307=CARTESIAN_POINT('Ctrl Pts',(70.5161341059696,442.127080899755,55.5219377590632));
#37308=CARTESIAN_POINT('Ctrl Pts',(72.2354226533932,442.264650263081,57.3432698470737));
#37309=CARTESIAN_POINT('Ctrl Pts',(74.6126891215678,442.402219626406,58.1318177678819));
#37310=CARTESIAN_POINT('Ctrl Pts',(77.0796598076102,442.539788989731,57.6990830704906));
#37311=CARTESIAN_POINT('Ctrl Pts',(79.0466176623673,442.677358353056,56.1485088279186));
#37312=CARTESIAN_POINT('Ctrl Pts',(80.0433712123539,442.814927716381,53.8507520860707));
#37313=CARTESIAN_POINT('Ctrl Pts',(79.8316514884425,442.952497079707,51.3550801439626));
#37314=CARTESIAN_POINT('Ctrl Pts',(78.4620690355979,443.090066443032,49.2580709429864));
#37315=CARTESIAN_POINT('Ctrl Pts',(76.2620157143041,443.227635806357,48.0610040828726));
#37316=CARTESIAN_POINT('Ctrl Pts',(73.7574033077667,443.365205169682,48.0500324313384));
#37317=CARTESIAN_POINT('Ctrl Pts',(71.5469469308476,443.502774533007,49.2277787070091));
#37318=CARTESIAN_POINT('Ctrl Pts',(70.3028860573773,443.626086331116,51.0966282777811));
#37319=CARTESIAN_POINT('Ctrl Pts',(70.0703410020562,443.703541674784,52.464881605413));
#37320=CARTESIAN_POINT('Ctrl Pts',(70.0698685442402,443.735140564009,53.0229212964126));
#37321=CARTESIAN_POINT('Origin',(74.9879498948689,433.764859435991,53.0228109606356));
#37322=CARTESIAN_POINT('',(70.0695156097612,439.889859435991,53.0227034971274));
#37323=CARTESIAN_POINT('',(70.069722329707,440.235140564009,53.0226894836296));
#37324=CARTESIAN_POINT('',(70.0696998948689,433.764859435991,53.0228109606359));
#37325=CARTESIAN_POINT('Ctrl Pts',(70.0695156097609,439.889859435991,53.0227034971274));
#37326=CARTESIAN_POINT('Ctrl Pts',(70.0701635410552,439.928219661898,53.7000091240524));
#37327=CARTESIAN_POINT('Ctrl Pts',(70.3799715464621,440.012436358161,55.1875519623061));
#37328=CARTESIAN_POINT('Ctrl Pts',(71.8322073992925,440.142509524781,57.0581624818043));
#37329=CARTESIAN_POINT('Ctrl Pts',(74.1225020644475,440.28007893585,58.0719467909454));
#37330=CARTESIAN_POINT('Ctrl Pts',(76.6196778606811,440.417648346919,57.8787595222969));
#37331=CARTESIAN_POINT('Ctrl Pts',(78.7267969530214,440.555217757988,56.5247811576843));
#37332=CARTESIAN_POINT('Ctrl Pts',(79.9401626795821,440.692787169057,54.3336736996951));
#37333=CARTESIAN_POINT('Ctrl Pts',(79.969725812863,440.830356580126,51.8292108229069));
#37334=CARTESIAN_POINT('Ctrl Pts',(78.8084194282583,440.967925991195,49.6100723052293));
#37335=CARTESIAN_POINT('Ctrl Pts',(76.7338482188175,441.105495402264,48.2067325114984));
#37336=CARTESIAN_POINT('Ctrl Pts',(74.2419284313758,441.243064813333,47.9546530544782));
#37337=CARTESIAN_POINT('Ctrl Pts',(71.928341478485,441.380634224401,48.9140923131546));
#37338=CARTESIAN_POINT('Ctrl Pts',(70.4071472833128,441.512899098621,50.7808344993748));
#37339=CARTESIAN_POINT('Ctrl Pts',(70.0699931805514,441.599307502484,52.3069372826869));
#37340=CARTESIAN_POINT('Ctrl Pts',(70.0694094802034,441.639859435991,53.0228960008483));
#37341=CARTESIAN_POINT('Ctrl Pts',(70.0697223297068,440.235140564009,53.0226894836296));
#37342=CARTESIAN_POINT('Ctrl Pts',(70.0703202469893,440.269653434849,53.6321383121744));
#37343=CARTESIAN_POINT('Ctrl Pts',(70.3348709418805,440.35002276013,55.051852454326));
#37344=CARTESIAN_POINT('Ctrl Pts',(71.6677368744888,440.476248539853,56.9239590872673));
#37345=CARTESIAN_POINT('Ctrl Pts',(73.9140643916323,440.613817903178,58.0317570703397));
#37346=CARTESIAN_POINT('Ctrl Pts',(76.4170988864601,440.751387266504,57.9421914464564));
#37347=CARTESIAN_POINT('Ctrl Pts',(78.5785024367767,440.888956629829,56.6766724315182));
#37348=CARTESIAN_POINT('Ctrl Pts',(79.8816022941954,441.026525993154,54.5377160398189));
#37349=CARTESIAN_POINT('Ctrl Pts',(80.014898931527,441.164095356479,52.0366291379667));
#37350=CARTESIAN_POINT('Ctrl Pts',(78.9465284517881,441.301664719805,49.7712840865122));
#37351=CARTESIAN_POINT('Ctrl Pts',(76.9318794943156,441.43923408313,48.2832003313887));
#37352=CARTESIAN_POINT('Ctrl Pts',(74.4525438530313,441.576803446455,47.9280968788807));
#37353=CARTESIAN_POINT('Ctrl Pts',(72.1011943580286,441.71437280978,48.7908594397661));
#37354=CARTESIAN_POINT('Ctrl Pts',(70.4575039816879,441.850485182298,50.6453973502539));
#37355=CARTESIAN_POINT('Ctrl Pts',(70.0695204468552,441.940741100375,52.239005209128));
#37356=CARTESIAN_POINT('Ctrl Pts',(70.0692875054392,441.985140564009,53.0228369856911));
#37357=CARTESIAN_POINT('Origin',(74.9879498948689,433.764859435991,53.0228109606356));
#37358=CARTESIAN_POINT('',(70.0701612938335,438.139859435991,53.0228096632581));
#37359=CARTESIAN_POINT('',(70.0700845742479,438.485140564009,53.0228422002615));
#37360=CARTESIAN_POINT('',(70.0696998948689,433.764859435991,53.0228109606359));
#37361=CARTESIAN_POINT('Ctrl Pts',(70.0701612938333,438.139859435991,53.0228096632581));
#37362=CARTESIAN_POINT('Ctrl Pts',(70.0702739414449,438.165418880599,53.4742429003227));
#37363=CARTESIAN_POINT('Ctrl Pts',(70.242451475972,438.236834795563,54.7357509431657));
#37364=CARTESIAN_POINT('Ctrl Pts',(71.3075510106673,438.354107180884,56.586112001967));
#37365=CARTESIAN_POINT('Ctrl Pts',(73.4367474201414,438.491676591953,57.9050989515375));
#37366=CARTESIAN_POINT('Ctrl Pts',(75.9367802424272,438.629246003022,58.0569396214243));
#37367=CARTESIAN_POINT('Ctrl Pts',(78.2099924611958,438.766815414091,57.0054284326608));
#37368=CARTESIAN_POINT('Ctrl Pts',(79.7129963873825,438.90438482516,55.0018790181383));
#37369=CARTESIAN_POINT('Ctrl Pts',(80.0864990188232,439.041954236229,52.5252494404828));
#37370=CARTESIAN_POINT('Ctrl Pts',(79.2412191183861,439.179523647298,50.1675568417403));
#37371=CARTESIAN_POINT('Ctrl Pts',(77.3792153333098,439.317093058367,48.492400302215));
#37372=CARTESIAN_POINT('Ctrl Pts',(74.9455912824701,439.454662469436,47.9002160217303));
#37373=CARTESIAN_POINT('Ctrl Pts',(72.5220927714855,439.592231880505,48.5325636389322));
#37374=CARTESIAN_POINT('Ctrl Pts',(70.6880455611049,439.729801291574,50.2382831133303));
#37375=CARTESIAN_POINT('Ctrl Pts',(70.1066659790318,439.829010476736,51.9483976678048));
#37376=CARTESIAN_POINT('Ctrl Pts',(70.0693889929006,439.882363191541,52.8903463895694));
#37377=CARTESIAN_POINT('Ctrl Pts',(70.0695156097609,439.889859435991,53.0227034971274));
#37378=CARTESIAN_POINT('Ctrl Pts',(70.0700845742477,438.485140564009,53.0228422002615));
#37379=CARTESIAN_POINT('Ctrl Pts',(70.0700285470462,438.50685286044,53.406329627451));
#37380=CARTESIAN_POINT('Ctrl Pts',(70.2079331020722,438.574421611312,54.5997090727309));
#37381=CARTESIAN_POINT('Ctrl Pts',(71.1630752524974,438.687846816626,56.4306054140694));
#37382=CARTESIAN_POINT('Ctrl Pts',(73.2358186748897,438.825416179951,57.836628058181));
#37383=CARTESIAN_POINT('Ctrl Pts',(75.7274140404831,438.962985543276,58.0919298326021));
#37384=CARTESIAN_POINT('Ctrl Pts',(78.0422377232922,439.100554906601,57.1354858952104));
#37385=CARTESIAN_POINT('Ctrl Pts',(79.6269519827668,439.238124269927,55.1959270225485));
#37386=CARTESIAN_POINT('Ctrl Pts',(80.1027345777162,439.375693633252,52.7368959420052));
#37387=CARTESIAN_POINT('Ctrl Pts',(79.3558539781017,439.513262996577,50.346211308417));
#37388=CARTESIAN_POINT('Ctrl Pts',(77.564847398211,439.650832359902,48.5953545532883));
#37389=CARTESIAN_POINT('Ctrl Pts',(75.1578464351838,439.788401723227,47.90285916436));
#37390=CARTESIAN_POINT('Ctrl Pts',(72.7102324938985,439.925971086553,48.4342627525347));
#37391=CARTESIAN_POINT('Ctrl Pts',(70.8070955727843,440.063540449878,50.0625359188796));
#37392=CARTESIAN_POINT('Ctrl Pts',(70.1300939560672,440.166596942364,51.8124234577472));
#37393=CARTESIAN_POINT('Ctrl Pts',(70.0695258081044,440.223796980407,52.8223777283444));
#37394=CARTESIAN_POINT('Ctrl Pts',(70.0697223297068,440.235140564009,53.0226894836296));
#37395=CARTESIAN_POINT('Origin',(74.9879498948689,423.667006141107,53.0228109606356));
#37396=CARTESIAN_POINT('',(80.6362536929626,17.6670061411077,53.0272245279143));
#37397=CARTESIAN_POINT('',(80.6384886732644,16.3329938588948,53.0278707901325));
#37398=CARTESIAN_POINT('',(80.6314498948689,423.667006141107,53.0228109606222));
#37399=CARTESIAN_POINT('',(72.1688064861925,15.,48.133892604668));
#37400=CARTESIAN_POINT('Ctrl Pts',(80.6362536929627,17.6670061411077,53.0272245279143));
#37401=CARTESIAN_POINT('Ctrl Pts',(80.6388674031541,17.6350087809895,53.3099173664622));
#37402=CARTESIAN_POINT('Ctrl Pts',(80.4919324779875,17.3908554113189,55.464601173614));
#37403=CARTESIAN_POINT('Ctrl Pts',(77.7100437690878,16.9345460320961,59.1173659193523));
#37404=CARTESIAN_POINT('Ctrl Pts',(71.3329561213306,16.2980780034392,58.6109033270751));
#37405=CARTESIAN_POINT('Ctrl Pts',(68.3132228555609,15.6616099747823,52.9593291895844));
#37406=CARTESIAN_POINT('Ctrl Pts',(70.4291852017175,15.2289173069691,49.1745538303573));
#37407=CARTESIAN_POINT('Ctrl Pts',(72.1003657071,15.0083806487084,48.1647847936954));
#37408=CARTESIAN_POINT('Ctrl Pts',(72.1646654645455,15.,48.1277497923176));
#37409=CARTESIAN_POINT('',(72.1688064861966,15.,57.9117293166054));
#37410=CARTESIAN_POINT('Origin',(74.9879498948689,15.,53.0228109606356));
#37411=CARTESIAN_POINT('Ctrl Pts',(80.6384886732644,16.3329938588948,53.0278707901325));
#37412=CARTESIAN_POINT('Ctrl Pts',(80.6396925569063,16.3129745917012,53.2045791057297));
#37413=CARTESIAN_POINT('Ctrl Pts',(80.5523891734711,16.0807993149553,55.252320400191));
#37414=CARTESIAN_POINT('Ctrl Pts',(78.6506201566575,15.7425460334332,58.0582788876747));
#37415=CARTESIAN_POINT('Ctrl Pts',(74.8443820757933,15.3182340143285,58.8942202496515));
#37416=CARTESIAN_POINT('Ctrl Pts',(72.983431993014,15.1060780047762,58.3814745569358));
#37417=CARTESIAN_POINT('Ctrl Pts',(72.1688064861966,15.,57.9117293166054));
#37418=CARTESIAN_POINT('Origin',(74.9879498948689,423.667006141107,53.0228109606356));
#37419=CARTESIAN_POINT('',(80.631428174539,21.6670061411077,53.0228143106163));
#37420=CARTESIAN_POINT('',(80.6243731925048,20.3329938588948,53.0275588194414));
#37421=CARTESIAN_POINT('',(80.6314498948689,423.667006141107,53.0228109606222));
#37422=CARTESIAN_POINT('Ctrl Pts',(80.6226532189624,21.6670061411077,53.0241676993539));
#37423=CARTESIAN_POINT('Ctrl Pts',(80.6252968410462,21.57461150497,53.8467888709005));
#37424=CARTESIAN_POINT('Ctrl Pts',(80.071690884932,21.2700608592801,56.5552810828106));
#37425=CARTESIAN_POINT('Ctrl Pts',(75.890175270785,20.7533542040378,59.633916297922));
#37426=CARTESIAN_POINT('Ctrl Pts',(69.9117395951546,20.1168861753808,57.3605004391449));
#37427=CARTESIAN_POINT('Ctrl Pts',(68.5965174256227,19.4804181467239,51.0887193976995));
#37428=CARTESIAN_POINT('Ctrl Pts',(72.3977774992468,18.9500281228431,47.3601749200438));
#37429=CARTESIAN_POINT('Ctrl Pts',(76.2793092635613,18.5257161037384,47.3001117920513));
#37430=CARTESIAN_POINT('Ctrl Pts',(79.4966060481514,18.1334014447521,48.8909550864173));
#37431=CARTESIAN_POINT('Ctrl Pts',(80.6215374008575,17.8471647905418,51.4355444702682));
#37432=CARTESIAN_POINT('Ctrl Pts',(80.6362536929627,17.6670061411077,53.0272245279143));
#37433=CARTESIAN_POINT('Ctrl Pts',(80.6243731925048,20.3329938588948,53.0275588194413));
#37434=CARTESIAN_POINT('Ctrl Pts',(80.6283935590626,20.2525773156817,53.7428893577669));
#37435=CARTESIAN_POINT('Ctrl Pts',(80.1698683025709,19.9600047629164,56.3396104649291));
#37436=CARTESIAN_POINT('Ctrl Pts',(77.0829706090005,19.5613542053749,58.8867113839554));
#37437=CARTESIAN_POINT('Ctrl Pts',(73.2105872069091,19.1370421862702,58.6136853706606));
#37438=CARTESIAN_POINT('Ctrl Pts',(69.8912577533702,18.7127301671655,56.6010225426405));
#37439=CARTESIAN_POINT('Ctrl Pts',(68.4956769583314,18.1823401432847,51.4606824589819));
#37440=CARTESIAN_POINT('Ctrl Pts',(72.7985336869453,17.5458721146278,46.717269598202));
#37441=CARTESIAN_POINT('Ctrl Pts',(78.9102182501813,16.9294233531645,47.7356724886824));
#37442=CARTESIAN_POINT('Ctrl Pts',(80.6269342902349,16.5251306012535,51.331896617944));
#37443=CARTESIAN_POINT('Ctrl Pts',(80.6384886732644,16.3329938588948,53.0278707901325));
#37444=CARTESIAN_POINT('Origin',(74.9879498948689,423.667006141107,53.0228109606356));
#37445=CARTESIAN_POINT('',(80.6314498948689,25.6670061411076,53.0228109606223));
#37446=CARTESIAN_POINT('',(80.6253679025463,24.3329938588948,53.0178459337856));
#37447=CARTESIAN_POINT('',(80.6314498948689,423.667006141107,53.0228109606222));
#37448=CARTESIAN_POINT('Ctrl Pts',(80.6314498948689,25.6670061411076,53.0228109606223));
#37449=CARTESIAN_POINT('Ctrl Pts',(80.6314498948729,25.4742213185053,54.7318077489414));
#37450=CARTESIAN_POINT('Ctrl Pts',(79.8060659192715,25.2814364959029,56.4221521097231));
#37451=CARTESIAN_POINT('Ctrl Pts',(78.4584055093469,25.0886516733005,57.473095229976));
#37452=CARTESIAN_POINT('Ctrl Pts',(77.1107450994222,24.8958668506981,58.5240383502288));
#37453=CARTESIAN_POINT('Ctrl Pts',(75.2702256751666,24.7030820280957,58.9126397065621));
#37454=CARTESIAN_POINT('Ctrl Pts',(73.6127451627081,24.5102972054933,58.4961923829962));
#37455=CARTESIAN_POINT('Ctrl Pts',(71.9552646502496,24.3175123828909,58.0797450594303));
#37456=CARTESIAN_POINT('Ctrl Pts',(70.5170033810758,24.1247275602885,56.8673394809208));
#37457=CARTESIAN_POINT('Ctrl Pts',(69.826137149614,23.9319427376861,55.3042099684649));
#37458=CARTESIAN_POINT('Ctrl Pts',(69.1352709181523,23.7391579150837,53.7410804560089));
#37459=CARTESIAN_POINT('Ctrl Pts',(69.2068803054892,23.5463730924813,51.8613477992592));
#37460=CARTESIAN_POINT('Ctrl Pts',(70.0146680415421,23.3535882698789,50.355310284465));
#37461=CARTESIAN_POINT('Ctrl Pts',(70.822455777595,23.1608034472765,48.8492727696708));
#37462=CARTESIAN_POINT('Ctrl Pts',(72.3487890589358,22.9680186246741,47.7498049531896));
#37463=CARTESIAN_POINT('Ctrl Pts',(74.0331492157569,22.7752338020717,47.4606667775738));
#37464=CARTESIAN_POINT('Ctrl Pts',(75.7175093725781,22.5824489794693,47.1715286019581));
#37465=CARTESIAN_POINT('Ctrl Pts',(77.5231293307811,22.389664156867,47.6990315230355));
#37466=CARTESIAN_POINT('Ctrl Pts',(78.7869273705855,22.1968793342646,48.8494595029941));
#37467=CARTESIAN_POINT('Ctrl Pts',(79.9447859852089,22.0202549365456,49.9034514424855));
#37468=CARTESIAN_POINT('Ctrl Pts',(80.6314498948652,21.8436305388266,51.4570729301807));
#37469=CARTESIAN_POINT('Ctrl Pts',(80.6314498948689,21.6670061411077,53.0228109606222));
#37470=CARTESIAN_POINT('Ctrl Pts',(80.6253679025463,24.3329938588948,53.0178459337856));
#37471=CARTESIAN_POINT('Ctrl Pts',(80.6151298375501,24.1921800396623,54.2675854419267));
#37472=CARTESIAN_POINT('Ctrl Pts',(79.8930755009726,23.9452882156536,56.4684188056548));
#37473=CARTESIAN_POINT('Ctrl Pts',(77.3122715737554,23.5923183868688,58.4096717625035));
#37474=CARTESIAN_POINT('Ctrl Pts',(73.4859668057208,23.1680063677642,59.0656658471794));
#37475=CARTESIAN_POINT('Ctrl Pts',(69.0626632683662,22.6376163438834,56.1021187103944));
#37476=CARTESIAN_POINT('Ctrl Pts',(69.1990635927837,22.0011483152264,49.695206442741));
#37477=CARTESIAN_POINT('Ctrl Pts',(74.6559956914946,21.3646802865695,46.3586883014623));
#37478=CARTESIAN_POINT('Ctrl Pts',(79.6894979343186,20.8086288011256,48.7854595298665));
#37479=CARTESIAN_POINT('Ctrl Pts',(80.6177869737537,20.464733325234,51.8556946779366));
#37480=CARTESIAN_POINT('Ctrl Pts',(80.6243731925048,20.3329938588948,53.0275588194413));
#37481=CARTESIAN_POINT('Origin',(74.9879498948689,423.667006141107,53.0228109606356));
#37482=CARTESIAN_POINT('',(80.6400146763751,29.6670061411077,53.0229792748411));
#37483=CARTESIAN_POINT('',(80.6386417035632,28.3329938588948,53.0220653173588));
#37484=CARTESIAN_POINT('',(80.6314498948689,423.667006141107,53.0228109606222));
#37485=CARTESIAN_POINT('Ctrl Pts',(80.6400146763751,29.6670061411077,53.0229792748411));
#37486=CARTESIAN_POINT('Ctrl Pts',(80.6400186296118,29.6659729624834,53.0320960062332));
#37487=CARTESIAN_POINT('Ctrl Pts',(80.6399984395038,29.6649397838592,53.041212719425));
#37488=CARTESIAN_POINT('Ctrl Pts',(80.6399540528249,29.663906605235,53.0503293148091));
#37489=CARTESIAN_POINT('Ctrl Pts',(80.6308395585354,29.4517505956827,54.9223584606314));
#37490=CARTESIAN_POINT('Ctrl Pts',(79.6014584560108,29.2395945861304,56.789420153395));
#37491=CARTESIAN_POINT('Ctrl Pts',(78.0210409074678,29.0274385765781,57.793596730602));
#37492=CARTESIAN_POINT('Ctrl Pts',(76.4406233589247,28.8152825670258,58.7977733078089));
#37493=CARTESIAN_POINT('Ctrl Pts',(74.3091693643633,28.6031265574734,58.939064769459));
#37494=CARTESIAN_POINT('Ctrl Pts',(72.6116221830727,28.3909705479211,58.152546524122));
#37495=CARTESIAN_POINT('Ctrl Pts',(70.9140750017821,28.1788145383688,57.3660282787849));
#37496=CARTESIAN_POINT('Ctrl Pts',(69.6504346337626,27.9666585288166,55.6517003264607));
#37497=CARTESIAN_POINT('Ctrl Pts',(69.3904097747983,27.7545025192642,53.7962936842702));
#37498=CARTESIAN_POINT('Ctrl Pts',(69.2603973453161,27.6484245144881,52.8685903631747));
#37499=CARTESIAN_POINT('Ctrl Pts',(69.381288793098,27.5423465097118,51.9056173696121));
#37500=CARTESIAN_POINT('Ctrl Pts',(69.7157350999898,27.4362685049356,51.0236229168265));
#37501=CARTESIAN_POINT('Ctrl Pts',(70.0501814068814,27.3301905001595,50.1416284640413));
#37502=CARTESIAN_POINT('Ctrl Pts',(70.5981825728826,27.2241124953834,49.3406125520325));
#37503=CARTESIAN_POINT('Ctrl Pts',(71.3106189980845,27.1180344906072,48.7323601111073));
#37504=CARTESIAN_POINT('Ctrl Pts',(72.7354918484887,26.9058784810549,47.5158552292564));
#37505=CARTESIAN_POINT('Ctrl Pts',(74.8181057356958,26.6937224715026,47.0704042317404));
#37506=CARTESIAN_POINT('Ctrl Pts',(76.6103494066449,26.4815664619503,47.6071909688715));
#37507=CARTESIAN_POINT('Ctrl Pts',(78.4025930775939,26.2694104523979,48.1439777060026));
#37508=CARTESIAN_POINT('Ctrl Pts',(79.9044665322848,26.0572544428457,49.6630021777805));
#37509=CARTESIAN_POINT('Ctrl Pts',(80.4217124325031,25.8450984332934,51.4625985221484));
#37510=CARTESIAN_POINT('Ctrl Pts',(80.5664447738713,25.7857343358981,51.9661497196119));
#37511=CARTESIAN_POINT('Ctrl Pts',(80.6340851624506,25.7263702385029,52.4916684452613));
#37512=CARTESIAN_POINT('Ctrl Pts',(80.6294005094961,25.6670061411077,53.0182687964583));
#37513=CARTESIAN_POINT('Ctrl Pts',(80.6386417035632,28.3329938588948,53.0220653173588));
#37514=CARTESIAN_POINT('Ctrl Pts',(80.637090133247,28.237860768419,53.8624301588762));
#37515=CARTESIAN_POINT('Ctrl Pts',(80.2117010840973,28.036649673167,55.6432505569544));
#37516=CARTESIAN_POINT('Ctrl Pts',(77.8164221205999,27.6232825683628,58.5700374594237));
#37517=CARTESIAN_POINT('Ctrl Pts',(72.5335666026989,27.092892544482,59.2330665250225));
#37518=CARTESIAN_POINT('Ctrl Pts',(68.4353446939828,26.4564245158251,54.3063931884985));
#37519=CARTESIAN_POINT('Ctrl Pts',(70.3674902113553,25.8199564871681,48.2091214630561));
#37520=CARTESIAN_POINT('Ctrl Pts',(76.5387626327649,25.1834884585111,46.5282601413106));
#37521=CARTESIAN_POINT('Ctrl Pts',(80.2415468362615,24.6878342490867,49.8742024937387));
#37522=CARTESIAN_POINT('Ctrl Pts',(80.6305549359316,24.4043360492146,52.3846754514713));
#37523=CARTESIAN_POINT('Ctrl Pts',(80.6253679025463,24.3329938588948,53.0178459337856));
#37524=CARTESIAN_POINT('Origin',(74.9879498948689,423.667006141107,53.0228109606356));
#37525=CARTESIAN_POINT('',(80.6314498948689,33.6670061411076,53.0228109606225));
#37526=CARTESIAN_POINT('',(80.6329429902157,32.3329938588949,53.0264768953321));
#37527=CARTESIAN_POINT('',(80.6314498948689,423.667006141107,53.0228109606222));
#37528=CARTESIAN_POINT('Ctrl Pts',(80.6288724674716,33.6670061411077,53.0272877637515));
#37529=CARTESIAN_POINT('Ctrl Pts',(80.633617327969,33.605575686464,53.5723418811337));
#37530=CARTESIAN_POINT('Ctrl Pts',(80.561099549628,33.5441452318203,54.1162638727118));
#37531=CARTESIAN_POINT('Ctrl Pts',(80.4062625201533,33.4827147771767,54.6358597062275));
#37532=CARTESIAN_POINT('Ctrl Pts',(79.8715178809539,33.2705587676244,56.4303341124181));
#37533=CARTESIAN_POINT('Ctrl Pts',(78.3549244089112,33.058402758072,57.9346624158183));
#37534=CARTESIAN_POINT('Ctrl Pts',(76.5575388418803,32.8462467485197,58.4539720580937));
#37535=CARTESIAN_POINT('Ctrl Pts',(74.7601532748492,32.6340907389674,58.9732817003692));
#37536=CARTESIAN_POINT('Ctrl Pts',(72.6819756128296,32.4219347294151,58.5075726815198));
#37537=CARTESIAN_POINT('Ctrl Pts',(71.2690158181734,32.2097787198628,57.2772510246664));
#37538=CARTESIAN_POINT('Ctrl Pts',(70.5625359208453,32.1037007150866,56.6620901962398));
#37539=CARTESIAN_POINT('Ctrl Pts',(70.022360490358,31.9976227103104,55.8557762083121));
#37540=CARTESIAN_POINT('Ctrl Pts',(69.6965183067651,31.8915447055342,54.9705669609224));
#37541=CARTESIAN_POINT('Ctrl Pts',(69.3706761231721,31.7854667007581,54.0853577135324));
#37542=CARTESIAN_POINT('Ctrl Pts',(69.2591671864736,31.679388695982,53.1212532066807));
#37543=CARTESIAN_POINT('Ctrl Pts',(69.3982068004462,31.5733106912058,52.1948598366998));
#37544=CARTESIAN_POINT('Ctrl Pts',(69.6762860283913,31.3611546816536,50.3420730967384));
#37545=CARTESIAN_POINT('Ctrl Pts',(70.9565594590206,31.1489986721012,48.6401309042619));
#37546=CARTESIAN_POINT('Ctrl Pts',(72.6616847459306,30.9368426625489,47.8701795179302));
#37547=CARTESIAN_POINT('Ctrl Pts',(74.3668100328406,30.7246866529966,47.1002281315985));
#37548=CARTESIAN_POINT('Ctrl Pts',(76.4967871760314,30.5125306434443,47.2622675514116));
#37549=CARTESIAN_POINT('Ctrl Pts',(78.0673518045997,30.300374633892,48.2817855607585));
#37550=CARTESIAN_POINT('Ctrl Pts',(79.6302679399409,30.0892518029639,49.2963386189995));
#37551=CARTESIAN_POINT('Ctrl Pts',(80.6392068600684,29.8781289720358,51.1600389321174));
#37552=CARTESIAN_POINT('Ctrl Pts',(80.6400146763751,29.6670061411077,53.0229792748411));
#37553=CARTESIAN_POINT('Ctrl Pts',(80.6329429902157,32.3329938588949,53.0264768953321));
#37554=CARTESIAN_POINT('Ctrl Pts',(80.635781829672,32.2835414971757,53.464786485973));
#37555=CARTESIAN_POINT('Ctrl Pts',(80.587714509014,32.2340891354566,53.9023462171139));
#37556=CARTESIAN_POINT('Ctrl Pts',(80.4860984518382,32.1846367737375,54.3270706628304));
#37557=CARTESIAN_POINT('Ctrl Pts',(80.0501545161511,31.9724807641851,56.1491847223035));
#37558=CARTESIAN_POINT('Ctrl Pts',(78.628644314649,31.7603247546329,57.7350649292334));
#37559=CARTESIAN_POINT('Ctrl Pts',(76.863771950532,31.5481687450806,58.3559537435553));
#37560=CARTESIAN_POINT('Ctrl Pts',(75.0988995864149,31.3360127355283,58.9768425578771));
#37561=CARTESIAN_POINT('Ctrl Pts',(72.990665059683,31.123856725976,58.6327399795908));
#37562=CARTESIAN_POINT('Ctrl Pts',(71.5133168751436,30.9117007164237,57.4822911256512));
#37563=CARTESIAN_POINT('Ctrl Pts',(70.035968690604,30.6995447068713,56.3318422717114));
#37564=CARTESIAN_POINT('Ctrl Pts',(69.1895068482571,30.487388697319,54.3750471421177));
#37565=CARTESIAN_POINT('Ctrl Pts',(69.3591270580384,30.2752326877666,52.5106959999642));
#37566=CARTESIAN_POINT('Ctrl Pts',(69.5287472678197,30.0630766782143,50.6463448578111));
#37567=CARTESIAN_POINT('Ctrl Pts',(70.7144495297283,29.8509206686621,48.874437703098));
#37568=CARTESIAN_POINT('Ctrl Pts',(72.3751599774456,29.6387646591098,48.0094920199503));
#37569=CARTESIAN_POINT('Ctrl Pts',(74.0358704251634,29.4266086495574,47.1445463368025));
#37570=CARTESIAN_POINT('Ctrl Pts',(76.1715890586898,29.2144526400051,47.1865621252207));
#37571=CARTESIAN_POINT('Ctrl Pts',(77.7954333266113,29.0022966304528,48.1157591853188));
#37572=CARTESIAN_POINT('Ctrl Pts',(79.4192775945326,28.7901406209005,49.0449562454168));
#37573=CARTESIAN_POINT('Ctrl Pts',(80.5312474968489,28.5779846113481,50.8613345771943));
#37574=CARTESIAN_POINT('Ctrl Pts',(80.631200650374,28.3658286017958,52.7322049902012));
#37575=CARTESIAN_POINT('Ctrl Pts',(80.636357132633,28.3548836874955,52.828721305627));
#37576=CARTESIAN_POINT('Ctrl Pts',(80.6388202093182,28.3439387731951,52.9253826475808));
#37577=CARTESIAN_POINT('Ctrl Pts',(80.6386417035632,28.3329938588948,53.0220653173588));
#37578=CARTESIAN_POINT('Origin',(74.9879498948689,423.667006141107,53.0228109606356));
#37579=CARTESIAN_POINT('',(80.6314498948689,37.6670061411077,53.0228109606227));
#37580=CARTESIAN_POINT('',(80.6202517864306,36.3329938588948,53.0234467810542));
#37581=CARTESIAN_POINT('',(80.6314498948689,423.667006141107,53.0228109606222));
#37582=CARTESIAN_POINT('Ctrl Pts',(80.6314498948689,37.6670061411077,53.022810960622));
#37583=CARTESIAN_POINT('Ctrl Pts',(80.631449894873,37.4742213185054,54.7318077489411));
#37584=CARTESIAN_POINT('Ctrl Pts',(79.8060659192717,37.2814364959029,56.4221521097229));
#37585=CARTESIAN_POINT('Ctrl Pts',(78.4584055093471,37.0886516733005,57.4730952299758));
#37586=CARTESIAN_POINT('Ctrl Pts',(77.1107450994225,36.8958668506981,58.5240383502287));
#37587=CARTESIAN_POINT('Ctrl Pts',(75.2702256751669,36.7030820280957,58.9126397065621));
#37588=CARTESIAN_POINT('Ctrl Pts',(73.6127451627084,36.5102972054933,58.4961923829963));
#37589=CARTESIAN_POINT('Ctrl Pts',(71.9552646502498,36.3175123828909,58.0797450594305));
#37590=CARTESIAN_POINT('Ctrl Pts',(70.517003381076,36.1247275602886,56.867339480921));
#37591=CARTESIAN_POINT('Ctrl Pts',(69.8261371496142,35.9319427376862,55.3042099684651));
#37592=CARTESIAN_POINT('Ctrl Pts',(69.1352709181523,35.7391579150838,53.7410804560092));
#37593=CARTESIAN_POINT('Ctrl Pts',(69.2068803054892,35.5463730924814,51.8613477992594));
#37594=CARTESIAN_POINT('Ctrl Pts',(70.014668041542,35.353588269879,50.3553102844652));
#37595=CARTESIAN_POINT('Ctrl Pts',(70.8224557775948,35.1608034472766,48.849272769671));
#37596=CARTESIAN_POINT('Ctrl Pts',(72.3487890589355,34.9680186246741,47.7498049531897));
#37597=CARTESIAN_POINT('Ctrl Pts',(74.0331492157566,34.7752338020717,47.4606667775739));
#37598=CARTESIAN_POINT('Ctrl Pts',(75.7175093725778,34.5824489794693,47.1715286019581));
#37599=CARTESIAN_POINT('Ctrl Pts',(77.5231293307808,34.389664156867,47.6990315230354));
#37600=CARTESIAN_POINT('Ctrl Pts',(78.7869273705853,34.1968793342646,48.8494595029939));
#37601=CARTESIAN_POINT('Ctrl Pts',(79.9447859852089,34.0202549365456,49.9034514424854));
#37602=CARTESIAN_POINT('Ctrl Pts',(80.6314498948653,33.8436305388266,51.4570729301809));
#37603=CARTESIAN_POINT('Ctrl Pts',(80.6314498948689,33.6670061411076,53.0228109606225));
#37604=CARTESIAN_POINT('Ctrl Pts',(80.620244429633,36.3329938588948,53.0234471987678));
#37605=CARTESIAN_POINT('Ctrl Pts',(80.6203792639667,36.2231442211563,54.0004693354651));
#37606=CARTESIAN_POINT('Ctrl Pts',(80.3804009483158,36.1132945834177,54.9773613084557));
#37607=CARTESIAN_POINT('Ctrl Pts',(79.9012805970799,36.0034449456792,55.81929120189));
#37608=CARTESIAN_POINT('Ctrl Pts',(78.9759406150268,35.7912889361269,57.4453364960856));
#37609=CARTESIAN_POINT('Ctrl Pts',(77.1585914201757,35.5791329265746,58.5679679172326));
#37610=CARTESIAN_POINT('Ctrl Pts',(75.2888161061955,35.3669769170222,58.6681202952851));
#37611=CARTESIAN_POINT('Ctrl Pts',(73.4190407922153,35.1548209074699,58.7682726733377));
#37612=CARTESIAN_POINT('Ctrl Pts',(71.4968393591057,34.9426648979176,57.8459460082958));
#37613=CARTESIAN_POINT('Ctrl Pts',(70.4023953172393,34.7305088883653,56.3271410709748));
#37614=CARTESIAN_POINT('Ctrl Pts',(69.3079512753728,34.518352878813,54.8083361336536));
#37615=CARTESIAN_POINT('Ctrl Pts',(69.0412646247494,34.3061968692607,52.6930529240536));
#37616=CARTESIAN_POINT('Ctrl Pts',(69.7279277601338,34.0940408597084,50.9510471944045));
#37617=CARTESIAN_POINT('Ctrl Pts',(70.4145908955182,33.8818848501561,49.2090414647555));
#37618=CARTESIAN_POINT('Ctrl Pts',(72.0546038169107,33.6697288406038,47.8403132150578));
#37619=CARTESIAN_POINT('Ctrl Pts',(73.8899023408418,33.4575728310515,47.4770547544705));
#37620=CARTESIAN_POINT('Ctrl Pts',(75.7252008647727,33.2454168214991,47.1137962938832));
#37621=CARTESIAN_POINT('Ctrl Pts',(77.7557849912424,33.0332608119468,47.756007622406));
#37622=CARTESIAN_POINT('Ctrl Pts',(79.0580310893936,32.8211048023945,49.1029678521407));
#37623=CARTESIAN_POINT('Ctrl Pts',(79.7091541384693,32.7150267976184,49.7764479670082));
#37624=CARTESIAN_POINT('Ctrl Pts',(80.1781926804654,32.6089487928422,50.6261153071788));
#37625=CARTESIAN_POINT('Ctrl Pts',(80.4269217507685,32.502870788066,51.5360067237003));
#37626=CARTESIAN_POINT('Ctrl Pts',(80.5596961518577,32.446245145009,52.021717090155));
#37627=CARTESIAN_POINT('Ctrl Pts',(80.6296923646812,32.3896195019519,52.5245885817045));
#37628=CARTESIAN_POINT('Ctrl Pts',(80.6329429902157,32.3329938588949,53.0264768953321));
#37629=CARTESIAN_POINT('Origin',(74.9879498948689,423.667006141107,53.0228109606356));
#37630=CARTESIAN_POINT('',(80.6368917650185,41.6670061411077,53.0191116230352));
#37631=CARTESIAN_POINT('',(80.633865742348,40.3329938588947,53.0161690164858));
#37632=CARTESIAN_POINT('',(80.6314498948689,423.667006141107,53.0228109606222));
#37633=CARTESIAN_POINT('Ctrl Pts',(80.6368917650185,41.6670061411077,53.0191116230352));
#37634=CARTESIAN_POINT('Ctrl Pts',(80.6224390043439,41.4847811344251,54.6286369705124));
#37635=CARTESIAN_POINT('Ctrl Pts',(79.473040189755,41.1964781229664,57.189451688561));
#37636=CARTESIAN_POINT('Ctrl Pts',(76.2235906019975,40.8020971067315,58.7581360420116));
#37637=CARTESIAN_POINT('Ctrl Pts',(72.3427116734402,40.3777850876269,58.6597153718375));
#37638=CARTESIAN_POINT('Ctrl Pts',(68.5780159994796,39.8473950637461,54.8947137762651));
#37639=CARTESIAN_POINT('Ctrl Pts',(69.9542034117819,39.2109270350892,48.6358286646777));
#37640=CARTESIAN_POINT('Ctrl Pts',(75.9545145524023,38.5744590064322,46.4208411581293));
#37641=CARTESIAN_POINT('Ctrl Pts',(80.0892431940405,38.0598187084384,49.5275271159818));
#37642=CARTESIAN_POINT('Ctrl Pts',(80.62580916943,37.7573344199969,52.2169736538586));
#37643=CARTESIAN_POINT('Ctrl Pts',(80.622857141901,37.6670061411077,53.0211285676652));
#37644=CARTESIAN_POINT('Ctrl Pts',(80.633865742348,40.3329938588947,53.0161690164858));
#37645=CARTESIAN_POINT('Ctrl Pts',(80.6198868644127,40.1627469451367,54.523658763612));
#37646=CARTESIAN_POINT('Ctrl Pts',(79.2207882231253,39.7803440218265,57.9367393444107));
#37647=CARTESIAN_POINT('Ctrl Pts',(73.4587819402533,39.185785088964,59.5175702230695));
#37648=CARTESIAN_POINT('Ctrl Pts',(68.6935887976469,38.5493170603069,55.2510918448196));
#37649=CARTESIAN_POINT('Ctrl Pts',(69.715665777593,37.91284903165,48.9247269106014));
#37650=CARTESIAN_POINT('Ctrl Pts',(74.601169621109,37.3824590077692,46.808120492965));
#37651=CARTESIAN_POINT('Ctrl Pts',(78.2462630815789,36.9581469886647,48.1438605690558));
#37652=CARTESIAN_POINT('Ctrl Pts',(80.1956475812481,36.6436846072985,50.2598786826923));
#37653=CARTESIAN_POINT('Ctrl Pts',(80.6201188542396,36.4353002307085,52.1135162054112));
#37654=CARTESIAN_POINT('Ctrl Pts',(80.620244429633,36.3329938588948,53.0234471987678));
#37655=CARTESIAN_POINT('Origin',(74.9879498948689,423.667006141107,53.0228109606356));
#37656=CARTESIAN_POINT('',(80.633385624059,45.6670061411077,53.0268327355589));
#37657=CARTESIAN_POINT('',(80.6393222206687,44.3329938588947,53.0263391207439));
#37658=CARTESIAN_POINT('',(80.6314498948689,423.667006141107,53.0228109606222));
#37659=CARTESIAN_POINT('Ctrl Pts',(80.6333856240591,45.6670061411077,53.0268327355589));
#37660=CARTESIAN_POINT('Ctrl Pts',(80.6357785977206,45.636539867958,53.2963621215798));
#37661=CARTESIAN_POINT('Ctrl Pts',(80.558137143727,45.4999955900322,54.5032763848713));
#37662=CARTESIAN_POINT('Ctrl Pts',(79.6816674585669,45.2573733073301,56.5427224905476));
#37663=CARTESIAN_POINT('Ctrl Pts',(76.6870768176045,44.8330612882254,59.0132153117264));
#37664=CARTESIAN_POINT('Ctrl Pts',(71.3759252168139,44.3026712643447,58.6392645053152));
#37665=CARTESIAN_POINT('Ctrl Pts',(68.3108182107715,43.6662032356877,53.011418232064));
#37666=CARTESIAN_POINT('Ctrl Pts',(71.38860861019,43.0297352070309,47.4045376647909));
#37667=CARTESIAN_POINT('Ctrl Pts',(77.7686820139573,42.3932671783739,46.9522470491929));
#37668=CARTESIAN_POINT('Ctrl Pts',(80.5030918708071,41.9390241563995,50.6184562946624));
#37669=CARTESIAN_POINT('Ctrl Pts',(80.6392656742262,41.6969371439774,52.7547422663191));
#37670=CARTESIAN_POINT('Ctrl Pts',(80.6368917650185,41.6670061411077,53.0191116230352));
#37671=CARTESIAN_POINT('Ctrl Pts',(80.6393222206687,44.3329938588947,53.0263391207439));
#37672=CARTESIAN_POINT('Ctrl Pts',(80.6403712518679,44.3145056786696,53.1896840219556));
#37673=CARTESIAN_POINT('Ctrl Pts',(80.5601215752485,44.0838614888923,55.226263817248));
#37674=CARTESIAN_POINT('Ctrl Pts',(78.0922262264452,43.6410612895625,58.9290551959863));
#37675=CARTESIAN_POINT('Ctrl Pts',(71.6968693820735,43.0045932609057,58.8325447221204));
#37676=CARTESIAN_POINT('Ctrl Pts',(68.3201615278016,42.3681252322486,53.3859514106338));
#37677=CARTESIAN_POINT('Ctrl Pts',(70.6207865388037,41.8377352083679,48.584358436323));
#37678=CARTESIAN_POINT('Ctrl Pts',(74.2487044880827,41.4134231892631,47.2026496248374));
#37679=CARTESIAN_POINT('Ctrl Pts',(78.1068463906541,40.9891111701586,47.6335196122566));
#37680=CARTESIAN_POINT('Ctrl Pts',(80.4344795314526,40.6289680600358,50.3998157139843));
#37681=CARTESIAN_POINT('Ctrl Pts',(80.637306874534,40.374902954689,52.6450754628535));
#37682=CARTESIAN_POINT('Ctrl Pts',(80.633865742348,40.3329938588947,53.0161690164858));
#37683=CARTESIAN_POINT('Origin',(74.9879498948689,423.667006141107,53.0228109606356));
#37684=CARTESIAN_POINT('',(80.6270010590704,49.6670061411077,53.0243752810309));
#37685=CARTESIAN_POINT('',(80.6244305214574,48.3329938588947,53.0264095113666));
#37686=CARTESIAN_POINT('',(80.6314498948689,423.667006141107,53.0228109606222));
#37687=CARTESIAN_POINT('Ctrl Pts',(80.6270010590704,49.6670061411077,53.0243752810309));
#37688=CARTESIAN_POINT('Ctrl Pts',(80.6288632137675,49.5761425919386,53.8321526964587));
#37689=CARTESIAN_POINT('Ctrl Pts',(80.4633217000993,49.4852790427694,54.6390877344253));
#37690=CARTESIAN_POINT('Ctrl Pts',(80.1288323138219,49.3944154936003,55.3684577541329));
#37691=CARTESIAN_POINT('Ctrl Pts',(79.3478377997498,49.1822594840479,57.0714534469405));
#37692=CARTESIAN_POINT('Ctrl Pts',(77.645791580905,48.9701034744957,58.3515885781149));
#37693=CARTESIAN_POINT('Ctrl Pts',(75.7940213035194,48.7579474649433,58.618467241464));
#37694=CARTESIAN_POINT('Ctrl Pts',(73.9422510261341,48.5457914553911,58.8853459048131));
#37695=CARTESIAN_POINT('Ctrl Pts',(71.9407566902084,48.3336354458388,58.138968100337));
#37696=CARTESIAN_POINT('Ctrl Pts',(70.7145322410308,48.1214794362864,56.7238837128038));
#37697=CARTESIAN_POINT('Ctrl Pts',(69.4883077918529,47.9093234267341,55.3087993252702));
#37698=CARTESIAN_POINT('Ctrl Pts',(69.0373532294238,47.6971674171817,53.2250083546785));
#37699=CARTESIAN_POINT('Ctrl Pts',(69.565269157885,47.4850114076293,51.4289345892408));
#37700=CARTESIAN_POINT('Ctrl Pts',(70.093185086346,47.272855398077,49.6328608238036));
#37701=CARTESIAN_POINT('Ctrl Pts',(71.5999715056962,47.0606993885248,48.1245042635199));
#37702=CARTESIAN_POINT('Ctrl Pts',(73.3968818377015,46.8485433789725,47.598003093214));
#37703=CARTESIAN_POINT('Ctrl Pts',(75.193792169707,46.6363873694202,47.071501922908));
#37704=CARTESIAN_POINT('Ctrl Pts',(77.2808264143674,46.4242313598679,47.52685614258));
#37705=CARTESIAN_POINT('Ctrl Pts',(78.6936691722792,46.2120753503156,48.7532951841045));
#37706=CARTESIAN_POINT('Ctrl Pts',(79.9036232471368,46.0303856139129,49.8036137050773));
#37707=CARTESIAN_POINT('Ctrl Pts',(80.6191148022999,45.8486958775103,51.4194578243488));
#37708=CARTESIAN_POINT('Ctrl Pts',(80.633385624059,45.6670061411077,53.0268327355589));
#37709=CARTESIAN_POINT('Ctrl Pts',(80.6244305214574,48.3329938588947,53.0264095113666));
#37710=CARTESIAN_POINT('Ctrl Pts',(80.6282266649446,48.2541084026502,53.7275376620316));
#37711=CARTESIAN_POINT('Ctrl Pts',(80.1802688641959,47.9630669368533,56.3092964517505));
#37712=CARTESIAN_POINT('Ctrl Pts',(76.3127965798036,47.4598694615042,59.5671977602111));
#37713=CARTESIAN_POINT('Ctrl Pts',(70.1919083484634,46.8234014328472,57.6692351964939));
#37714=CARTESIAN_POINT('Ctrl Pts',(68.7803362744653,46.2930114089665,52.535461261843));
#37715=CARTESIAN_POINT('Ctrl Pts',(70.6133799988629,45.8686993898619,49.113348085619));
#37716=CARTESIAN_POINT('Ctrl Pts',(73.808800501213,45.4443873707573,46.9087629319908));
#37717=CARTESIAN_POINT('Ctrl Pts',(78.8849827941382,44.9324855271014,47.707940083055));
#37718=CARTESIAN_POINT('Ctrl Pts',(80.6283333838672,44.5266616882219,51.3152646902586));
#37719=CARTESIAN_POINT('Ctrl Pts',(80.6393222206687,44.3329938588947,53.0263391207439));
#37720=CARTESIAN_POINT('Origin',(74.9879498948689,423.667006141107,53.0228109606356));
#37721=CARTESIAN_POINT('',(80.6254600338732,53.6670061411076,53.018749021103));
#37722=CARTESIAN_POINT('',(80.6254941394426,52.3329938588948,53.0186489958662));
#37723=CARTESIAN_POINT('',(80.6314498948689,423.667006141107,53.0228109606222));
#37724=CARTESIAN_POINT('Ctrl Pts',(80.6254600338732,53.6670061411076,53.018749021103));
#37725=CARTESIAN_POINT('Ctrl Pts',(80.6145961036434,53.5157453159191,54.3612137459823));
#37726=CARTESIAN_POINT('Ctrl Pts',(80.137779540393,53.3644844907305,55.7095665100964));
#37727=CARTESIAN_POINT('Ctrl Pts',(79.2657590440722,53.2132236655419,56.7189534378691));
#37728=CARTESIAN_POINT('Ctrl Pts',(78.0426770694989,53.0010676559896,58.1347033679884));
#37729=CARTESIAN_POINT('Ctrl Pts',(76.0421333948125,52.7889116464373,58.8836255331242));
#37730=CARTESIAN_POINT('Ctrl Pts',(74.1884269720648,52.576755636885,58.6193099606255));
#37731=CARTESIAN_POINT('Ctrl Pts',(72.3347205493172,52.3645996273327,58.3549943881269));
#37732=CARTESIAN_POINT('Ctrl Pts',(70.6278513785079,52.1524436177804,57.0774410779938));
#37733=CARTESIAN_POINT('Ctrl Pts',(69.8486910436903,51.9402876082281,55.3752409220011));
#37734=CARTESIAN_POINT('Ctrl Pts',(69.0695307088726,51.7281315986757,53.6730407660079));
#37735=CARTESIAN_POINT('Ctrl Pts',(69.2180792100468,51.5159755891234,51.5461937641553));
#37736=CARTESIAN_POINT('Ctrl Pts',(70.2295003756775,51.303819579571,49.9704027090604));
#37737=CARTESIAN_POINT('Ctrl Pts',(71.2409215413078,51.0916635700188,48.394611653966));
#37738=CARTESIAN_POINT('Ctrl Pts',(73.1152153713943,50.8795075604665,47.3698765456294));
#37739=CARTESIAN_POINT('Ctrl Pts',(74.9861181344609,50.6673515509142,47.3693945622379));
#37740=CARTESIAN_POINT('Ctrl Pts',(76.8570208975277,50.4551955413619,47.3689125788463));
#37741=CARTESIAN_POINT('Ctrl Pts',(78.7245325935749,50.2430395318096,48.3926837204001));
#37742=CARTESIAN_POINT('Ctrl Pts',(79.7408730892389,50.0308835222573,49.9665956485603));
#37743=CARTESIAN_POINT('Ctrl Pts',(80.2490433370711,49.9248055174811,50.7535516126407));
#37744=CARTESIAN_POINT('Ctrl Pts',(80.5444207848074,49.8187275127049,51.678042773373));
#37745=CARTESIAN_POINT('Ctrl Pts',(80.611992343254,49.7126495079288,52.6188948471453));
#37746=CARTESIAN_POINT('Ctrl Pts',(80.6216839327447,49.6974350523217,52.7538384873408));
#37747=CARTESIAN_POINT('Ctrl Pts',(80.6266892544993,49.6822205967147,52.8891186931059));
#37748=CARTESIAN_POINT('Ctrl Pts',(80.6270010590704,49.6670061411077,53.0243752810309));
#37749=CARTESIAN_POINT('Ctrl Pts',(80.6254941394426,52.3329938588948,53.0186489958662));
#37750=CARTESIAN_POINT('Ctrl Pts',(80.617499907999,52.1937111266308,54.255977736584));
#37751=CARTESIAN_POINT('Ctrl Pts',(80.2173852564667,52.0544283943668,55.4982743983749));
#37752=CARTESIAN_POINT('Ctrl Pts',(79.4671048810938,51.9151456621028,56.4720440015237));
#37753=CARTESIAN_POINT('Ctrl Pts',(78.3242748410938,51.7029896525505,57.9552937186233));
#37754=CARTESIAN_POINT('Ctrl Pts',(76.3690076889641,51.4908336429982,58.8155202978237));
#37755=CARTESIAN_POINT('Ctrl Pts',(74.5049558165395,51.2786776334458,58.6555578082506));
#37756=CARTESIAN_POINT('Ctrl Pts',(72.6409039441153,51.0665216238935,58.4955953186776));
#37757=CARTESIAN_POINT('Ctrl Pts',(70.8680673513958,50.8543656143412,57.3154437603313));
#37758=CARTESIAN_POINT('Ctrl Pts',(69.9904446590788,50.6422096047889,55.6601718277894));
#37759=CARTESIAN_POINT('Ctrl Pts',(69.5516333129203,50.5361316000128,54.8325358615184));
#37760=CARTESIAN_POINT('Ctrl Pts',(69.3366254418624,50.4300535952366,53.8861198016984));
#37761=CARTESIAN_POINT('Ctrl Pts',(69.3499873054311,50.3239755904605,52.9429390126479));
#37762=CARTESIAN_POINT('Ctrl Pts',(69.3633491689999,50.2178975856843,51.9997582235974));
#37763=CARTESIAN_POINT('Ctrl Pts',(69.6050807671954,50.1118195809082,51.0598127053167));
#37764=CARTESIAN_POINT('Ctrl Pts',(70.0671612296048,50.005741576132,50.2449395026388));
#37765=CARTESIAN_POINT('Ctrl Pts',(70.9913221544237,49.7935855665797,48.6151930972829));
#37766=CARTESIAN_POINT('Ctrl Pts',(72.7968785360981,49.5814295570274,47.485735954339));
#37767=CARTESIAN_POINT('Ctrl Pts',(74.6647137408786,49.369273547475,47.378642402046));
#37768=CARTESIAN_POINT('Ctrl Pts',(76.5325489456591,49.1571175379227,47.2715488497529));
#37769=CARTESIAN_POINT('Ctrl Pts',(78.4626629735455,48.9449615283704,48.1868188881107));
#37770=CARTESIAN_POINT('Ctrl Pts',(79.5630169742935,48.732805518818,49.7018473685824));
#37771=CARTESIAN_POINT('Ctrl Pts',(80.2542290065312,48.5995349655103,50.6535464710284));
#37772=CARTESIAN_POINT('Ctrl Pts',(80.6180172462219,48.4662644122025,51.8419106059009));
#37773=CARTESIAN_POINT('Ctrl Pts',(80.6244305214574,48.3329938588947,53.0264095113666));
#37774=CARTESIAN_POINT('Origin',(74.9879498948689,423.667006141107,53.0228109606356));
#37775=CARTESIAN_POINT('',(80.6413657361973,57.6670061411076,53.0214830440174));
#37776=CARTESIAN_POINT('',(80.6403082971391,56.3329938588947,53.0200974632052));
#37777=CARTESIAN_POINT('',(80.6314498948689,423.667006141107,53.0228109606222));
#37778=CARTESIAN_POINT('Ctrl Pts',(80.6413657361973,57.6670061411076,53.0214830440174));
#37779=CARTESIAN_POINT('Ctrl Pts',(80.6414833583072,57.4553480398996,54.888013559151));
#37780=CARTESIAN_POINT('Ctrl Pts',(78.6026480433023,57.0315339291392,58.6340626778927));
#37781=CARTESIAN_POINT('Ctrl Pts',(72.2284115525991,56.3955638088267,59.0977760344396));
#37782=CARTESIAN_POINT('Ctrl Pts',(68.3809746809543,55.7590957801697,53.9882620695771));
#37783=CARTESIAN_POINT('Ctrl Pts',(70.610393675563,55.1226277515128,47.9801654008882));
#37784=CARTESIAN_POINT('Ctrl Pts',(75.8135978038988,54.592237727632,46.8510784551353));
#37785=CARTESIAN_POINT('Ctrl Pts',(79.1304928053609,54.1679257085273,48.8682833122854));
#37786=CARTESIAN_POINT('Ctrl Pts',(80.4347554668827,53.8948745146113,50.9989963543705));
#37787=CARTESIAN_POINT('Ctrl Pts',(80.6298336780962,53.7279013254714,52.4782942349981));
#37788=CARTESIAN_POINT('Ctrl Pts',(80.6254600338732,53.6670061411077,53.018749021103));
#37789=CARTESIAN_POINT('Ctrl Pts',(80.6403082971391,56.3329938588947,53.0200974632052));
#37790=CARTESIAN_POINT('Ctrl Pts',(80.6318782823841,56.1333138506113,54.783408729567));
#37791=CARTESIAN_POINT('Ctrl Pts',(79.7401566050892,55.9336338423279,56.5554703182809));
#37792=CARTESIAN_POINT('Ctrl Pts',(78.3168392779151,55.7339538340445,57.5922327845057));
#37793=CARTESIAN_POINT('Ctrl Pts',(76.8045931244024,55.5217978244922,58.693772140292));
#37794=CARTESIAN_POINT('Ctrl Pts',(74.6922479438257,55.3096418149399,58.9652590151995));
#37795=CARTESIAN_POINT('Ctrl Pts',(72.9442372900428,55.0974858053875,58.2910146121869));
#37796=CARTESIAN_POINT('Ctrl Pts',(72.0702319631515,54.9914078006114,57.9538924106807));
#37797=CARTESIAN_POINT('Ctrl Pts',(71.2873102679585,54.8853297958352,57.3803373896945));
#37798=CARTESIAN_POINT('Ctrl Pts',(70.6789285839257,54.779251791059,56.6594766078752));
#37799=CARTESIAN_POINT('Ctrl Pts',(70.0705468998929,54.6731737862828,55.9386158260558));
#37800=CARTESIAN_POINT('Ctrl Pts',(69.6367052270203,54.5670957815067,55.0704492834031));
#37801=CARTESIAN_POINT('Ctrl Pts',(69.4512397654423,54.4610177767306,54.1522231387392));
#37802=CARTESIAN_POINT('Ctrl Pts',(69.0803088422862,54.2488617671783,52.315770849411));
#37803=CARTESIAN_POINT('Ctrl Pts',(69.7028827643085,54.036705757626,50.2790801520375));
#37804=CARTESIAN_POINT('Ctrl Pts',(71.0428692552329,53.8245497480737,48.9734333447806));
#37805=CARTESIAN_POINT('Ctrl Pts',(72.3828557461571,53.6123937385214,47.6677865375239));
#37806=CARTESIAN_POINT('Ctrl Pts',(74.4402548059832,53.400237728969,47.093183620384));
#37807=CARTESIAN_POINT('Ctrl Pts',(76.2644654877336,53.1880817194168,47.5154934736778));
#37808=CARTESIAN_POINT('Ctrl Pts',(78.0886761694843,52.9759257098644,47.9378033269716));
#37809=CARTESIAN_POINT('Ctrl Pts',(79.6796984731593,52.7637697003121,49.3570259506994));
#37810=CARTESIAN_POINT('Ctrl Pts',(80.3100131610616,52.5516136907598,51.1197736900626));
#37811=CARTESIAN_POINT('Ctrl Pts',(80.526519387434,52.4787404134715,51.7252583288011));
#37812=CARTESIAN_POINT('Ctrl Pts',(80.6296767530029,52.4058671361831,52.3712736970513));
#37813=CARTESIAN_POINT('Ctrl Pts',(80.6254941394426,52.3329938588948,53.0186489958662));
#37814=CARTESIAN_POINT('Origin',(74.9879498948689,423.667006141107,53.0228109606356));
#37815=CARTESIAN_POINT('',(80.6314498948689,61.6670061411077,53.0228109606227));
#37816=CARTESIAN_POINT('',(80.6321857743054,60.3329938588946,53.0296130592723));
#37817=CARTESIAN_POINT('',(80.6314498948689,423.667006141107,53.0228109606222));
#37818=CARTESIAN_POINT('Ctrl Pts',(80.6286885834456,61.6670061411076,53.0279061367502));
#37819=CARTESIAN_POINT('Ctrl Pts',(80.6333660002909,61.6071067734325,53.5597788572812));
#37820=CARTESIAN_POINT('Ctrl Pts',(80.3206569018713,61.335051396205,55.9699752993004));
#37821=CARTESIAN_POINT('Ctrl Pts',(76.8880290754071,60.8508400094253,59.418899735667));
#37822=CARTESIAN_POINT('Ctrl Pts',(70.6327739589726,60.2143719807683,58.0841012989217));
#37823=CARTESIAN_POINT('Ctrl Pts',(68.3763035247955,59.5779039521114,52.0861119846998));
#37824=CARTESIAN_POINT('Ctrl Pts',(71.5643353852583,59.0475139282306,47.82176873059));
#37825=CARTESIAN_POINT('Ctrl Pts',(75.3913197498731,58.623201909126,47.1697729028191));
#37826=CARTESIAN_POINT('Ctrl Pts',(79.0926822278916,58.1988898900212,48.3405947051246));
#37827=CARTESIAN_POINT('Ctrl Pts',(80.6388404574232,57.8801579673485,51.1417900962632));
#37828=CARTESIAN_POINT('Ctrl Pts',(80.6413654595009,57.6675040494519,53.0170921838845));
#37829=CARTESIAN_POINT('Ctrl Pts',(80.6413657361973,57.6670061411076,53.0214830440174));
#37830=CARTESIAN_POINT('Ctrl Pts',(80.6321857743054,60.3329938588946,53.0296130592723));
#37831=CARTESIAN_POINT('Ctrl Pts',(80.6361440296551,60.2850725841441,53.4542934594533));
#37832=CARTESIAN_POINT('Ctrl Pts',(80.3981394867326,60.0249952998413,55.753981612222));
#37833=CARTESIAN_POINT('Ctrl Pts',(77.9529272269266,59.6588400107624,58.4982913970464));
#37834=CARTESIAN_POINT('Ctrl Pts',(74.0841280030346,59.2345279916577,58.8196952732654));
#37835=CARTESIAN_POINT('Ctrl Pts',(70.4968069555375,58.8102159725532,57.3357695377179));
#37836=CARTESIAN_POINT('Ctrl Pts',(68.3331244406284,58.2798259486722,52.4709315643751));
#37837=CARTESIAN_POINT('Ctrl Pts',(71.8627679117568,57.6433579200153,47.1221792238239));
#37838=CARTESIAN_POINT('Ctrl Pts',(78.2582921364095,57.0068898913583,47.2068747390464));
#37839=CARTESIAN_POINT('Ctrl Pts',(80.5882341009387,56.5701018709849,50.9268863207001));
#37840=CARTESIAN_POINT('Ctrl Pts',(80.6408350042226,56.3454698601636,52.9099258251642));
#37841=CARTESIAN_POINT('Ctrl Pts',(80.6403082971391,56.3329938588947,53.0200974632052));
#37842=CARTESIAN_POINT('Origin',(74.9879498948689,423.667006141107,53.0228109606356));
#37843=CARTESIAN_POINT('',(80.6314498948689,65.6670061411076,53.0228109606235));
#37844=CARTESIAN_POINT('',(80.6204112247681,64.3329938588946,53.021333253121));
#37845=CARTESIAN_POINT('',(80.6314498948689,423.667006141107,53.0228109606222));
#37846=CARTESIAN_POINT('Ctrl Pts',(80.6314498948689,65.6670061411076,53.0228109606229));
#37847=CARTESIAN_POINT('Ctrl Pts',(80.6314498948728,65.4742213185052,54.7318077489422));
#37848=CARTESIAN_POINT('Ctrl Pts',(79.8060659192709,65.2814364959028,56.422152109724));
#37849=CARTESIAN_POINT('Ctrl Pts',(78.4584055093459,65.0886516733004,57.4730952299767));
#37850=CARTESIAN_POINT('Ctrl Pts',(77.1107450994209,64.8958668506979,58.5240383502293));
#37851=CARTESIAN_POINT('Ctrl Pts',(75.2702256751649,64.7030820280955,58.9126397065622));
#37852=CARTESIAN_POINT('Ctrl Pts',(73.6127451627063,64.5102972054931,58.4961923829958));
#37853=CARTESIAN_POINT('Ctrl Pts',(71.9552646502477,64.3175123828907,58.0797450594293));
#37854=CARTESIAN_POINT('Ctrl Pts',(70.5170033810742,64.1247275602883,56.867339480919));
#37855=CARTESIAN_POINT('Ctrl Pts',(69.826137149613,63.9319427376859,55.3042099684626));
#37856=CARTESIAN_POINT('Ctrl Pts',(69.1352709181519,63.7391579150834,53.7410804560061));
#37857=CARTESIAN_POINT('Ctrl Pts',(69.2068803054898,63.546373092481,51.8613477992561));
#37858=CARTESIAN_POINT('Ctrl Pts',(70.0146680415436,63.3535882698786,50.3553102844622));
#37859=CARTESIAN_POINT('Ctrl Pts',(70.8224557775975,63.1608034472762,48.8492727696683));
#37860=CARTESIAN_POINT('Ctrl Pts',(72.3487890589391,62.9680186246737,47.7498049531878));
#37861=CARTESIAN_POINT('Ctrl Pts',(74.0331492157606,62.7752338020713,47.4606667775732));
#37862=CARTESIAN_POINT('Ctrl Pts',(75.7175093725822,62.5824489794689,47.1715286019586));
#37863=CARTESIAN_POINT('Ctrl Pts',(77.5231293307851,62.3896641568665,47.6990315230374));
#37864=CARTESIAN_POINT('Ctrl Pts',(78.7869273705887,62.1968793342641,48.8494595029971));
#37865=CARTESIAN_POINT('Ctrl Pts',(79.9447859852104,62.0202549365453,49.9034514424885));
#37866=CARTESIAN_POINT('Ctrl Pts',(80.6314498948653,61.8436305388265,51.4570729301826));
#37867=CARTESIAN_POINT('Ctrl Pts',(80.6314498948689,61.6670061411077,53.0228109606227));
#37868=CARTESIAN_POINT('Ctrl Pts',(80.6204112247681,64.3329938588946,53.021333253121));
#37869=CARTESIAN_POINT('Ctrl Pts',(80.6189023994922,64.2246753081247,53.9846691853807));
#37870=CARTESIAN_POINT('Ctrl Pts',(80.1536906680074,64.0102787525785,55.8927738082689));
#37871=CARTESIAN_POINT('Ctrl Pts',(78.1067448734721,63.6898041922563,57.9921046355568));
#37872=CARTESIAN_POINT('Ctrl Pts',(74.4252754900851,63.2654921731517,59.2240506837341));
#37873=CARTESIAN_POINT('Ctrl Pts',(69.6016913704958,62.7351021492708,56.9698974561461));
#37874=CARTESIAN_POINT('Ctrl Pts',(68.7592374263501,62.0986341206141,50.6171180655309));
#37875=CARTESIAN_POINT('Ctrl Pts',(73.6433787437401,61.4621660919569,46.4873399806718));
#37876=CARTESIAN_POINT('Ctrl Pts',(79.3005017798363,60.8736193380506,48.2131327071158));
#37877=CARTESIAN_POINT('Ctrl Pts',(80.6186201289628,60.4972285936964,51.5741577680182));
#37878=CARTESIAN_POINT('Ctrl Pts',(80.6321857743054,60.3329938588946,53.0296130592723));
#37879=CARTESIAN_POINT('Origin',(74.9879498948689,423.667006141107,53.0228109606356));
#37880=CARTESIAN_POINT('',(80.635553539915,69.6670061411076,53.0185589072328));
#37881=CARTESIAN_POINT('',(80.634082314566,68.3329938588946,53.0192791715721));
#37882=CARTESIAN_POINT('',(80.6314498948689,423.667006141107,53.0228109606222));
#37883=CARTESIAN_POINT('Ctrl Pts',(80.635553539915,69.6670061411076,53.0185589072328));
#37884=CARTESIAN_POINT('Ctrl Pts',(80.6224114597592,69.4863122213936,54.6163488873045));
#37885=CARTESIAN_POINT('Ctrl Pts',(79.913089862654,69.3056183016796,56.2245575530554));
#37886=CARTESIAN_POINT('Ctrl Pts',(78.7132493239764,69.1249243819656,57.2751258742408));
#37887=CARTESIAN_POINT('Ctrl Pts',(77.304494778235,68.9127683724132,58.5086172011074));
#37888=CARTESIAN_POINT('Ctrl Pts',(75.2195336705436,68.7006123628609,58.9733715267185));
#37889=CARTESIAN_POINT('Ctrl Pts',(73.421880772217,68.4884563533086,58.4549880409685));
#37890=CARTESIAN_POINT('Ctrl Pts',(71.6242278738907,68.2763003437562,57.9366045552187));
#37891=CARTESIAN_POINT('Ctrl Pts',(70.1138831849293,68.064144334204,56.4350832581081));
#37892=CARTESIAN_POINT('Ctrl Pts',(69.5738910421763,67.8519883246516,54.6410500236063));
#37893=CARTESIAN_POINT('Ctrl Pts',(69.3038949707998,67.7459103198755,53.7440334063556));
#37894=CARTESIAN_POINT('Ctrl Pts',(69.2764870359754,67.6398323150993,52.7738888047566));
#37895=CARTESIAN_POINT('Ctrl Pts',(69.472486901429,67.5337543103232,51.8512011040834));
#37896=CARTESIAN_POINT('Ctrl Pts',(69.6684867668826,67.427676305547,50.92851340341));
#37897=CARTESIAN_POINT('Ctrl Pts',(70.0878944326141,67.3215983007709,50.0532826036618));
#37898=CARTESIAN_POINT('Ctrl Pts',(70.6992159209813,67.2155202959947,49.3434778924606));
#37899=CARTESIAN_POINT('Ctrl Pts',(71.9218588977159,67.0033642864424,47.923868470058));
#37900=CARTESIAN_POINT('Ctrl Pts',(73.9121571649931,66.7912082768901,47.1659634018436));
#37901=CARTESIAN_POINT('Ctrl Pts',(75.7653062618025,66.5790522673377,47.4230933420581));
#37902=CARTESIAN_POINT('Ctrl Pts',(77.6184553586117,66.3668962577854,47.6802232822726));
#37903=CARTESIAN_POINT('Ctrl Pts',(79.3344552849528,66.1547402482332,48.9523882309157));
#37904=CARTESIAN_POINT('Ctrl Pts',(80.1201456948056,65.9425842386809,50.6520296058731));
#37905=CARTESIAN_POINT('Ctrl Pts',(80.4603341389693,65.8507248728231,51.3879407837776));
#37906=CARTESIAN_POINT('Ctrl Pts',(80.626115678942,65.7588655069654,52.2039917848341));
#37907=CARTESIAN_POINT('Ctrl Pts',(80.6231418722761,65.6670061411076,53.0210100020442));
#37908=CARTESIAN_POINT('Ctrl Pts',(80.6340823145659,68.3329938588947,53.0192791715721));
#37909=CARTESIAN_POINT('Ctrl Pts',(80.6304952755444,68.2703560368814,53.5741188988039));
#37910=CARTESIAN_POINT('Ctrl Pts',(80.3992795908312,68.1016402100919,55.0719021143628));
#37911=CARTESIAN_POINT('Ctrl Pts',(78.6294574171612,67.7207683737503,58.0736920277588));
#37912=CARTESIAN_POINT('Ctrl Pts',(73.5095530650882,67.1903783498695,59.534770382201));
#37913=CARTESIAN_POINT('Ctrl Pts',(68.7078085314535,66.5539103212125,55.2908589708327));
#37914=CARTESIAN_POINT('Ctrl Pts',(69.6873122266739,65.9174422925556,48.9702200830722));
#37915=CARTESIAN_POINT('Ctrl Pts',(75.5299851241042,65.2809742638987,46.3677065188326));
#37916=CARTESIAN_POINT('Ctrl Pts',(79.9731810233658,64.7528247860117,49.2894682583619));
#37917=CARTESIAN_POINT('Ctrl Pts',(80.6218576305895,64.436831317677,52.0978501152049));
#37918=CARTESIAN_POINT('Ctrl Pts',(80.6204112247681,64.3329938588946,53.021333253121));
#37919=CARTESIAN_POINT('Origin',(74.9879498948689,423.667006141107,53.0228109606356));
#37920=CARTESIAN_POINT('',(80.6374169710376,73.6670061411077,53.0261783696298));
#37921=CARTESIAN_POINT('',(80.6381904870062,72.3329938588947,53.0242910303993));
#37922=CARTESIAN_POINT('',(80.6314498948689,423.667006141107,53.0228109606222));
#37923=CARTESIAN_POINT('Ctrl Pts',(80.6374169710376,73.6670061411077,53.0261783696298));
#37924=CARTESIAN_POINT('Ctrl Pts',(80.6395239027795,73.6380709549265,53.2819622128666));
#37925=CARTESIAN_POINT('Ctrl Pts',(80.623649672582,73.6091357687453,53.5375128025017));
#37926=CARTESIAN_POINT('Ctrl Pts',(80.588902319524,73.5802005825642,53.7905152642106));
#37927=CARTESIAN_POINT('Ctrl Pts',(80.3341308547354,73.3680445730119,55.6455575074846));
#37928=CARTESIAN_POINT('Ctrl Pts',(79.0647429823832,73.1558885634595,57.3636127549326));
#37929=CARTESIAN_POINT('Ctrl Pts',(77.367601272787,72.9437325539072,58.1510055404649));
#37930=CARTESIAN_POINT('Ctrl Pts',(75.6704595631907,72.7315765443549,58.9383983259973));
#37931=CARTESIAN_POINT('Ctrl Pts',(73.5455640163505,72.5194205348026,58.7951286496138));
#37932=CARTESIAN_POINT('Ctrl Pts',(71.9614739050273,72.3072645252503,57.7947260906705));
#37933=CARTESIAN_POINT('Ctrl Pts',(71.1694288493658,72.2011865204742,57.2945248111989));
#37934=CARTESIAN_POINT('Ctrl Pts',(70.5125851525835,72.095108515698,56.5800403110874));
#37935=CARTESIAN_POINT('Ctrl Pts',(70.0555325713626,71.9890305109218,55.7548909438627));
#37936=CARTESIAN_POINT('Ctrl Pts',(69.5984799901418,71.8829525061457,54.9297415766381));
#37937=CARTESIAN_POINT('Ctrl Pts',(69.3412185244824,71.7768745013695,53.9939273423004));
#37938=CARTESIAN_POINT('Ctrl Pts',(69.3373259782948,71.6707964965933,53.0571661463347));
#37939=CARTESIAN_POINT('Ctrl Pts',(69.3295408859195,71.458640487041,51.1836437544033));
#37940=CARTESIAN_POINT('Ctrl Pts',(70.3352314714312,71.2464844774887,49.30633351596));
#37941=CARTESIAN_POINT('Ctrl Pts',(71.9029614556376,71.0343284679364,48.2853045850381));
#37942=CARTESIAN_POINT('Ctrl Pts',(73.4706914398441,70.8221724583841,47.2642756541161));
#37943=CARTESIAN_POINT('Ctrl Pts',(75.6004608227454,70.6100164488317,47.0995280307156));
#37944=CARTESIAN_POINT('Ctrl Pts',(77.3081571194718,70.3978604392794,47.8675537996514));
#37945=CARTESIAN_POINT('Ctrl Pts',(79.0158534161979,70.1857044297271,48.6355795685871));
#37946=CARTESIAN_POINT('Ctrl Pts',(80.3014766267492,69.9735484201748,50.3363787298588));
#37947=CARTESIAN_POINT('Ctrl Pts',(80.5780142401291,69.7613924106225,52.1878924745556));
#37948=CARTESIAN_POINT('Ctrl Pts',(80.6190239256628,69.7299303207842,52.4624663218646));
#37949=CARTESIAN_POINT('Ctrl Pts',(80.6378418145131,69.6984682309459,52.7403546822356));
#37950=CARTESIAN_POINT('Ctrl Pts',(80.635553539915,69.6670061411076,53.0185589072328));
#37951=CARTESIAN_POINT('Ctrl Pts',(80.6381904870062,72.3329938588947,53.0242910303993));
#37952=CARTESIAN_POINT('Ctrl Pts',(80.6386945101535,72.3160367656382,53.1741355929961));
#37953=CARTESIAN_POINT('Ctrl Pts',(80.6329254382104,72.2990796723817,53.3239143339577));
#37954=CARTESIAN_POINT('Ctrl Pts',(80.6207036538708,72.2821225791251,53.4731619524118));
#37955=CARTESIAN_POINT('Ctrl Pts',(80.4677927182608,72.0699665695728,55.3404500947464));
#37956=CARTESIAN_POINT('Ctrl Pts',(79.3048148169729,71.8578105600204,57.1245996642243));
#37957=CARTESIAN_POINT('Ctrl Pts',(77.6552999893402,71.6456545504681,58.007423664));
#37958=CARTESIAN_POINT('Ctrl Pts',(76.0057851617079,71.4334985409158,58.8902476637755));
#37959=CARTESIAN_POINT('Ctrl Pts',(73.869733407731,71.2213425313635,58.8717460938492));
#37960=CARTESIAN_POINT('Ctrl Pts',(72.2341915565031,71.0091865218112,57.9601030296608));
#37961=CARTESIAN_POINT('Ctrl Pts',(70.5986497052751,70.7970305122589,57.0484599654722));
#37962=CARTESIAN_POINT('Ctrl Pts',(69.463617756796,70.5848745027065,55.2436754070206));
#37963=CARTESIAN_POINT('Ctrl Pts',(69.3468788376743,70.3727184931542,53.3752674689147));
#37964=CARTESIAN_POINT('Ctrl Pts',(69.2301399185525,70.1605624836019,51.5068595308084));
#37965=CARTESIAN_POINT('Ctrl Pts',(70.1316940287881,69.9484064740495,49.5748282130472));
#37966=CARTESIAN_POINT('Ctrl Pts',(71.6410391704125,69.7362504644972,48.4666912778906));
#37967=CARTESIAN_POINT('Ctrl Pts',(73.1503843120364,69.5240944549449,47.3585543427344));
#37968=CARTESIAN_POINT('Ctrl Pts',(75.2675204850484,69.3119384453926,47.0743117901824));
#37969=CARTESIAN_POINT('Ctrl Pts',(77.0140960782944,69.0997824358403,47.7449466224388));
#37970=CARTESIAN_POINT('Ctrl Pts',(78.7606716715407,68.887626426288,48.4155814546954));
#37971=CARTESIAN_POINT('Ctrl Pts',(80.1366866850208,68.6754704167358,50.0410936717606));
#37972=CARTESIAN_POINT('Ctrl Pts',(80.5208389391871,68.4633144071834,51.8748258785865));
#37973=CARTESIAN_POINT('Ctrl Pts',(80.5994963581544,68.4198742244205,52.2502932639831));
#37974=CARTESIAN_POINT('Ctrl Pts',(80.6365699749868,68.3764340416576,52.6344902632031));
#37975=CARTESIAN_POINT('Ctrl Pts',(80.634082314566,68.3329938588946,53.0192791715721));
#37976=CARTESIAN_POINT('Origin',(74.9879498948689,423.667006141107,53.0228109606356));
#37977=CARTESIAN_POINT('',(80.6230624303151,77.6670061411075,53.0263696586206));
#37978=CARTESIAN_POINT('',(80.623997495512,76.3329938588947,53.0273509825437));
#37979=CARTESIAN_POINT('',(80.6314498948689,423.667006141107,53.0228109606222));
#37980=CARTESIAN_POINT('Ctrl Pts',(80.6230624303151,77.6670061411075,53.0263696586206));
#37981=CARTESIAN_POINT('Ctrl Pts',(80.6260769320359,77.577673678907,53.8215122457189));
#37982=CARTESIAN_POINT('Ctrl Pts',(80.4694078527787,77.4883412167064,54.6152708064669));
#37983=CARTESIAN_POINT('Ctrl Pts',(80.1472801889822,77.3990087545058,55.3341809537919));
#37984=CARTESIAN_POINT('Ctrl Pts',(79.382257955922,77.1868527449535,57.0415234396697));
#37985=CARTESIAN_POINT('Ctrl Pts',(77.6840214498711,76.9746967354012,58.3267082725514));
#37986=CARTESIAN_POINT('Ctrl Pts',(75.8320457850984,76.7625407258489,58.6101388598591));
#37987=CARTESIAN_POINT('Ctrl Pts',(74.9060579527121,76.6564627210727,58.7518541535129));
#37988=CARTESIAN_POINT('Ctrl Pts',(73.9416353306453,76.5503847162965,58.6431308857733));
#37989=CARTESIAN_POINT('Ctrl Pts',(73.0554884509454,76.4443067115204,58.3198473448531));
#37990=CARTESIAN_POINT('Ctrl Pts',(72.1693415712455,76.3382287067442,57.9965638039329));
#37991=CARTESIAN_POINT('Ctrl Pts',(71.3614704339124,76.2321507019681,57.4587199898319));
#37992=CARTESIAN_POINT('Ctrl Pts',(70.7442712211004,76.1260726971919,56.7540201800639));
#37993=CARTESIAN_POINT('Ctrl Pts',(69.5098727954763,75.9139166876396,55.3446205605277));
#37994=CARTESIAN_POINT('Ctrl Pts',(69.0381620679362,75.7017606780873,53.2677969583232));
#37995=CARTESIAN_POINT('Ctrl Pts',(69.5522770720199,75.489604668535,51.4689186567875));
#37996=CARTESIAN_POINT('Ctrl Pts',(70.0663920761035,75.2774486589827,49.6700403552521));
#37997=CARTESIAN_POINT('Ctrl Pts',(71.5663328118108,75.0652926494304,48.1491073543856));
#37998=CARTESIAN_POINT('Ctrl Pts',(73.3592549048717,74.8531366398781,47.6091808854886));
#37999=CARTESIAN_POINT('Ctrl Pts',(75.1521769979327,74.6409806303257,47.0692544165915));
#38000=CARTESIAN_POINT('Ctrl Pts',(77.2380804483475,74.4288246207734,47.510334479664));
#38001=CARTESIAN_POINT('Ctrl Pts',(78.6609546449425,74.2166686112211,48.7268891307503));
#38002=CARTESIAN_POINT('Ctrl Pts',(79.8897682072063,74.03344778785,49.7775223195927));
#38003=CARTESIAN_POINT('Ctrl Pts',(80.6240756444564,73.8502269644788,51.4065265702791));
#38004=CARTESIAN_POINT('Ctrl Pts',(80.6374169710376,73.6670061411077,53.0261783696298));
#38005=CARTESIAN_POINT('Ctrl Pts',(80.623997495512,76.3329938588947,53.0273509825437));
#38006=CARTESIAN_POINT('Ctrl Pts',(80.628953018813,76.2556394896187,53.7142739204978));
#38007=CARTESIAN_POINT('Ctrl Pts',(80.5133497506328,76.1782851203428,54.3997260528318));
#38008=CARTESIAN_POINT('Ctrl Pts',(80.2703413430329,76.1009307510668,55.0371249672848));
#38009=CARTESIAN_POINT('Ctrl Pts',(79.6038541810714,75.8887747415144,56.7852875009471));
#38010=CARTESIAN_POINT('Ctrl Pts',(77.9790086826698,75.6766187319621,58.1719873639615));
#38011=CARTESIAN_POINT('Ctrl Pts',(76.1463891559292,75.4644627224097,58.5561694741797));
#38012=CARTESIAN_POINT('Ctrl Pts',(74.3137696291889,75.2523067128574,58.9403515843979));
#38013=CARTESIAN_POINT('Ctrl Pts',(72.2733760741098,75.0401507033052,58.3220159418202));
#38014=CARTESIAN_POINT('Ctrl Pts',(70.9600714828875,74.8279946937529,56.9879217738211));
#38015=CARTESIAN_POINT('Ctrl Pts',(69.6467668916651,74.6158386842005,55.6538276058221));
#38016=CARTESIAN_POINT('Ctrl Pts',(69.0605512642994,74.4036826746482,53.6039749124017));
#38017=CARTESIAN_POINT('Ctrl Pts',(69.4734667251875,74.1915266650959,51.7776148586989));
#38018=CARTESIAN_POINT('Ctrl Pts',(69.8863821860757,73.9793706555435,49.951254804996));
#38019=CARTESIAN_POINT('Ctrl Pts',(71.2984287352179,73.7672146459912,48.3483873910108));
#38020=CARTESIAN_POINT('Ctrl Pts',(73.0568426519176,73.5550586364389,47.7094367835952));
#38021=CARTESIAN_POINT('Ctrl Pts',(74.8152565686171,73.3429026268866,47.0704861761797));
#38022=CARTESIAN_POINT('Ctrl Pts',(76.9200378528742,73.1307466173343,47.3954523753337));
#38023=CARTESIAN_POINT('Ctrl Pts',(78.412500974108,72.918590607782,48.5280161009088));
#38024=CARTESIAN_POINT('Ctrl Pts',(79.1587325347249,72.8125126030058,49.0942979636963));
#38025=CARTESIAN_POINT('Ctrl Pts',(79.751884554586,72.7064345982297,49.8624792080891));
#38026=CARTESIAN_POINT('Ctrl Pts',(80.1364912013237,72.6003565934535,50.7237841874762));
#38027=CARTESIAN_POINT('Ctrl Pts',(80.4596165750155,72.5112356819339,51.4474053096998));
#38028=CARTESIAN_POINT('Ctrl Pts',(80.6355415069229,72.4221147704143,52.2367572353762));
#38029=CARTESIAN_POINT('Ctrl Pts',(80.6381904870062,72.3329938588947,53.0242910303993));
#38030=CARTESIAN_POINT('Origin',(74.9879498948689,423.667006141107,53.0228109606356));
#38031=CARTESIAN_POINT('',(80.6276716108647,81.6670061411075,53.0174733762821));
#38032=CARTESIAN_POINT('',(80.6254978766381,80.3329938588945,53.0173329105307));
#38033=CARTESIAN_POINT('',(80.6314498948689,423.667006141107,53.0228109606222));
#38034=CARTESIAN_POINT('Ctrl Pts',(80.6276716108647,81.6670061411075,53.0174733762821));
#38035=CARTESIAN_POINT('Ctrl Pts',(80.6152958715597,81.5172764028875,54.3450615231278));
#38036=CARTESIAN_POINT('Ctrl Pts',(79.8112139615196,81.2614686598914,56.6251524598295));
#38037=CARTESIAN_POINT('Ctrl Pts',(77.0839556680519,80.8995829121189,58.5025483215824));
#38038=CARTESIAN_POINT('Ctrl Pts',(73.2334767124565,80.4752708930145,58.9972398405646));
#38039=CARTESIAN_POINT('Ctrl Pts',(68.9385484018002,79.9448808691335,55.8505334134376));
#38040=CARTESIAN_POINT('Ctrl Pts',(69.3439483205791,79.3084128404767,49.4549735833925));
#38041=CARTESIAN_POINT('Ctrl Pts',(74.9361886871511,78.6719448118197,46.3506618849799));
#38042=CARTESIAN_POINT('Ctrl Pts',(79.7843452960189,78.1248092453634,48.9443577070945));
#38043=CARTESIAN_POINT('Ctrl Pts',(80.6189177802548,77.7898296884593,51.9331250441539));
#38044=CARTESIAN_POINT('Ctrl Pts',(80.6230624303151,77.6670061411075,53.0263696586206));
#38045=CARTESIAN_POINT('Ctrl Pts',(80.6254978766381,80.3329938588945,53.0173329105307));
#38046=CARTESIAN_POINT('Ctrl Pts',(80.6172902306014,80.1952422135991,54.2420270657874));
#38047=CARTESIAN_POINT('Ctrl Pts',(80.225754257094,80.0574905683037,55.4722729920021));
#38048=CARTESIAN_POINT('Ctrl Pts',(79.4909454765108,79.9197389230084,56.4408613921962));
#38049=CARTESIAN_POINT('Ctrl Pts',(78.3592413989422,79.7075829134561,57.932617439416));
#38050=CARTESIAN_POINT('Ctrl Pts',(76.4132897193138,79.4954269039038,58.8037184020166));
#38051=CARTESIAN_POINT('Ctrl Pts',(74.5469455541935,79.2832708943514,58.6576511033595));
#38052=CARTESIAN_POINT('Ctrl Pts',(72.6806013890734,79.0711148847992,58.5115838047024));
#38053=CARTESIAN_POINT('Ctrl Pts',(70.8938647384612,78.8589588752468,57.3483482447878));
#38054=CARTESIAN_POINT('Ctrl Pts',(70.0080197895437,78.6468028656945,55.6986910227933));
#38055=CARTESIAN_POINT('Ctrl Pts',(69.1221748406262,78.4346468561422,54.0490338007986));
#38056=CARTESIAN_POINT('Ctrl Pts',(69.1372215934034,78.2224908465899,51.9129549167242));
#38057=CARTESIAN_POINT('Ctrl Pts',(70.0458418447529,78.0103348370376,50.2775079992128));
#38058=CARTESIAN_POINT('Ctrl Pts',(70.9544620961024,77.7981788274852,48.6420610817015));
#38059=CARTESIAN_POINT('Ctrl Pts',(72.7566558460243,77.5860228179329,47.5072461307536));
#38060=CARTESIAN_POINT('Ctrl Pts',(74.6261151221574,77.3738668083806,47.3836792435535));
#38061=CARTESIAN_POINT('Ctrl Pts',(75.5608447602238,77.2677888036044,47.3218957999535));
#38062=CARTESIAN_POINT('Ctrl Pts',(76.5123907798431,77.1617107988283,47.5129243722904));
#38063=CARTESIAN_POINT('Ctrl Pts',(77.3675494076294,77.0556327940521,47.9110101187751));
#38064=CARTESIAN_POINT('Ctrl Pts',(78.2227080354158,76.949554789276,48.3090958652599));
#38065=CARTESIAN_POINT('Ctrl Pts',(78.9814792713693,76.8434767844998,48.9142387858926));
#38066=CARTESIAN_POINT('Ctrl Pts',(79.5359719577514,76.7373987797237,49.669271600366));
#38067=CARTESIAN_POINT('Ctrl Pts',(80.2406093027247,76.6025971394473,50.6287510142958));
#38068=CARTESIAN_POINT('Ctrl Pts',(80.6153617497143,76.467795499171,51.8302842926289));
#38069=CARTESIAN_POINT('Ctrl Pts',(80.623997495512,76.3329938588947,53.0273509825437));
#38070=CARTESIAN_POINT('Origin',(74.9879498948689,423.667006141107,53.0228109606356));
#38071=CARTESIAN_POINT('',(80.6387596333603,85.6670061411075,53.023247336888));
#38072=CARTESIAN_POINT('',(80.6402800254983,84.3329938588945,53.0213524957134));
#38073=CARTESIAN_POINT('',(80.6314498948689,423.667006141107,53.0228109606222));
#38074=CARTESIAN_POINT('Ctrl Pts',(80.6387596333603,85.6670061411075,53.023247336888));
#38075=CARTESIAN_POINT('Ctrl Pts',(80.6397095806137,85.5629571316442,53.942111686572));
#38076=CARTESIAN_POINT('Ctrl Pts',(80.151294702481,85.3528301174047,55.7994486431996));
#38077=CARTESIAN_POINT('Ctrl Pts',(77.580926274119,84.9305470936132,58.683946013413));
#38078=CARTESIAN_POINT('Ctrl Pts',(72.2748837406891,84.4001570697319,59.1244947231283));
#38079=CARTESIAN_POINT('Ctrl Pts',(68.3872132968793,83.7636890410755,54.030031733356));
#38080=CARTESIAN_POINT('Ctrl Pts',(70.5737567372417,83.1272210124182,48.0192970676245));
#38081=CARTESIAN_POINT('Ctrl Pts',(76.8101842784523,82.4907529837615,46.5991298374534));
#38082=CARTESIAN_POINT('Ctrl Pts',(80.3051414638775,82.0040146933244,50.034716227933));
#38083=CARTESIAN_POINT('Ctrl Pts',(80.6328313825237,81.7294324124398,52.4639669128515));
#38084=CARTESIAN_POINT('Ctrl Pts',(80.6276716108647,81.6670061411075,53.0174733762821));
#38085=CARTESIAN_POINT('Ctrl Pts',(80.6402800254983,84.3329938588945,53.0213524957134));
#38086=CARTESIAN_POINT('Ctrl Pts',(80.6315430011957,84.1348449375797,54.7708123482206));
#38087=CARTESIAN_POINT('Ctrl Pts',(78.8173730615227,83.7245400067127,58.4058088718737));
#38088=CARTESIAN_POINT('Ctrl Pts',(72.6215538909905,83.102079066293,59.2665588153995));
#38089=CARTESIAN_POINT('Ctrl Pts',(68.4535757982522,82.4656110376363,54.3987571295987));
#38090=CARTESIAN_POINT('Ctrl Pts',(69.9948804987645,81.9352210137553,49.3024299862164));
#38091=CARTESIAN_POINT('Ctrl Pts',(73.3695905296702,81.5109089946509,47.3835136009241));
#38092=CARTESIAN_POINT('Ctrl Pts',(77.2483078732814,81.0865969755459,47.2208493614383));
#38093=CARTESIAN_POINT('Ctrl Pts',(80.2162883538608,80.6939585969607,49.8143795435911));
#38094=CARTESIAN_POINT('Ctrl Pts',(80.62993110634,80.4073982231515,52.3558338058509));
#38095=CARTESIAN_POINT('Ctrl Pts',(80.6254978766381,80.3329938588945,53.0173329105307));
#38096=CARTESIAN_POINT('Origin',(74.9879498948689,423.667006141107,53.0228109606356));
#38097=CARTESIAN_POINT('',(80.631286606836,89.6670061411074,53.0264418435404));
#38098=CARTESIAN_POINT('',(80.6317605038146,88.3329938588946,53.0278742010531));
#38099=CARTESIAN_POINT('',(80.6314498948689,423.667006141107,53.0228109606222));
#38100=CARTESIAN_POINT('Ctrl Pts',(80.6312866068361,89.6670061411075,53.0264418435404));
#38101=CARTESIAN_POINT('Ctrl Pts',(80.6344559667197,89.6086378604009,53.5442211596003));
#38102=CARTESIAN_POINT('Ctrl Pts',(80.3234366051561,89.3381135701419,55.9395580373531));
#38103=CARTESIAN_POINT('Ctrl Pts',(76.9406356429825,88.8554332703309,59.4085991706795));
#38104=CARTESIAN_POINT('Ctrl Pts',(70.6648736271285,88.2189652416738,58.1115464523212));
#38105=CARTESIAN_POINT('Ctrl Pts',(68.3743024533118,87.5824972130169,52.1396801497238));
#38106=CARTESIAN_POINT('Ctrl Pts',(72.1515458643403,86.9460291843599,46.9780587327407));
#38107=CARTESIAN_POINT('Ctrl Pts',(78.5477530123006,86.3095611557031,47.3731141139413));
#38108=CARTESIAN_POINT('Ctrl Pts',(80.6270392993929,85.8832201412856,51.1138794115315));
#38109=CARTESIAN_POINT('Ctrl Pts',(80.6387411090271,85.6690351364204,53.0053291321087));
#38110=CARTESIAN_POINT('Ctrl Pts',(80.6387596333603,85.6670061411075,53.023247336888));
#38111=CARTESIAN_POINT('Ctrl Pts',(80.6317605038146,88.3329938588946,53.0278742010531));
#38112=CARTESIAN_POINT('Ctrl Pts',(80.6354316875401,88.2866036711127,53.438801427614));
#38113=CARTESIAN_POINT('Ctrl Pts',(80.4060682461895,88.0280574737784,55.7248623794342));
#38114=CARTESIAN_POINT('Ctrl Pts',(77.2955260761042,87.5573552668916,59.2885359377501));
#38115=CARTESIAN_POINT('Ctrl Pts',(70.9567606325384,86.9208872382348,58.3464174285945));
#38116=CARTESIAN_POINT('Ctrl Pts',(68.7786383180496,86.3904972143539,53.4880273953303));
#38117=CARTESIAN_POINT('Ctrl Pts',(70.0682487881018,85.9661851952494,49.8263593707863));
#38118=CARTESIAN_POINT('Ctrl Pts',(72.8900068067502,85.5418731761447,47.1601655348787));
#38119=CARTESIAN_POINT('Ctrl Pts',(78.2142824574917,85.0114831522641,47.1762691716988));
#38120=CARTESIAN_POINT('Ctrl Pts',(80.5808862801361,84.5731640449218,50.9013697299768));
#38121=CARTESIAN_POINT('Ctrl Pts',(80.6408976431443,84.347000947132,52.8976836997423));
#38122=CARTESIAN_POINT('Ctrl Pts',(80.6402800254983,84.3329938588945,53.0213524957134));
#38123=CARTESIAN_POINT('Origin',(74.9879498948689,423.667006141107,53.0228109606356));
#38124=CARTESIAN_POINT('',(80.6204621564745,93.6670061411077,53.0221988416072));
#38125=CARTESIAN_POINT('',(80.6222974695971,92.3329938588945,53.0225854127507));
#38126=CARTESIAN_POINT('',(80.6314498948689,423.667006141107,53.0228109606222));
#38127=CARTESIAN_POINT('Ctrl Pts',(80.6204621564745,93.6670061411077,53.0221988416072));
#38128=CARTESIAN_POINT('Ctrl Pts',(80.6183893468973,93.5482405843816,54.078428328712));
#38129=CARTESIAN_POINT('Ctrl Pts',(80.335268865848,93.4294750276555,55.1354937426111));
#38130=CARTESIAN_POINT('Ctrl Pts',(79.7794841936502,93.3107094709294,56.0231975011701));
#38131=CARTESIAN_POINT('Ctrl Pts',(78.7866621880601,93.0985534613771,57.6089408115375));
#38132=CARTESIAN_POINT('Ctrl Pts',(76.9237630301127,92.8863974518248,58.6542475278061));
#38133=CARTESIAN_POINT('Ctrl Pts',(75.0514311231125,92.6742414422725,58.6757755010019));
#38134=CARTESIAN_POINT('Ctrl Pts',(73.1790992161119,92.4620854327202,58.6973034741976));
#38135=CARTESIAN_POINT('Ctrl Pts',(71.2973345600582,92.2499294231679,57.6950527043195));
#38136=CARTESIAN_POINT('Ctrl Pts',(70.2676506174,92.0377734136155,56.1316182871956));
#38137=CARTESIAN_POINT('Ctrl Pts',(69.2379666747419,91.8256174040632,54.5681838700718));
#38138=CARTESIAN_POINT('Ctrl Pts',(69.0603634454785,91.6134613945108,52.4435658057023));
#38139=CARTESIAN_POINT('Ctrl Pts',(69.8195899162345,91.4013053849585,50.7319392723414));
#38140=CARTESIAN_POINT('Ctrl Pts',(70.5788163869904,91.1891493754062,49.0203127389806));
#38141=CARTESIAN_POINT('Ctrl Pts',(72.2748725577659,90.976993365854,47.7216777366283));
#38142=CARTESIAN_POINT('Ctrl Pts',(74.1238093241108,90.7648373563017,47.4358277493677));
#38143=CARTESIAN_POINT('Ctrl Pts',(75.9727460904561,90.5526813467493,47.1499777621071));
#38144=CARTESIAN_POINT('Ctrl Pts',(77.974563452371,90.3405253371969,47.8769127899383));
#38145=CARTESIAN_POINT('Ctrl Pts',(79.2190840426557,90.1283693276446,49.277382447264));
#38146=CARTESIAN_POINT('Ctrl Pts',(79.8413443377979,90.0222913228685,49.9776172759268));
#38147=CARTESIAN_POINT('Ctrl Pts',(80.2742804400326,89.9162133180923,50.8462357619631));
#38148=CARTESIAN_POINT('Ctrl Pts',(80.4845719094074,89.8101353133162,51.7657715351335));
#38149=CARTESIAN_POINT('Ctrl Pts',(80.5791527605388,89.7624255892466,52.179342643514));
#38150=CARTESIAN_POINT('Ctrl Pts',(80.6286959996827,89.714715865177,52.6032135421563));
#38151=CARTESIAN_POINT('Ctrl Pts',(80.631286606836,89.6670061411074,53.0264418435404));
#38152=CARTESIAN_POINT('Ctrl Pts',(80.6222974695971,92.3329938588945,53.0225854127507));
#38153=CARTESIAN_POINT('Ctrl Pts',(80.6225629497166,92.2262063950931,53.9726808477364));
#38154=CARTESIAN_POINT('Ctrl Pts',(79.9442096617391,91.9072629217394,56.8106361137177));
#38155=CARTESIAN_POINT('Ctrl Pts',(75.4352492268543,91.3761634388334,59.6854827972209));
#38156=CARTESIAN_POINT('Ctrl Pts',(70.6049911897418,90.8457734149526,57.4456663254745));
#38157=CARTESIAN_POINT('Ctrl Pts',(69.1775862436694,90.4214613958479,53.8354830882459));
#38158=CARTESIAN_POINT('Ctrl Pts',(69.5597087935644,89.9971493767433,49.9722085389421));
#38159=CARTESIAN_POINT('Ctrl Pts',(73.5900826298085,89.4667593528626,46.493091226704));
#38160=CARTESIAN_POINT('Ctrl Pts',(79.2838657016368,88.8766815119875,48.1901383461276));
#38161=CARTESIAN_POINT('Ctrl Pts',(80.618642281703,88.498759680665,51.5595100349322));
#38162=CARTESIAN_POINT('Ctrl Pts',(80.6317605038146,88.3329938588946,53.0278742010531));
#38163=CARTESIAN_POINT('Origin',(74.9879498948689,423.667006141107,53.0228109606356));
#38164=CARTESIAN_POINT('',(80.6362700731203,97.6670061411075,53.016734409587));
#38165=CARTESIAN_POINT('',(80.6327545556523,96.3329938588947,53.0173721012319));
#38166=CARTESIAN_POINT('',(80.6314498948689,423.667006141107,53.0228109606222));
#38167=CARTESIAN_POINT('Ctrl Pts',(80.6362700731203,97.6670061411075,53.016734409587));
#38168=CARTESIAN_POINT('Ctrl Pts',(80.6225472232024,97.487843308362,54.6012631912224));
#38169=CARTESIAN_POINT('Ctrl Pts',(79.924533412689,97.3086804756165,56.1986225284727));
#38170=CARTESIAN_POINT('Ctrl Pts',(78.7426840125468,97.1295176428711,57.2491580436995));
#38171=CARTESIAN_POINT('Ctrl Pts',(77.3431947949246,96.9173616333188,58.4931516744551));
#38172=CARTESIAN_POINT('Ctrl Pts',(75.2652637017498,96.7052056237665,58.9703803392536));
#38173=CARTESIAN_POINT('Ctrl Pts',(73.4626676116383,96.4930496142142,58.4651838088526));
#38174=CARTESIAN_POINT('Ctrl Pts',(71.6600715215263,96.2808936046619,57.9599872784515));
#38175=CARTESIAN_POINT('Ctrl Pts',(70.132810434478,96.0687375951095,56.47236555285));
#38176=CARTESIAN_POINT('Ctrl Pts',(69.5836633530081,95.8565815855572,54.6822460857428));
#38177=CARTESIAN_POINT('Ctrl Pts',(69.0345162715382,95.6444255760048,52.8921266186361));
#38178=CARTESIAN_POINT('Ctrl Pts',(69.4634831956461,95.4322695664525,50.7995094100236));
#38179=CARTESIAN_POINT('Ctrl Pts',(70.6719858524335,95.2201135569002,49.371294191754));
#38180=CARTESIAN_POINT('Ctrl Pts',(71.880488509221,95.0079575473479,47.9430789734843));
#38181=CARTESIAN_POINT('Ctrl Pts',(73.8685268986879,94.7958015377957,47.1792657455576));
#38182=CARTESIAN_POINT('Ctrl Pts',(75.7264635754982,94.5836455282434,47.4205499466461));
#38183=CARTESIAN_POINT('Ctrl Pts',(76.6554319139033,94.4775675234672,47.5411920471903));
#38184=CARTESIAN_POINT('Ctrl Pts',(77.5518748241443,94.371489518691,47.9131085049883));
#38185=CARTESIAN_POINT('Ctrl Pts',(78.3136094973527,94.2654115139148,48.4694616553019));
#38186=CARTESIAN_POINT('Ctrl Pts',(79.0753441705613,94.1593335091386,49.0258148056156));
#38187=CARTESIAN_POINT('Ctrl Pts',(79.7023706067374,94.0532555043625,49.7666046484449));
#38188=CARTESIAN_POINT('Ctrl Pts',(80.099930755316,93.9471774995863,50.6148278610756));
#38189=CARTESIAN_POINT('Ctrl Pts',(80.4499403768181,93.8537870467601,51.3615985991982));
#38190=CARTESIAN_POINT('Ctrl Pts',(80.6220920955778,93.7603965939339,52.1916402789372));
#38191=CARTESIAN_POINT('Ctrl Pts',(80.6204621564745,93.6670061411077,53.0221988416072));
#38192=CARTESIAN_POINT('Ctrl Pts',(80.6327545556523,96.3329938588947,53.0173721012319));
#38193=CARTESIAN_POINT('Ctrl Pts',(80.6186391321579,96.1658091190738,54.4991059289975));
#38194=CARTESIAN_POINT('Ctrl Pts',(80.0202136543595,95.9986243792528,55.9913418499903));
#38195=CARTESIAN_POINT('Ctrl Pts',(78.9748718282735,95.831439639432,57.0309993077515));
#38196=CARTESIAN_POINT('Ctrl Pts',(77.6483419627002,95.6192836298797,58.3503157583809));
#38197=CARTESIAN_POINT('Ctrl Pts',(75.6021251094401,95.4071276203275,58.9408272947501));
#38198=CARTESIAN_POINT('Ctrl Pts',(73.7717246599809,95.1949716107751,58.5411011943371));
#38199=CARTESIAN_POINT('Ctrl Pts',(72.8565244352513,95.088893605999,58.3412381441306));
#38200=CARTESIAN_POINT('Ctrl Pts',(71.995278311472,94.9828156012228,57.8938156847286));
#38201=CARTESIAN_POINT('Ctrl Pts',(71.2840608794616,94.8767375964466,57.2741881315675));
#38202=CARTESIAN_POINT('Ctrl Pts',(70.5728434474512,94.7706595916704,56.6545605784064));
#38203=CARTESIAN_POINT('Ctrl Pts',(70.0116547072098,94.6645815868943,55.8627279314863));
#38204=CARTESIAN_POINT('Ctrl Pts',(69.688300068699,94.5585035821182,54.983535991159));
#38205=CARTESIAN_POINT('Ctrl Pts',(69.0415907916772,94.3463475725659,53.2251521105042));
#38206=CARTESIAN_POINT('Ctrl Pts',(69.3462179215783,94.1341915630135,51.1173310562202));
#38207=CARTESIAN_POINT('Ctrl Pts',(70.4713707929385,93.9220355534611,49.6225707419123));
#38208=CARTESIAN_POINT('Ctrl Pts',(71.5965236642985,93.7098795439088,48.1278104276046));
#38209=CARTESIAN_POINT('Ctrl Pts',(73.5422022771169,93.4977235343564,47.2461108532722));
#38210=CARTESIAN_POINT('Ctrl Pts',(75.4094828660979,93.2855675248041,47.3852274432813));
#38211=CARTESIAN_POINT('Ctrl Pts',(77.2767634550792,93.0734115152518,47.5243440332904));
#38212=CARTESIAN_POINT('Ctrl Pts',(79.0656460202229,92.8612555056996,48.6842767876416));
#38213=CARTESIAN_POINT('Ctrl Pts',(79.9574615217452,92.6490994961473,50.3302540990467));
#38214=CARTESIAN_POINT('Ctrl Pts',(80.4003870022527,92.5437309503964,51.1477385342401));
#38215=CARTESIAN_POINT('Ctrl Pts',(80.6220355169939,92.4383624046455,52.0851141895814));
#38216=CARTESIAN_POINT('Ctrl Pts',(80.6222974695971,92.3329938588945,53.0225854127507));
#38217=CARTESIAN_POINT('Origin',(74.9879498948689,423.667006141107,53.0228109606356));
#38218=CARTESIAN_POINT('',(80.6374103558004,101.667006141107,53.0273186999381));
#38219=CARTESIAN_POINT('',(80.6400616791356,100.332993858895,53.0267327569543));
#38220=CARTESIAN_POINT('',(80.6314498948689,423.667006141107,53.0228109606222));
#38221=CARTESIAN_POINT('Ctrl Pts',(80.6374103558004,101.667006141107,53.0273186999381));
#38222=CARTESIAN_POINT('Ctrl Pts',(80.6393935608058,101.639602041895,53.2696633040341));
#38223=CARTESIAN_POINT('Ctrl Pts',(80.5154322052391,101.40004193313,55.3859628634931));
#38224=CARTESIAN_POINT('Ctrl Pts',(77.8414071731253,100.948325814813,59.0542315289232));
#38225=CARTESIAN_POINT('Ctrl Pts',(71.4557480292651,100.311857786156,58.689182577611));
#38226=CARTESIAN_POINT('Ctrl Pts',(68.3107929723319,99.6753897574989,53.1055643668355));
#38227=CARTESIAN_POINT('Ctrl Pts',(70.811068570169,99.144999733618,48.404841819497));
#38228=CARTESIAN_POINT('Ctrl Pts',(74.4938206403223,98.7206877145134,47.176735522705));
#38229=CARTESIAN_POINT('Ctrl Pts',(78.330459889719,98.2963756954088,47.7692784801554));
#38230=CARTESIAN_POINT('Ctrl Pts',(80.4851494606274,97.9451485042735,50.5600566397906));
#38231=CARTESIAN_POINT('Ctrl Pts',(80.6387971620634,97.6999993179143,52.7249404172344));
#38232=CARTESIAN_POINT('Ctrl Pts',(80.6362700731203,97.6670061411075,53.016734409587));
#38233=CARTESIAN_POINT('Ctrl Pts',(80.6400616791356,100.332993858895,53.0267327569543));
#38234=CARTESIAN_POINT('Ctrl Pts',(80.6407843424398,100.317567852607,53.1628880610317));
#38235=CARTESIAN_POINT('Ctrl Pts',(80.6362648167285,100.302141846319,53.2989746798747));
#38236=CARTESIAN_POINT('Ctrl Pts',(80.6263460537318,100.286715840031,53.4346471959759));
#38237=CARTESIAN_POINT('Ctrl Pts',(80.4899319269776,100.074559830478,55.3005701759463));
#38238=CARTESIAN_POINT('Ctrl Pts',(79.3322583638292,99.8624038209258,57.0881661052152));
#38239=CARTESIAN_POINT('Ctrl Pts',(77.6881992837944,99.6502478113736,57.9866183866898));
#38240=CARTESIAN_POINT('Ctrl Pts',(76.8661697437769,99.5441698065974,58.4358445274272));
#38241=CARTESIAN_POINT('Ctrl Pts',(75.9225438245377,99.4380918018213,58.6627847562159));
#38242=CARTESIAN_POINT('Ctrl Pts',(74.9792695105176,99.3320137970451,58.6613326054378));
#38243=CARTESIAN_POINT('Ctrl Pts',(74.0359951964976,99.225935792269,58.6598804546596));
#38244=CARTESIAN_POINT('Ctrl Pts',(73.0930724876966,99.1198577874928,58.4300359243145));
#38245=CARTESIAN_POINT('Ctrl Pts',(72.2724299890143,99.0137797827166,57.978280924852));
#38246=CARTESIAN_POINT('Ctrl Pts',(70.6311449916498,98.8016237731643,57.074770925927));
#38247=CARTESIAN_POINT('Ctrl Pts',(69.4789808347601,98.5894677636121,55.2836190505323));
#38248=CARTESIAN_POINT('Ctrl Pts',(69.3483124386082,98.3773117540598,53.417284902689));
#38249=CARTESIAN_POINT('Ctrl Pts',(69.2176440424562,98.1651557445075,51.5509507548455));
#38250=CARTESIAN_POINT('Ctrl Pts',(70.108471407042,97.9529997349551,49.6094343345535));
#38251=CARTESIAN_POINT('Ctrl Pts',(71.609485997445,97.7408437254028,48.4900392197709));
#38252=CARTESIAN_POINT('Ctrl Pts',(73.1105005878481,97.5286877158505,47.3706441049884));
#38253=CARTESIAN_POINT('Ctrl Pts',(75.2217024040683,97.3165317062982,47.0733702957154));
#38254=CARTESIAN_POINT('Ctrl Pts',(76.9743338504003,97.1043756967459,47.7312906645623));
#38255=CARTESIAN_POINT('Ctrl Pts',(78.7269652967321,96.8922196871936,48.3892110334092));
#38256=CARTESIAN_POINT('Ctrl Pts',(80.1210263731757,96.6800636776413,50.0023255803758));
#38257=CARTESIAN_POINT('Ctrl Pts',(80.5146354724544,96.4679076680889,51.832943536304));
#38258=CARTESIAN_POINT('Ctrl Pts',(80.5980698329034,96.4229363983575,52.2209844597968));
#38259=CARTESIAN_POINT('Ctrl Pts',(80.6365514842358,96.3779651286261,52.6187983336141));
#38260=CARTESIAN_POINT('Ctrl Pts',(80.6327545556523,96.3329938588947,53.0173721012319));
#38261=CARTESIAN_POINT('Origin',(74.9879498948689,423.667006141107,53.0228109606356));
#38262=CARTESIAN_POINT('',(80.6232183355818,105.667006141107,53.0253975325881));
#38263=CARTESIAN_POINT('',(80.6224354235563,104.332993858895,53.0256136329225));
#38264=CARTESIAN_POINT('',(80.6314498948689,423.667006141107,53.0228109606222));
#38265=CARTESIAN_POINT('Ctrl Pts',(80.6232183355818,105.667006141107,53.0253975325881));
#38266=CARTESIAN_POINT('Ctrl Pts',(80.6260644232382,105.579204765875,53.8062098106832));
#38267=CARTESIAN_POINT('Ctrl Pts',(80.1085346718932,105.279247381091,56.469692650254));
#38268=CARTESIAN_POINT('Ctrl Pts',(76.0367440446578,104.767133986754,59.6170696871648));
#38269=CARTESIAN_POINT('Ctrl Pts',(70.0009775363973,104.130665958098,57.4636869316869));
#38270=CARTESIAN_POINT('Ctrl Pts',(68.8062846772482,103.600275934217,52.2751534679328));
#38271=CARTESIAN_POINT('Ctrl Pts',(70.781449457728,103.175963915112,48.9330535328036));
#38272=CARTESIAN_POINT('Ctrl Pts',(74.0666489726483,102.751651896007,46.8646309372967));
#38273=CARTESIAN_POINT('Ctrl Pts',(79.0170332829222,102.248665971339,47.8586964864205));
#38274=CARTESIAN_POINT('Ctrl Pts',(80.6240400599734,101.851758051447,51.3934890958369));
#38275=CARTESIAN_POINT('Ctrl Pts',(80.6374103558004,101.667006141107,53.0273186999381));
#38276=CARTESIAN_POINT('Ctrl Pts',(80.6224354235563,104.332993858895,53.0256136329225));
#38277=CARTESIAN_POINT('Ctrl Pts',(80.626288657042,104.257170576587,53.6993939361133));
#38278=CARTESIAN_POINT('Ctrl Pts',(80.3583492568762,104.075269289503,55.3132815258189));
#38279=CARTESIAN_POINT('Ctrl Pts',(78.8282293448942,103.787289997644,57.4582382784806));
#38280=CARTESIAN_POINT('Ctrl Pts',(75.3777508129794,103.362977978539,59.2373126971688));
#38281=CARTESIAN_POINT('Ctrl Pts',(70.2667783164759,102.832587954658,57.7452903541108));
#38282=CARTESIAN_POINT('Ctrl Pts',(68.4651765033714,102.196119926002,51.5953500665264));
#38283=CARTESIAN_POINT('Ctrl Pts',(72.6622400074956,101.559651897344,46.7689060980581));
#38284=CARTESIAN_POINT('Ctrl Pts',(78.8396299348509,100.938609874976,47.6581366381825));
#38285=CARTESIAN_POINT('Ctrl Pts',(80.6308454535261,100.529723862159,51.2903252308906));
#38286=CARTESIAN_POINT('Ctrl Pts',(80.6400616791356,100.332993858895,53.0267327569543));
#38287=CARTESIAN_POINT('Origin',(74.9879498948689,423.667006141107,53.0228109606356));
#38288=CARTESIAN_POINT('',(80.627375492094,109.667006141107,53.018034188696));
#38289=CARTESIAN_POINT('',(80.6285061370469,108.332993858894,53.0199845307064));
#38290=CARTESIAN_POINT('',(80.6314498948689,423.667006141107,53.0228109606222));
#38291=CARTESIAN_POINT('Ctrl Pts',(80.627375492094,109.667006141107,53.018034188696));
#38292=CARTESIAN_POINT('Ctrl Pts',(80.6172081439586,109.518807489856,54.3334327993462));
#38293=CARTESIAN_POINT('Ctrl Pts',(79.5040108698863,109.158452829052,57.5480756578864));
#38294=CARTESIAN_POINT('Ctrl Pts',(74.1348045617336,108.585942158696,59.6457571128379));
#38295=CARTESIAN_POINT('Ctrl Pts',(69.8305489765598,108.055552134815,56.5118211866107));
#38296=CARTESIAN_POINT('Ctrl Pts',(69.1302854250172,107.631240115711,52.6933740094433));
#38297=CARTESIAN_POINT('Ctrl Pts',(70.2542803117838,107.206928096606,48.9775237190036));
#38298=CARTESIAN_POINT('Ctrl Pts',(74.8827889425443,106.676538072725,46.3459693518712));
#38299=CARTESIAN_POINT('Ctrl Pts',(79.7705207976768,106.1278714193,48.9205634374283));
#38300=CARTESIAN_POINT('Ctrl Pts',(80.6191873715017,105.791360775428,51.9195193494878));
#38301=CARTESIAN_POINT('Ctrl Pts',(80.6232183355818,105.667006141107,53.0253975325881));
#38302=CARTESIAN_POINT('Ctrl Pts',(80.6285061370469,108.332993858894,53.0199845307063));
#38303=CARTESIAN_POINT('Ctrl Pts',(80.6273255247201,108.302851305344,53.287752480045));
#38304=CARTESIAN_POINT('Ctrl Pts',(80.5383454663005,108.166630747017,54.498662736846));
#38305=CARTESIAN_POINT('Ctrl Pts',(79.3572700732904,107.818254179138,57.4591402729806));
#38306=CARTESIAN_POINT('Ctrl Pts',(74.52013864804,107.287864155257,59.6840740039152));
#38307=CARTESIAN_POINT('Ctrl Pts',(69.1272472113271,106.6513961266,56.2222455007014));
#38308=CARTESIAN_POINT('Ctrl Pts',(69.1311857674209,106.014928097943,49.8261617046435));
#38309=CARTESIAN_POINT('Ctrl Pts',(74.5085221507447,105.378460069286,46.362903576955));
#38310=CARTESIAN_POINT('Ctrl Pts',(79.6429858726333,104.817815322937,48.7087080503247));
#38311=CARTESIAN_POINT('Ctrl Pts',(80.6155071844479,104.469326586139,51.8141347374896));
#38312=CARTESIAN_POINT('Ctrl Pts',(80.6224354235563,104.332993858895,53.0256136329225));
#38313=CARTESIAN_POINT('Origin',(74.9879498948689,423.667006141107,53.0228109606356));
#38314=CARTESIAN_POINT('',(80.6411686659135,113.667006141107,53.0214655157299));
#38315=CARTESIAN_POINT('',(80.6367476654038,112.332993858895,53.0201225356658));
#38316=CARTESIAN_POINT('',(80.6314498948689,423.667006141107,53.0228109606222));
#38317=CARTESIAN_POINT('Ctrl Pts',(80.6411686659135,113.667006141107,53.0214655157299));
#38318=CARTESIAN_POINT('Ctrl Pts',(80.6381590892165,113.458410213836,54.8626429328173));
#38319=CARTESIAN_POINT('Ctrl Pts',(78.6510709869002,113.037658277013,58.5856119621277));
#38320=CARTESIAN_POINT('Ctrl Pts',(73.3819666201983,112.510828335414,59.0388557003805));
#38321=CARTESIAN_POINT('Ctrl Pts',(70.3494075285618,112.086516316309,56.6151203100856));
#38322=CARTESIAN_POINT('Ctrl Pts',(68.7614344313501,111.662204297205,53.0726283441146));
#38323=CARTESIAN_POINT('Ctrl Pts',(70.5303630449218,111.131814273324,48.0507699139827));
#38324=CARTESIAN_POINT('Ctrl Pts',(76.7695181841129,110.495346244667,46.587732736418));
#38325=CARTESIAN_POINT('Ctrl Pts',(80.290773265235,110.007076867261,50.0049409544789));
#38326=CARTESIAN_POINT('Ctrl Pts',(80.6317633641979,109.730963499408,52.4503541218443));
#38327=CARTESIAN_POINT('Ctrl Pts',(80.627375492094,109.667006141107,53.018034188696));
#38328=CARTESIAN_POINT('Ctrl Pts',(80.6367476654038,112.332993858895,53.0201225356658));
#38329=CARTESIAN_POINT('Ctrl Pts',(80.6253734967643,112.136376024548,54.7573615278239));
#38330=CARTESIAN_POINT('Ctrl Pts',(78.8479097578291,111.727602180649,58.3813275115759));
#38331=CARTESIAN_POINT('Ctrl Pts',(72.6610927960897,111.106672327199,59.2814013261173));
#38332=CARTESIAN_POINT('Ctrl Pts',(68.4699764911283,110.470204298542,54.4497921162674));
#38333=CARTESIAN_POINT('Ctrl Pts',(70.2588968349819,109.833736269885,48.3089723467443));
#38334=CARTESIAN_POINT('Ctrl Pts',(76.4059152161931,109.197268241228,46.4974261411829));
#38335=CARTESIAN_POINT('Ctrl Pts',(80.1971179225261,108.697020770898,49.7905105458927));
#38336=CARTESIAN_POINT('Ctrl Pts',(80.6314803485583,108.40892931012,52.3454205783677));
#38337=CARTESIAN_POINT('Ctrl Pts',(80.6285061370469,108.332993858894,53.0199845307063));
#38338=CARTESIAN_POINT('Origin',(74.9879498948689,423.667006141107,53.0228109606356));
#38339=CARTESIAN_POINT('',(80.6297280373482,117.667006141107,53.029522769627));
#38340=CARTESIAN_POINT('',(80.63273293575,116.332993858895,53.0278590605154));
#38341=CARTESIAN_POINT('',(80.6314498948689,423.667006141107,53.0228109606222));
#38342=CARTESIAN_POINT('Ctrl Pts',(80.6297280373482,117.667006141107,53.029522769627));
#38343=CARTESIAN_POINT('Ctrl Pts',(80.6342201504912,117.610168947369,53.5338174939984));
#38344=CARTESIAN_POINT('Ctrl Pts',(80.3409432296834,117.341175744079,55.9145507214586));
#38345=CARTESIAN_POINT('Ctrl Pts',(77.7203244431643,116.966104536013,58.6179969197401));
#38346=CARTESIAN_POINT('Ctrl Pts',(73.841439580255,116.541792516908,58.7766162966422));
#38347=CARTESIAN_POINT('Ctrl Pts',(70.3196135975197,116.117480497803,57.1433221915374));
#38348=CARTESIAN_POINT('Ctrl Pts',(68.3621779488011,115.587090473922,52.1918965167118));
#38349=CARTESIAN_POINT('Ctrl Pts',(72.1133696732489,114.950622445266,46.9961198394222));
#38350=CARTESIAN_POINT('Ctrl Pts',(78.4996923124141,114.314154416609,47.3493712893946));
#38351=CARTESIAN_POINT('Ctrl Pts',(80.6269983281491,113.886282315223,51.0860990420978));
#38352=CARTESIAN_POINT('Ctrl Pts',(80.6412200300068,113.670566223389,52.9900423562021));
#38353=CARTESIAN_POINT('Ctrl Pts',(80.6411686659135,113.667006141107,53.0214655157299));
#38354=CARTESIAN_POINT('Ctrl Pts',(80.63273293575,116.332993858895,53.0278590605154));
#38355=CARTESIAN_POINT('Ctrl Pts',(80.6367547024567,116.288134758081,53.4247644365811));
#38356=CARTESIAN_POINT('Ctrl Pts',(80.4185607171579,116.031119647715,55.695001895594));
#38357=CARTESIAN_POINT('Ctrl Pts',(77.3351104931415,115.561948527797,59.2738152357066));
#38358=CARTESIAN_POINT('Ctrl Pts',(71.002608172017,114.92548049914,58.3741943203373));
#38359=CARTESIAN_POINT('Ctrl Pts',(68.326532179209,114.289012470483,52.5648466186468));
#38360=CARTESIAN_POINT('Ctrl Pts',(71.7796338362221,113.652544441826,47.1663631667719));
#38361=CARTESIAN_POINT('Ctrl Pts',(77.1039338323076,113.122154417946,47.1666527860612));
#38362=CARTESIAN_POINT('Ctrl Pts',(79.9174693977396,112.697842398841,49.8415220367884));
#38363=CARTESIAN_POINT('Ctrl Pts',(80.6034465893773,112.470148214083,51.8085666155929));
#38364=CARTESIAN_POINT('Ctrl Pts',(80.6376465351616,112.348532034101,52.8828332408032));
#38365=CARTESIAN_POINT('Ctrl Pts',(80.6367476654038,112.332993858895,53.0201225356658));
#38366=CARTESIAN_POINT('Origin',(74.9879498948689,423.667006141107,53.0228109606356));
#38367=CARTESIAN_POINT('',(80.621118997799,121.667006141107,53.0201440891292));
#38368=CARTESIAN_POINT('',(80.6220356038237,120.332993858894,53.0220685349663));
#38369=CARTESIAN_POINT('',(80.6314498948689,423.667006141107,53.0228109606222));
#38370=CARTESIAN_POINT('Ctrl Pts',(80.621118997799,121.667006141107,53.0201440891292));
#38371=CARTESIAN_POINT('Ctrl Pts',(80.6173308858264,121.54977167135,54.0624647895258));
#38372=CARTESIAN_POINT('Ctrl Pts',(80.0879360230795,121.326459196816,56.0512552874316));
#38373=CARTESIAN_POINT('Ctrl Pts',(77.8952676648289,120.997068717506,58.1187176641229));
#38374=CARTESIAN_POINT('Ctrl Pts',(74.1653018934157,120.572756698402,59.1949440485428));
#38375=CARTESIAN_POINT('Ctrl Pts',(69.4406556577397,120.042366674521,56.7401755299422));
#38376=CARTESIAN_POINT('Ctrl Pts',(68.8657804610841,119.405898645864,50.3576170192741));
#38377=CARTESIAN_POINT('Ctrl Pts',(73.9190741955237,118.769430617207,46.4366317002641));
#38378=CARTESIAN_POINT('Ctrl Pts',(79.4141901927945,118.189799782288,48.3687963867855));
#38379=CARTESIAN_POINT('Ctrl Pts',(80.6174524542663,117.822324956922,51.6514382045845));
#38380=CARTESIAN_POINT('Ctrl Pts',(80.6297280373482,117.667006141107,53.029522769627));
#38381=CARTESIAN_POINT('Ctrl Pts',(80.6220356038237,120.332993858894,53.0220685349662));
#38382=CARTESIAN_POINT('Ctrl Pts',(80.6222590142985,120.227737482062,53.9594345098134));
#38383=CARTESIAN_POINT('Ctrl Pts',(79.9569189659327,119.910325095676,56.7865524380521));
#38384=CARTESIAN_POINT('Ctrl Pts',(75.4880780795087,119.380756699739,59.6763907722353));
#38385=CARTESIAN_POINT('Ctrl Pts',(69.6582969414783,118.744288671082,57.0451258062755));
#38386=CARTESIAN_POINT('Ctrl Pts',(68.7254440554294,118.107820642425,50.7049901510374));
#38387=CARTESIAN_POINT('Ctrl Pts',(72.7454665815478,117.577430618544,47.2139173328772));
#38388=CARTESIAN_POINT('Ctrl Pts',(76.6236647050234,117.153118599439,47.3885231790242));
#38389=CARTESIAN_POINT('Ctrl Pts',(79.6362958357505,116.773665681149,49.1138518710274));
#38390=CARTESIAN_POINT('Ctrl Pts',(80.6177342147434,116.500290767633,51.5476456528997));
#38391=CARTESIAN_POINT('Ctrl Pts',(80.63273293575,116.332993858895,53.0278590605154));
#38392=CARTESIAN_POINT('Origin',(74.9879498948689,423.667006141107,53.0228109606356));
#38393=CARTESIAN_POINT('',(80.6357111684385,125.667006141107,53.0197150307418));
#38394=CARTESIAN_POINT('',(80.6328519299148,124.332993858894,53.0182731545141));
#38395=CARTESIAN_POINT('',(80.6314498948689,423.667006141107,53.0228109606222));
#38396=CARTESIAN_POINT('Ctrl Pts',(80.6357111684385,125.667006141107,53.0197150307418));
#38397=CARTESIAN_POINT('Ctrl Pts',(80.6319016651264,125.595452400107,53.652965053311));
#38398=CARTESIAN_POINT('Ctrl Pts',(80.3527813722094,125.41782065433,55.2289179960977));
#38399=CARTESIAN_POINT('Ctrl Pts',(78.414091999895,125.028032899,58.2221885065829));
#38400=CARTESIAN_POINT('Ctrl Pts',(73.2373364704086,124.49764287512,59.4669265192302));
#38401=CARTESIAN_POINT('Ctrl Pts',(68.6180861968185,123.861174846463,55.0250731286094));
#38402=CARTESIAN_POINT('Ctrl Pts',(69.8622107451905,123.224706817806,48.7511542937376));
#38403=CARTESIAN_POINT('Ctrl Pts',(75.8090405776548,122.588238789149,46.3963467894746));
#38404=CARTESIAN_POINT('Ctrl Pts',(80.0527232061874,122.069005230249,49.4497267074848));
#38405=CARTESIAN_POINT('Ctrl Pts',(80.6241861283289,121.761927680902,52.1762055610979));
#38406=CARTESIAN_POINT('Ctrl Pts',(80.621118997799,121.667006141107,53.0201440891292));
#38407=CARTESIAN_POINT('Ctrl Pts',(80.6328519299148,124.332993858894,53.0182731545141));
#38408=CARTESIAN_POINT('Ctrl Pts',(80.6189547166767,124.167340206042,54.4855436430345));
#38409=CARTESIAN_POINT('Ctrl Pts',(79.2808346715744,123.789530543638,57.852453412815));
#38410=CARTESIAN_POINT('Ctrl Pts',(73.6016194435095,123.19956487168,59.5544497443309));
#38411=CARTESIAN_POINT('Ctrl Pts',(68.7399147931205,122.563096843024,55.3793614187719));
#38412=CARTESIAN_POINT('Ctrl Pts',(69.4858278482179,122.032706819143,50.107570048997));
#38413=CARTESIAN_POINT('Ctrl Pts',(72.5283512255512,121.608394800038,47.6963547154323));
#38414=CARTESIAN_POINT('Ctrl Pts',(76.33686993267,121.184082780934,46.9439630993421));
#38415=CARTESIAN_POINT('Ctrl Pts',(79.9412181579135,120.758949133886,49.2290963001954));
#38416=CARTESIAN_POINT('Ctrl Pts',(80.6218087054788,120.439893491614,52.0700684619069));
#38417=CARTESIAN_POINT('Ctrl Pts',(80.6220356038237,120.332993858894,53.0220685349662));
#38418=CARTESIAN_POINT('Origin',(74.9879498948689,423.667006141107,53.0228109606356));
#38419=CARTESIAN_POINT('',(80.6371028432593,129.667006141107,53.0252254998433));
#38420=CARTESIAN_POINT('',(80.6389896620935,128.332993858894,53.0249895228329));
#38421=CARTESIAN_POINT('',(80.6314498948689,423.667006141107,53.0228109606222));
#38422=CARTESIAN_POINT('Ctrl Pts',(80.6371028432593,129.667006141107,53.0252254998433));
#38423=CARTESIAN_POINT('Ctrl Pts',(80.6382524187439,129.641133128863,53.2540168026428));
#38424=CARTESIAN_POINT('Ctrl Pts',(80.5164513696564,129.403104107067,55.3571413879679));
#38425=CARTESIAN_POINT('Ctrl Pts',(77.8918269900061,128.952919075718,59.0360272806059));
#38426=CARTESIAN_POINT('Ctrl Pts',(71.4916583615966,128.316451047061,58.7114103344188));
#38427=CARTESIAN_POINT('Ctrl Pts',(68.3169862074485,127.679983018404,53.1588109294466));
#38428=CARTESIAN_POINT('Ctrl Pts',(71.2627145002853,127.043514989747,47.4814358085654));
#38429=CARTESIAN_POINT('Ctrl Pts',(77.644334875132,126.40704696109,46.8962383844676));
#38430=CARTESIAN_POINT('Ctrl Pts',(80.469995123209,125.94821067821,50.5336793739854));
#38431=CARTESIAN_POINT('Ctrl Pts',(80.6375492316251,125.701530404883,52.7141755787275));
#38432=CARTESIAN_POINT('Ctrl Pts',(80.6357111684385,125.667006141107,53.0197150307418));
#38433=CARTESIAN_POINT('Ctrl Pts',(80.6389896620935,128.332993858894,53.0249895228329));
#38434=CARTESIAN_POINT('Ctrl Pts',(80.6395867975546,128.319098939575,53.1476577057808));
#38435=CARTESIAN_POINT('Ctrl Pts',(80.5801191447157,128.093048010703,55.1427011305502));
#38436=CARTESIAN_POINT('Ctrl Pts',(78.2242510960193,127.654841072279,58.8632366177664));
#38437=CARTESIAN_POINT('Ctrl Pts',(71.8159553123667,127.018373043623,58.8990106732897));
#38438=CARTESIAN_POINT('Ctrl Pts',(68.9222576097237,126.487983019741,54.4297060139589));
#38439=CARTESIAN_POINT('Ctrl Pts',(69.6382539201413,126.063671000637,50.6141775879205));
#38440=CARTESIAN_POINT('Ctrl Pts',(72.0203115207733,125.639358981532,47.5487723172087));
#38441=CARTESIAN_POINT('Ctrl Pts',(77.2847411767612,125.108968957652,46.7525619622429));
#38442=CARTESIAN_POINT('Ctrl Pts',(80.4073730821569,124.638154581847,50.3192597336851));
#38443=CARTESIAN_POINT('Ctrl Pts',(80.636753160923,124.379496215594,52.6063804225535));
#38444=CARTESIAN_POINT('Ctrl Pts',(80.6328519299148,124.332993858894,53.0182731545141));
#38445=CARTESIAN_POINT('Origin',(74.9879498948689,423.667006141107,53.0228109606356));
#38446=CARTESIAN_POINT('',(80.6223069729932,133.667006141107,53.0265007246441));
#38447=CARTESIAN_POINT('',(80.6314498948689,132.332993858894,53.0228109606253));
#38448=CARTESIAN_POINT('',(80.6314498948689,423.667006141107,53.0228109606222));
#38449=CARTESIAN_POINT('Ctrl Pts',(80.6223069729932,133.667006141107,53.0265007246441));
#38450=CARTESIAN_POINT('Ctrl Pts',(80.6265294801301,133.580735852844,53.7931407639138));
#38451=CARTESIAN_POINT('Ctrl Pts',(80.1255680059032,133.282309555028,56.4402161564905));
#38452=CARTESIAN_POINT('Ctrl Pts',(76.0784316098281,132.77172724766,59.6103041826723));
#38453=CARTESIAN_POINT('Ctrl Pts',(70.0405686636907,132.135259219003,57.4998268712375));
#38454=CARTESIAN_POINT('Ctrl Pts',(68.5417731922881,131.498791190346,51.2818275488413));
#38455=CARTESIAN_POINT('Ctrl Pts',(72.9761497214014,130.862323161689,46.6553991821764));
#38456=CARTESIAN_POINT('Ctrl Pts',(78.1993353737933,130.331933137808,47.6881151028675));
#38457=CARTESIAN_POINT('Ctrl Pts',(80.30411061963,129.933494130948,50.6645098309892));
#38458=CARTESIAN_POINT('Ctrl Pts',(80.6335392190362,129.747211133639,52.3159843585587));
#38459=CARTESIAN_POINT('Ctrl Pts',(80.6371028432593,129.667006141107,53.0252254998433));
#38460=CARTESIAN_POINT('Ctrl Pts',(80.6259063365819,132.332993858894,53.0265080521389));
#38461=CARTESIAN_POINT('Ctrl Pts',(80.6305336094359,132.258701663556,53.6865164641486));
#38462=CARTESIAN_POINT('Ctrl Pts',(80.2181584724033,131.972253458664,56.2262411860581));
#38463=CARTESIAN_POINT('Ctrl Pts',(76.4462897180739,131.473649244221,59.5392914259234));
#38464=CARTESIAN_POINT('Ctrl Pts',(71.3309082217835,130.94325922034,58.0624560662408));
#38465=CARTESIAN_POINT('Ctrl Pts',(69.3695355394668,130.518947201236,54.7122433733663));
#38466=CARTESIAN_POINT('Ctrl Pts',(69.1579113875603,130.094635182131,50.8358890158844));
#38467=CARTESIAN_POINT('Ctrl Pts',(72.6104447936233,129.56424515825,46.7827194398347));
#38468=CARTESIAN_POINT('Ctrl Pts',(78.8205962231645,128.941672048912,47.6359557426244));
#38469=CARTESIAN_POINT('Ctrl Pts',(80.6304693731441,128.531254949127,51.2746858953672));
#38470=CARTESIAN_POINT('Ctrl Pts',(80.6389896620935,128.332993858894,53.0249895228329));
#38471=CARTESIAN_POINT('Origin',(74.9879498948689,423.667006141107,53.0228109606356));
#38472=CARTESIAN_POINT('',(80.6275033360921,137.667006141107,53.0165438204127));
#38473=CARTESIAN_POINT('',(80.6314498948689,136.332993858894,53.0228109606257));
#38474=CARTESIAN_POINT('',(80.6314498948689,423.667006141107,53.0228109606222));
#38475=CARTESIAN_POINT('Ctrl Pts',(80.6275033360921,137.667006141107,53.0165438204127));
#38476=CARTESIAN_POINT('Ctrl Pts',(80.6170493129659,137.520338576824,54.3192593131434));
#38477=CARTESIAN_POINT('Ctrl Pts',(79.5194214481417,137.161515002989,57.5247164620686));
#38478=CARTESIAN_POINT('Ctrl Pts',(74.1883937223739,136.590535419602,59.6470816704889));
#38479=CARTESIAN_POINT('Ctrl Pts',(68.9794920835046,135.954067390944,55.9353102396218));
#38480=CARTESIAN_POINT('Ctrl Pts',(69.2937571436266,135.317599362288,49.534624955543));
#38481=CARTESIAN_POINT('Ctrl Pts',(73.9144292228386,134.787209338407,46.8893347883613));
#38482=CARTESIAN_POINT('Ctrl Pts',(77.6851592684559,134.362897319302,47.8126455754286));
#38483=CARTESIAN_POINT('Ctrl Pts',(80.0200232668462,134.024855588461,49.8409324552161));
#38484=CARTESIAN_POINT('Ctrl Pts',(80.6161454848692,133.792891862396,51.9078185426905));
#38485=CARTESIAN_POINT('Ctrl Pts',(80.6223069729932,133.667006141107,53.0265007246441));
#38486=CARTESIAN_POINT('Ctrl Pts',(80.6314498948689,136.332993858894,53.0228109606257));
#38487=CARTESIAN_POINT('Ctrl Pts',(80.6314498948719,136.140209036292,54.7318077489449));
#38488=CARTESIAN_POINT('Ctrl Pts',(79.8060659192693,135.94742421369,56.4221521097263));
#38489=CARTESIAN_POINT('Ctrl Pts',(78.4584055093439,135.754639391087,57.4730952299782));
#38490=CARTESIAN_POINT('Ctrl Pts',(77.1107450994185,135.561854568485,58.5240383502302));
#38491=CARTESIAN_POINT('Ctrl Pts',(75.2702256751625,135.369069745882,58.9126397065623));
#38492=CARTESIAN_POINT('Ctrl Pts',(73.6127451627042,135.17628492328,58.4961923829952));
#38493=CARTESIAN_POINT('Ctrl Pts',(71.9552646502458,134.983500100678,58.0797450594281));
#38494=CARTESIAN_POINT('Ctrl Pts',(70.5170033810729,134.790715278075,56.8673394809174));
#38495=CARTESIAN_POINT('Ctrl Pts',(69.8261371496123,134.597930455473,55.3042099684609));
#38496=CARTESIAN_POINT('Ctrl Pts',(69.1352709181517,134.40514563287,53.7410804560043));
#38497=CARTESIAN_POINT('Ctrl Pts',(69.2068803054901,134.212360810268,51.8613477992545));
#38498=CARTESIAN_POINT('Ctrl Pts',(70.0146680415444,134.019575987666,50.3553102844608));
#38499=CARTESIAN_POINT('Ctrl Pts',(70.8224557775985,133.826791165063,48.8492727696672));
#38500=CARTESIAN_POINT('Ctrl Pts',(72.3487890589403,133.634006342461,47.7498049531873));
#38501=CARTESIAN_POINT('Ctrl Pts',(74.0331492157619,133.441221519858,47.460666777573));
#38502=CARTESIAN_POINT('Ctrl Pts',(75.7175093725834,133.248436697256,47.1715286019588));
#38503=CARTESIAN_POINT('Ctrl Pts',(77.523129330786,133.055651874653,47.6990315230379));
#38504=CARTESIAN_POINT('Ctrl Pts',(78.7869273705894,132.862867052051,48.8494595029977));
#38505=CARTESIAN_POINT('Ctrl Pts',(79.9447859852113,132.686242654332,49.9034514424897));
#38506=CARTESIAN_POINT('Ctrl Pts',(80.631449894866,132.509618256613,51.4570729301846));
#38507=CARTESIAN_POINT('Ctrl Pts',(80.6314498948689,132.332993858894,53.0228109606253));
#38508=CARTESIAN_POINT('Origin',(74.9879498948689,423.667006141107,53.0228109606356));
#38509=CARTESIAN_POINT('',(80.6411518234535,141.667006141107,53.0227491827673));
#38510=CARTESIAN_POINT('',(80.6397210784657,140.332993858894,53.0209782018833));
#38511=CARTESIAN_POINT('',(80.6314498948689,423.667006141107,53.0228109606222));
#38512=CARTESIAN_POINT('Ctrl Pts',(80.6411518234535,141.667006141107,53.0227491827673));
#38513=CARTESIAN_POINT('Ctrl Pts',(80.6375409305296,141.459941300805,54.8502991094422));
#38514=CARTESIAN_POINT('Ctrl Pts',(79.6692138860864,141.252876460503,56.679321513607));
#38515=CARTESIAN_POINT('Ctrl Pts',(78.1561081471227,141.0458116202,57.7034820184246));
#38516=CARTESIAN_POINT('Ctrl Pts',(76.6057991949101,140.833655610648,58.7528238841218));
#38517=CARTESIAN_POINT('Ctrl Pts',(74.4835929147854,140.621499601096,58.9572384899893));
#38518=CARTESIAN_POINT('Ctrl Pts',(72.7625167868681,140.409343591543,58.2196836204947));
#38519=CARTESIAN_POINT('Ctrl Pts',(71.0414406589509,140.197187581991,57.4821287510002));
#38520=CARTESIAN_POINT('Ctrl Pts',(69.7214946832408,139.985031572439,55.8026044061438));
#38521=CARTESIAN_POINT('Ctrl Pts',(69.4123227137353,139.772875562886,53.9574241779733));
#38522=CARTESIAN_POINT('Ctrl Pts',(69.1031507442298,139.560719553334,52.1122439498026));
#38523=CARTESIAN_POINT('Ctrl Pts',(69.8047527809292,139.348563543782,50.1014078383178));
#38524=CARTESIAN_POINT('Ctrl Pts',(71.1893974253191,139.136407534229,48.839304051185));
#38525=CARTESIAN_POINT('Ctrl Pts',(71.8817197475139,139.030329529453,48.2082521576187));
#38526=CARTESIAN_POINT('Ctrl Pts',(72.7448027216314,138.924251524677,47.7643833451403));
#38527=CARTESIAN_POINT('Ctrl Pts',(73.6616100464181,138.818173519901,47.5424985339224));
#38528=CARTESIAN_POINT('Ctrl Pts',(74.5784173712049,138.712095515125,47.3206137227045));
#38529=CARTESIAN_POINT('Ctrl Pts',(75.5489490466608,138.606017510349,47.3207129127471));
#38530=CARTESIAN_POINT('Ctrl Pts',(76.4532076287885,138.499939505572,47.5653618588544));
#38531=CARTESIAN_POINT('Ctrl Pts',(78.2617247930437,138.28778349602,48.0546597510688));
#38532=CARTESIAN_POINT('Ctrl Pts',(79.8051495839855,138.075627486468,49.522156667542));
#38533=CARTESIAN_POINT('Ctrl Pts',(80.3739101054989,137.863471476916,51.3045115284849));
#38534=CARTESIAN_POINT('Ctrl Pts',(80.5494754470752,137.797983031646,51.8546899043311));
#38535=CARTESIAN_POINT('Ctrl Pts',(80.6321711556246,137.732494586377,52.4348691150039));
#38536=CARTESIAN_POINT('Ctrl Pts',(80.6275033360921,137.667006141107,53.0165438204127));
#38537=CARTESIAN_POINT('Ctrl Pts',(80.6397210784657,140.332993858894,53.0209782018833));
#38538=CARTESIAN_POINT('Ctrl Pts',(80.6287643883681,140.137907111517,54.7421720158137));
#38539=CARTESIAN_POINT('Ctrl Pts',(79.321297971357,139.836742359363,57.4088279887623));
#38540=CARTESIAN_POINT('Ctrl Pts',(75.8739191842768,139.429499602433,58.8224506187867));
#38541=CARTESIAN_POINT('Ctrl Pts',(72.0061278849508,139.005187583328,58.4891364257266));
#38542=CARTESIAN_POINT('Ctrl Pts',(68.476400198112,138.474797559447,54.5030113663535));
#38543=CARTESIAN_POINT('Ctrl Pts',(70.2291765021866,137.83832953079,48.3389777955731));
#38544=CARTESIAN_POINT('Ctrl Pts',(76.3526370626844,137.201861502133,46.4915108263287));
#38545=CARTESIAN_POINT('Ctrl Pts',(80.1931527706955,136.700082944835,49.7591848231774));
#38546=CARTESIAN_POINT('Ctrl Pts',(80.6290640066136,136.410460397088,52.3302465850105));
#38547=CARTESIAN_POINT('Ctrl Pts',(80.6247374915432,136.332993858894,53.019329840359));
#38548=CARTESIAN_POINT('Origin',(74.9879498948689,423.667006141107,53.0228109606356));
#38549=CARTESIAN_POINT('',(80.629461543256,145.667006141107,53.0278924515447));
#38550=CARTESIAN_POINT('',(80.6299737020758,144.332993858894,53.0273121532265));
#38551=CARTESIAN_POINT('',(80.6314498948689,423.667006141107,53.0228109606222));
#38552=CARTESIAN_POINT('Ctrl Pts',(80.629461543256,145.667006141107,53.0278924515447));
#38553=CARTESIAN_POINT('Ctrl Pts',(80.633661519085,145.611700034338,53.5183154898172));
#38554=CARTESIAN_POINT('Ctrl Pts',(80.5749012622352,145.556393927568,54.0077190168699));
#38555=CARTESIAN_POINT('Ctrl Pts',(80.4491472122468,145.501087820799,54.4792559898802));
#38556=CARTESIAN_POINT('Ctrl Pts',(79.9667506200988,145.288931811246,56.288087028507));
#38557=CARTESIAN_POINT('Ctrl Pts',(78.4985307500936,145.076775801694,57.8340091610261));
#38558=CARTESIAN_POINT('Ctrl Pts',(76.7154875349777,144.864619792142,58.4057146067159));
#38559=CARTESIAN_POINT('Ctrl Pts',(74.9324443198619,144.65246378259,58.9774200524057));
#38560=CARTESIAN_POINT('Ctrl Pts',(72.8345777596355,144.440307773037,58.5749088112661));
#38561=CARTESIAN_POINT('Ctrl Pts',(71.3912177720621,144.228151763485,57.3845352029265));
#38562=CARTESIAN_POINT('Ctrl Pts',(69.9478577844887,144.015995753933,56.1941615945869));
#38563=CARTESIAN_POINT('Ctrl Pts',(69.1590043695682,143.80383974438,54.2159256190472));
#38564=CARTESIAN_POINT('Ctrl Pts',(69.3768109363074,143.591683734828,52.3550905752519));
#38565=CARTESIAN_POINT('Ctrl Pts',(69.485714219677,143.485605730052,51.4246730533542));
#38566=CARTESIAN_POINT('Ctrl Pts',(69.8462824984615,143.379527725276,50.5236057643925));
#38567=CARTESIAN_POINT('Ctrl Pts',(70.3929736009116,143.2734497205,49.7549072677544));
#38568=CARTESIAN_POINT('Ctrl Pts',(70.9396647033619,143.167371715723,48.9862087711162));
#38569=CARTESIAN_POINT('Ctrl Pts',(71.6724786294777,143.061293710947,48.3498790668017));
#38570=CARTESIAN_POINT('Ctrl Pts',(72.5156146144877,142.955215706171,47.9416408998399));
#38571=CARTESIAN_POINT('Ctrl Pts',(74.2018865845076,142.743059696619,47.1251645659165));
#38572=CARTESIAN_POINT('Ctrl Pts',(76.329446790104,142.530903687066,47.2210543814042));
#38573=CARTESIAN_POINT('Ctrl Pts',(77.9275991182749,142.318747677514,48.1937755732785));
#38574=CARTESIAN_POINT('Ctrl Pts',(79.5257514464457,142.106591667962,49.1664967651527));
#38575=CARTESIAN_POINT('Ctrl Pts',(80.5944958971913,141.894435658409,51.0160493334135));
#38576=CARTESIAN_POINT('Ctrl Pts',(80.6396623104136,141.682279648857,52.8879601803071));
#38577=CARTESIAN_POINT('Ctrl Pts',(80.6407461819222,141.677188479607,52.9328809674318));
#38578=CARTESIAN_POINT('Ctrl Pts',(80.6412406056292,141.672097310357,52.9778146300166));
#38579=CARTESIAN_POINT('Ctrl Pts',(80.6411518234535,141.667006141107,53.0227491827673));
#38580=CARTESIAN_POINT('Ctrl Pts',(80.6299737020758,144.332993858894,53.0273121532265));
#38581=CARTESIAN_POINT('Ctrl Pts',(80.6335616117796,144.28966584505,53.4111490723472));
#38582=CARTESIAN_POINT('Ctrl Pts',(80.5111600798701,144.140259826428,54.7328567481776));
#38583=CARTESIAN_POINT('Ctrl Pts',(79.4598393053229,143.884775803031,56.8205690949624));
#38584=CARTESIAN_POINT('Ctrl Pts',(76.3211035792066,143.460463783927,59.1051359965959));
#38585=CARTESIAN_POINT('Ctrl Pts',(71.0423553953876,142.930073760046,58.4101625121945));
#38586=CARTESIAN_POINT('Ctrl Pts',(68.3237688121462,142.293605731389,52.6069891024768));
#38587=CARTESIAN_POINT('Ctrl Pts',(71.7355301328902,141.657137702732,47.1968330854384));
#38588=CARTESIAN_POINT('Ctrl Pts',(78.131284816172,141.020669674075,47.1318294725001));
#38589=CARTESIAN_POINT('Ctrl Pts',(80.567608711688,140.579288392796,50.8486300315097));
#38590=CARTESIAN_POINT('Ctrl Pts',(80.6406797423337,140.350063121069,52.870381050318));
#38591=CARTESIAN_POINT('Ctrl Pts',(80.6397210784657,140.332993858894,53.0209782018833));
#38592=CARTESIAN_POINT('Origin',(74.9879498948689,423.667006141107,53.0228109606356));
#38593=CARTESIAN_POINT('',(80.6225096147018,149.667006141107,53.0213500647842));
#38594=CARTESIAN_POINT('',(80.6264905426344,148.332993858894,53.023059952509));
#38595=CARTESIAN_POINT('',(80.6314498948689,423.667006141107,53.0228109606222));
#38596=CARTESIAN_POINT('Ctrl Pts',(80.6225096147018,149.667006141107,53.0213500647842));
#38597=CARTESIAN_POINT('Ctrl Pts',(80.6207021386803,149.551302758318,54.0506438715325));
#38598=CARTESIAN_POINT('Ctrl Pts',(79.8583912421759,149.223443365977,56.970430727468));
#38599=CARTESIAN_POINT('Ctrl Pts',(75.1550028210449,148.683427964083,59.698390786709));
#38600=CARTESIAN_POINT('Ctrl Pts',(70.4230863720779,148.153037940203,57.2576660475808));
#38601=CARTESIAN_POINT('Ctrl Pts',(69.1485793584295,147.728725921098,53.5907136673885));
#38602=CARTESIAN_POINT('Ctrl Pts',(69.6926334846929,147.304413901994,49.7468987662606));
#38603=CARTESIAN_POINT('Ctrl Pts',(73.8655835469356,146.774023878113,46.4401392784498));
#38604=CARTESIAN_POINT('Ctrl Pts',(79.3981822703055,146.192861956225,48.3456113603836));
#38605=CARTESIAN_POINT('Ctrl Pts',(80.6175502763282,145.82385604389,51.6370368956453));
#38606=CARTESIAN_POINT('Ctrl Pts',(80.629461543256,145.667006141107,53.0278924515447));
#38607=CARTESIAN_POINT('Ctrl Pts',(80.6264905426344,148.332993858894,53.023059952509));
#38608=CARTESIAN_POINT('Ctrl Pts',(80.6268129881547,148.22926856903,53.9454088413081));
#38609=CARTESIAN_POINT('Ctrl Pts',(79.9631268520014,147.913387269614,56.7537913392259));
#38610=CARTESIAN_POINT('Ctrl Pts',(75.5416724725442,147.385349960645,59.6774833042897));
#38611=CARTESIAN_POINT('Ctrl Pts',(69.6838446044191,146.748881931988,57.0787552882691));
#38612=CARTESIAN_POINT('Ctrl Pts',(68.712125846895,146.112413903331,50.7569148841861));
#38613=CARTESIAN_POINT('Ctrl Pts',(73.4982792811873,145.475945874674,46.5139632297563));
#38614=CARTESIAN_POINT('Ctrl Pts',(79.2453262741431,144.882805859862,48.1381250442711));
#38615=CARTESIAN_POINT('Ctrl Pts',(80.6159933796395,144.501821854602,51.5316881450347));
#38616=CARTESIAN_POINT('Ctrl Pts',(80.6299737020758,144.332993858894,53.0273121532265));
#38617=CARTESIAN_POINT('Origin',(74.9879498948689,423.667006141107,53.0228109606356));
#38618=CARTESIAN_POINT('',(80.6352064155011,153.667006141107,53.0176672101712));
#38619=CARTESIAN_POINT('',(80.6287116038918,152.332993858894,53.0183048799968));
#38620=CARTESIAN_POINT('',(80.6314498948689,423.667006141107,53.0228109606222));
#38621=CARTESIAN_POINT('Ctrl Pts',(80.6352064155011,153.667006141107,53.0176672101712));
#38622=CARTESIAN_POINT('Ctrl Pts',(80.6209020684031,153.490905482299,54.5766293472566));
#38623=CARTESIAN_POINT('Ctrl Pts',(79.1397801677944,153.102648813938,58.0389759024666));
#38624=CARTESIAN_POINT('Ctrl Pts',(74.3184020126598,152.608314140801,59.2134233877355));
#38625=CARTESIAN_POINT('Ctrl Pts',(70.9516299530984,152.184002121697,57.2806135715887));
#38626=CARTESIAN_POINT('Ctrl Pts',(68.8418931422078,151.759690102592,54.0217919325278));
#38627=CARTESIAN_POINT('Ctrl Pts',(69.8241254614745,151.229300078712,48.7888778110099));
#38628=CARTESIAN_POINT('Ctrl Pts',(75.7671119106681,150.592832050054,46.3912859569748));
#38629=CARTESIAN_POINT('Ctrl Pts',(80.0346917712683,150.072067404186,49.4204165109013));
#38630=CARTESIAN_POINT('Ctrl Pts',(80.624016362438,149.763458767871,52.1633104035476));
#38631=CARTESIAN_POINT('Ctrl Pts',(80.6225096147018,149.667006141107,53.0213500647842));
#38632=CARTESIAN_POINT('Ctrl Pts',(80.6287116038918,152.332993858894,53.0183048799968));
#38633=CARTESIAN_POINT('Ctrl Pts',(80.615318583347,152.168871293011,54.4729876890807));
#38634=CARTESIAN_POINT('Ctrl Pts',(79.307288013441,151.792592717575,57.8257938433298));
#38635=CARTESIAN_POINT('Ctrl Pts',(73.642959648389,151.204158132586,59.5630876029432));
#38636=CARTESIAN_POINT('Ctrl Pts',(68.7639080710162,150.567690103929,55.4272975763874));
#38637=CARTESIAN_POINT('Ctrl Pts',(69.5952201151085,149.931222075272,49.0854663169038));
#38638=CARTESIAN_POINT('Ctrl Pts',(75.3939889653761,149.294754046615,46.3574973920444));
#38639=CARTESIAN_POINT('Ctrl Pts',(79.8991646679696,148.764364022735,49.1950249110227));
#38640=CARTESIAN_POINT('Ctrl Pts',(80.620971065803,148.443777293494,52.0379444949594));
#38641=CARTESIAN_POINT('Ctrl Pts',(80.6264832288695,148.335346573806,53.0021390759566));
#38642=CARTESIAN_POINT('Ctrl Pts',(80.6264905426344,148.332993858894,53.023059952509));
#38643=CARTESIAN_POINT('Origin',(74.9879498948689,423.667006141107,53.0228109606356));
#38644=CARTESIAN_POINT('',(80.6383546037414,157.667006141107,53.0279836470809));
#38645=CARTESIAN_POINT('',(80.6404628146951,156.332993858894,53.0238399447972));
#38646=CARTESIAN_POINT('',(80.6314498948689,423.667006141107,53.0228109606222));
#38647=CARTESIAN_POINT('Ctrl Pts',(80.6383546037414,157.667006141107,53.0279836470809));
#38648=CARTESIAN_POINT('Ctrl Pts',(80.639943014158,157.642664215832,53.24303366321));
#38649=CARTESIAN_POINT('Ctrl Pts',(80.5307282685173,157.406166281004,55.3303178933253));
#38650=CARTESIAN_POINT('Ctrl Pts',(78.5417996070232,157.0635903414,58.135748356356));
#38651=CARTESIAN_POINT('Ctrl Pts',(74.7324983674773,156.639278322295,58.8841679932114));
#38652=CARTESIAN_POINT('Ctrl Pts',(71.002752658437,156.214966303191,57.8071792131713));
#38653=CARTESIAN_POINT('Ctrl Pts',(68.3129682762291,155.68457627931,53.2122656656242));
#38654=CARTESIAN_POINT('Ctrl Pts',(71.2277399375131,155.048108250653,47.5051086854453));
#38655=CARTESIAN_POINT('Ctrl Pts',(77.5932150058283,154.411640221996,46.8801042110002));
#38656=CARTESIAN_POINT('Ctrl Pts',(80.4685585989152,153.951272852148,50.504449189847));
#38657=CARTESIAN_POINT('Ctrl Pts',(80.6381351282911,153.703061491851,52.6984808594245));
#38658=CARTESIAN_POINT('Ctrl Pts',(80.6352064155011,153.667006141107,53.0176672101712));
#38659=CARTESIAN_POINT('Ctrl Pts',(80.6404628146951,156.332993858894,53.0238399447972));
#38660=CARTESIAN_POINT('Ctrl Pts',(80.641007859621,156.320630026543,53.1328929203889));
#38661=CARTESIAN_POINT('Ctrl Pts',(80.5893550289291,156.09611018464,55.1129350212325));
#38662=CARTESIAN_POINT('Ctrl Pts',(78.2611269268695,155.659434333185,58.8426502572334));
#38663=CARTESIAN_POINT('Ctrl Pts',(71.8655032454052,155.022966304528,58.9194692881673));
#38664=CARTESIAN_POINT('Ctrl Pts',(68.33462666264,154.386498275871,53.5862888115946));
#38665=CARTESIAN_POINT('Ctrl Pts',(70.9238769856076,153.750030247214,47.7242654920534));
#38666=CARTESIAN_POINT('Ctrl Pts',(76.1859185490112,153.219640223333,46.9124224547526));
#38667=CARTESIAN_POINT('Ctrl Pts',(79.3745360971544,152.795328204228,49.1268356994087));
#38668=CARTESIAN_POINT('Ctrl Pts',(80.4920978723783,152.535138751008,51.2287370500932));
#38669=CARTESIAN_POINT('Ctrl Pts',(80.632631314106,152.381027302563,52.5925655894274));
#38670=CARTESIAN_POINT('Ctrl Pts',(80.6287116038918,152.332993858894,53.0183048799968));
#38671=CARTESIAN_POINT('Origin',(74.9879498948689,423.667006141107,53.0228109606356));
#38672=CARTESIAN_POINT('',(80.6211904296695,161.667006141107,53.0245698560322));
#38673=CARTESIAN_POINT('',(80.6314498948689,160.332993858894,53.0228109606264));
#38674=CARTESIAN_POINT('',(80.6314498948689,423.667006141107,53.0228109606222));
#38675=CARTESIAN_POINT('Ctrl Pts',(80.6211904296695,161.667006141107,53.0245698560322));
#38676=CARTESIAN_POINT('Ctrl Pts',(80.6241319221786,161.582266939812,53.7779642526502));
#38677=CARTESIAN_POINT('Ctrl Pts',(80.307523847763,161.391449733741,55.4724725522702));
#38678=CARTESIAN_POINT('Ctrl Pts',(78.6385393623837,161.094554522894,57.6156269035887));
#38679=CARTESIAN_POINT('Ctrl Pts',(75.1163796021698,160.670242503789,59.2482011009735));
#38680=CARTESIAN_POINT('Ctrl Pts',(70.0725868922178,160.139852479909,57.5428197268428));
#38681=CARTESIAN_POINT('Ctrl Pts',(68.530890451871,159.503384451252,51.3226343019818));
#38682=CARTESIAN_POINT('Ctrl Pts',(72.9269747274227,158.866916422595,46.6767386422982));
#38683=CARTESIAN_POINT('Ctrl Pts',(78.9734922431205,158.254790319213,47.8081729292422));
#38684=CARTESIAN_POINT('Ctrl Pts',(80.6260989647779,157.854820225384,51.3687302644544));
#38685=CARTESIAN_POINT('Ctrl Pts',(80.6383546037414,157.667006141107,53.0279836470809));
#38686=CARTESIAN_POINT('Ctrl Pts',(80.6256611505083,160.332993858894,53.0268354269295));
#38687=CARTESIAN_POINT('Ctrl Pts',(80.6302503427949,160.260232750524,53.6737963609542));
#38688=CARTESIAN_POINT('Ctrl Pts',(80.2289081100368,159.975315632601,56.2016586546249));
#38689=CARTESIAN_POINT('Ctrl Pts',(76.4971135606888,159.478242505127,59.5222476700871));
#38690=CARTESIAN_POINT('Ctrl Pts',(70.334196289122,158.841774476469,57.8110042209413));
#38691=CARTESIAN_POINT('Ctrl Pts',(68.4451819243434,158.205306447813,51.6873485020516));
#38692=CARTESIAN_POINT('Ctrl Pts',(71.8856615424623,157.674916423932,47.6239422302756));
#38693=CARTESIAN_POINT('Ctrl Pts',(75.7451117847744,157.250604404827,47.2049533120979));
#38694=CARTESIAN_POINT('Ctrl Pts',(79.2631705587981,156.838656218073,48.5572394850874));
#38695=CARTESIAN_POINT('Ctrl Pts',(80.6316552128679,156.532786036096,51.26160872025));
#38696=CARTESIAN_POINT('Ctrl Pts',(80.6404628146951,156.332993858894,53.0238399447972));
#38697=CARTESIAN_POINT('Origin',(74.9879498948689,423.667006141107,53.0228109606356));
#38698=CARTESIAN_POINT('',(80.6298086662852,165.667006141107,53.0194647221037));
#38699=CARTESIAN_POINT('',(80.6314498948689,164.332993858894,53.0228109606266));
#38700=CARTESIAN_POINT('',(80.6314498948689,423.667006141107,53.0228109606222));
#38701=CARTESIAN_POINT('Ctrl Pts',(80.6298086662852,165.667006141107,53.0194647221037));
#38702=CARTESIAN_POINT('Ctrl Pts',(80.6279297615169,165.627947668569,53.3662095389731));
#38703=CARTESIAN_POINT('Ctrl Pts',(80.504839828438,165.482811191255,54.6560627762247));
#38704=CARTESIAN_POINT('Ctrl Pts',(79.1670753196014,165.125518704388,57.6387493563994));
#38705=CARTESIAN_POINT('Ctrl Pts',(74.2407590117034,164.595128680508,59.6585459220802));
#38706=CARTESIAN_POINT('Ctrl Pts',(68.9980337649973,163.95866065185,55.9732553471886));
#38707=CARTESIAN_POINT('Ctrl Pts',(69.2706230284558,163.322192623193,49.5829816025151));
#38708=CARTESIAN_POINT('Ctrl Pts',(74.7886807951738,162.685724594536,46.3486436607436));
#38709=CARTESIAN_POINT('Ctrl Pts',(79.7400684039384,162.133995767174,48.8673383718253));
#38710=CARTESIAN_POINT('Ctrl Pts',(80.6167674992983,161.794422949365,51.8917398563494));
#38711=CARTESIAN_POINT('Ctrl Pts',(80.6211904296695,161.667006141107,53.0245698560322));
#38712=CARTESIAN_POINT('Ctrl Pts',(80.6314498948689,164.332993858894,53.0228109606266));
#38713=CARTESIAN_POINT('Ctrl Pts',(80.6314498948716,164.140209036292,54.7318077489456));
#38714=CARTESIAN_POINT('Ctrl Pts',(79.8060659192689,163.94742421369,56.4221521097268));
#38715=CARTESIAN_POINT('Ctrl Pts',(78.4584055093435,163.754639391087,57.4730952299786));
#38716=CARTESIAN_POINT('Ctrl Pts',(77.1107450994181,163.561854568485,58.5240383502304));
#38717=CARTESIAN_POINT('Ctrl Pts',(75.2702256751622,163.369069745882,58.9126397065623));
#38718=CARTESIAN_POINT('Ctrl Pts',(73.612745162704,163.17628492328,58.4961923829952));
#38719=CARTESIAN_POINT('Ctrl Pts',(71.9552646502458,162.983500100678,58.079745059428));
#38720=CARTESIAN_POINT('Ctrl Pts',(70.5170033810729,162.790715278075,56.8673394809174));
#38721=CARTESIAN_POINT('Ctrl Pts',(69.8261371496123,162.597930455473,55.304209968461));
#38722=CARTESIAN_POINT('Ctrl Pts',(69.1352709181517,162.40514563287,53.7410804560045));
#38723=CARTESIAN_POINT('Ctrl Pts',(69.2068803054901,162.212360810268,51.8613477992548));
#38724=CARTESIAN_POINT('Ctrl Pts',(70.0146680415442,162.019575987666,50.3553102844612));
#38725=CARTESIAN_POINT('Ctrl Pts',(70.8224557775982,161.826791165063,48.8492727696676));
#38726=CARTESIAN_POINT('Ctrl Pts',(72.3487890589397,161.634006342461,47.7498049531876));
#38727=CARTESIAN_POINT('Ctrl Pts',(74.0331492157611,161.441221519858,47.4606667775731));
#38728=CARTESIAN_POINT('Ctrl Pts',(75.7175093725825,161.248436697256,47.1715286019587));
#38729=CARTESIAN_POINT('Ctrl Pts',(77.5231293307851,161.055651874654,47.6990315230374));
#38730=CARTESIAN_POINT('Ctrl Pts',(78.7869273705886,160.862867052051,48.849459502997));
#38731=CARTESIAN_POINT('Ctrl Pts',(79.9447859852113,160.686242654332,49.9034514424893));
#38732=CARTESIAN_POINT('Ctrl Pts',(80.6314498948664,160.509618256613,51.457072930185));
#38733=CARTESIAN_POINT('Ctrl Pts',(80.6314498948689,160.332993858894,53.0228109606264));
#38734=CARTESIAN_POINT('Origin',(74.9879498948689,423.667006141107,53.0228109606356));
#38735=CARTESIAN_POINT('',(80.6381153479507,169.667006141107,53.0212138869262));
#38736=CARTESIAN_POINT('',(80.6382506461677,168.332993858894,53.0199786605548));
#38737=CARTESIAN_POINT('',(80.6314498948689,423.667006141107,53.0228109606222));
#38738=CARTESIAN_POINT('Ctrl Pts',(80.6381153479507,169.667006141107,53.0212138869262));
#38739=CARTESIAN_POINT('Ctrl Pts',(80.6306212693463,169.461472387773,54.8364412321562));
#38740=CARTESIAN_POINT('Ctrl Pts',(78.7087307956748,169.043782624887,58.5295467855593));
#38741=CARTESIAN_POINT('Ctrl Pts',(72.4002672174427,168.413936852449,59.1781432572696));
#38742=CARTESIAN_POINT('Ctrl Pts',(68.415791308239,167.777468823792,54.1747588859273));
#38743=CARTESIAN_POINT('Ctrl Pts',(70.4610652576824,167.141000795135,48.1144983378858));
#38744=CARTESIAN_POINT('Ctrl Pts',(76.6787490482889,166.504532766478,46.5627435525341));
#38745=CARTESIAN_POINT('Ctrl Pts',(80.263241046223,166.013201215135,49.950684280813));
#38746=CARTESIAN_POINT('Ctrl Pts',(80.6330326356445,165.734025673345,52.4244932876794));
#38747=CARTESIAN_POINT('Ctrl Pts',(80.6298086662852,165.667006141107,53.0194647221037));
#38748=CARTESIAN_POINT('Ctrl Pts',(80.6382506461677,168.332993858894,53.0199786605548));
#38749=CARTESIAN_POINT('Ctrl Pts',(80.6278923608474,168.139438198485,54.7293384245555));
#38750=CARTESIAN_POINT('Ctrl Pts',(78.8923093685276,167.733726528524,58.3308523866159));
#38751=CARTESIAN_POINT('Ctrl Pts',(72.7493845539464,167.11585884901,59.3140825259745));
#38752=CARTESIAN_POINT('Ctrl Pts',(69.207833010338,166.585468825129,55.3384589024206));
#38753=CARTESIAN_POINT('Ctrl Pts',(69.3334586153764,166.161156806024,51.4583653347606));
#38754=CARTESIAN_POINT('Ctrl Pts',(71.2200682242025,165.73684478692,48.0654886688141));
#38755=CARTESIAN_POINT('Ctrl Pts',(76.3014478199115,165.206454763039,46.4755981265107));
#38756=CARTESIAN_POINT('Ctrl Pts',(80.1821266586199,164.703145118772,49.7346730674102));
#38757=CARTESIAN_POINT('Ctrl Pts',(80.6293559903944,164.411991484057,52.3174616771233));
#38758=CARTESIAN_POINT('Ctrl Pts',(80.6249991981787,164.332993858894,53.0195421517516));
#38759=CARTESIAN_POINT('Origin',(74.9879498948689,423.667006141107,53.0228109606356));
#38760=CARTESIAN_POINT('',(80.6301199691199,173.667006141107,53.0281825627581));
#38761=CARTESIAN_POINT('',(80.6341311956073,172.332993858894,53.0271652027316));
#38762=CARTESIAN_POINT('',(80.6314498948689,423.667006141107,53.0228109606222));
#38763=CARTESIAN_POINT('Ctrl Pts',(80.6301199691199,173.667006141107,53.0281825627581));
#38764=CARTESIAN_POINT('Ctrl Pts',(80.634874351723,173.613231121306,53.504493868065));
#38765=CARTESIAN_POINT('Ctrl Pts',(80.3629297496774,173.347300091953,55.8552562258711));
#38766=CARTESIAN_POINT('Ctrl Pts',(77.0704786758444,172.869213053048,59.3668862437205));
#38767=CARTESIAN_POINT('Ctrl Pts',(70.781351567379,172.23274502439,58.2020756788708));
#38768=CARTESIAN_POINT('Ctrl Pts',(68.351646798808,171.596276995734,52.2854517956076));
#38769=CARTESIAN_POINT('Ctrl Pts',(72.0284531099989,170.959808967076,47.0367729157542));
#38770=CARTESIAN_POINT('Ctrl Pts',(77.3480421827307,170.429418943196,47.260698415578));
#38771=CARTESIAN_POINT('Ctrl Pts',(80.0467424555462,170.005106924091,50.0513837657998));
#38772=CARTESIAN_POINT('Ctrl Pts',(80.6258905036357,169.78632865832,51.9674207687533));
#38773=CARTESIAN_POINT('Ctrl Pts',(80.6383568056569,169.673628397326,52.9627276267381));
#38774=CARTESIAN_POINT('Ctrl Pts',(80.6381153479507,169.667006141107,53.0212138869262));
#38775=CARTESIAN_POINT('Ctrl Pts',(80.6341311956073,172.332993858894,53.0271652027315));
#38776=CARTESIAN_POINT('Ctrl Pts',(80.6376049499977,172.291196932018,53.3971740870304));
#38777=CARTESIAN_POINT('Ctrl Pts',(80.4355736701072,172.037243995589,55.6418677387875));
#38778=CARTESIAN_POINT('Ctrl Pts',(77.4232005111353,171.571135049609,59.2405940969629));
#38779=CARTESIAN_POINT('Ctrl Pts',(72.1424114296051,171.040745025728,58.5613024007155));
#38780=CARTESIAN_POINT('Ctrl Pts',(69.692973246283,170.616433006623,55.5494656733147));
#38781=CARTESIAN_POINT('Ctrl Pts',(68.8925550574566,170.192120987518,51.7507502839452));
#38782=CARTESIAN_POINT('Ctrl Pts',(71.6864479885501,169.661730963638,47.2183852476993));
#38783=CARTESIAN_POINT('Ctrl Pts',(78.0939616097122,169.025262934981,47.1120657835623));
#38784=CARTESIAN_POINT('Ctrl Pts',(80.5579189119324,168.582350566733,50.8188324455204));
#38785=CARTESIAN_POINT('Ctrl Pts',(80.639246058666,168.351594208037,52.8557122766402));
#38786=CARTESIAN_POINT('Ctrl Pts',(80.6382506461677,168.332993858894,53.0199786605548));
#38787=CARTESIAN_POINT('Origin',(74.9879498948689,423.667006141107,53.0228109606356));
#38788=CARTESIAN_POINT('',(80.6222904215375,177.667006141107,53.0205978427077));
#38789=CARTESIAN_POINT('',(80.622100390063,176.332993858894,53.0243351757114));
#38790=CARTESIAN_POINT('',(80.6314498948689,423.667006141107,53.0228109606222));
#38791=CARTESIAN_POINT('Ctrl Pts',(80.6222904215376,177.667006141107,53.0205978427077));
#38792=CARTESIAN_POINT('Ctrl Pts',(80.620411075197,177.552833845287,54.0372215553682));
#38793=CARTESIAN_POINT('Ctrl Pts',(79.8716611686231,177.226505539914,56.9464913633814));
#38794=CARTESIAN_POINT('Ctrl Pts',(75.208166943184,176.688021224989,59.6915257515102));
#38795=CARTESIAN_POINT('Ctrl Pts',(69.4940514634066,176.051553196332,56.8177150893079));
#38796=CARTESIAN_POINT('Ctrl Pts',(68.828326029216,175.415085167675,50.4439921364254));
#38797=CARTESIAN_POINT('Ctrl Pts',(72.9914360826229,174.884695143794,47.1248529083393));
#38798=CARTESIAN_POINT('Ctrl Pts',(76.8588776947801,174.46038312469,47.4622003004928));
#38799=CARTESIAN_POINT('Ctrl Pts',(79.7273594481839,174.089846125386,49.2690685230197));
#38800=CARTESIAN_POINT('Ctrl Pts',(80.6161171137957,173.825387130859,51.6253256927186));
#38801=CARTESIAN_POINT('Ctrl Pts',(80.6301199691199,173.667006141107,53.0281825627581));
#38802=CARTESIAN_POINT('Ctrl Pts',(80.622100390063,176.332993858894,53.0243351757114));
#38803=CARTESIAN_POINT('Ctrl Pts',(80.6228905078415,176.230799655998,53.9343920094406));
#38804=CARTESIAN_POINT('Ctrl Pts',(79.9847919659374,175.91644944355,56.7319395831436));
#38805=CARTESIAN_POINT('Ctrl Pts',(76.4713185355127,175.496021226327,59.0702562117385));
#38806=CARTESIAN_POINT('Ctrl Pts',(72.6470540467699,175.071709207221,58.4024920268817));
#38807=CARTESIAN_POINT('Ctrl Pts',(69.551817146766,174.647397188117,56.0593282640832));
#38808=CARTESIAN_POINT('Ctrl Pts',(68.6892013076634,174.117007164236,50.8053712366301));
#38809=CARTESIAN_POINT('Ctrl Pts',(73.4571407575176,173.480539135579,46.5235155598984));
#38810=CARTESIAN_POINT('Ctrl Pts',(79.2182824818878,172.885868033799,48.1117410261231));
#38811=CARTESIAN_POINT('Ctrl Pts',(80.6199726041598,172.50335294157,51.5190549462608));
#38812=CARTESIAN_POINT('Ctrl Pts',(80.6341311956073,172.332993858894,53.0271652027315));
#38813=CARTESIAN_POINT('Origin',(74.9879498948689,423.667006141107,53.0228109606356));
#38814=CARTESIAN_POINT('',(80.6352537257938,181.667006141107,53.0187032745236));
#38815=CARTESIAN_POINT('',(80.6313512644076,180.332993858894,53.0175461958891));
#38816=CARTESIAN_POINT('',(80.6314498948689,423.667006141107,53.0228109606222));
#38817=CARTESIAN_POINT('Ctrl Pts',(80.6352537257938,181.667006141107,53.0187032745236));
#38818=CARTESIAN_POINT('Ctrl Pts',(80.6210959151668,181.492436569267,54.5633324678709));
#38819=CARTESIAN_POINT('Ctrl Pts',(79.1610194561343,181.105710987875,58.0064109974519));
#38820=CARTESIAN_POINT('Ctrl Pts',(73.3284950085148,180.506829396931,59.4904555706305));
#38821=CARTESIAN_POINT('Ctrl Pts',(68.6464467632618,179.870361368274,55.1148460287544));
#38822=CARTESIAN_POINT('Ctrl Pts',(69.6131321617587,179.339971344393,49.8790376028731));
#38823=CARTESIAN_POINT('Ctrl Pts',(72.7542485557096,178.915659325288,47.5977450556339));
#38824=CARTESIAN_POINT('Ctrl Pts',(76.5910088428193,178.491347306184,47.0059863330989));
#38825=CARTESIAN_POINT('Ctrl Pts',(80.0226830505157,178.075129578123,49.3894393899014));
#38826=CARTESIAN_POINT('Ctrl Pts',(80.6239032938417,177.764989854839,52.148122027812));
#38827=CARTESIAN_POINT('Ctrl Pts',(80.6222904215376,177.667006141107,53.0205978427077));
#38828=CARTESIAN_POINT('Ctrl Pts',(80.6313512644076,180.332993858894,53.0175461958891));
#38829=CARTESIAN_POINT('Ctrl Pts',(80.6167777966843,180.170402379979,54.4569563804603));
#38830=CARTESIAN_POINT('Ctrl Pts',(79.6849478057585,179.901732896288,56.8499640912845));
#38831=CARTESIAN_POINT('Ctrl Pts',(76.7481860199208,179.52698540782,58.6194466045056));
#38832=CARTESIAN_POINT('Ctrl Pts',(72.8748126305075,179.102673388715,58.8799969309715));
#38833=CARTESIAN_POINT('Ctrl Pts',(68.7783742806616,178.572283364835,55.4789142536309));
#38834=CARTESIAN_POINT('Ctrl Pts',(69.5704243653522,177.935815336178,49.1196539745438));
#38835=CARTESIAN_POINT('Ctrl Pts',(75.340431971015,177.299347307521,46.3597779503322));
#38836=CARTESIAN_POINT('Ctrl Pts',(79.9125147985732,176.76507348176,49.1746134232404));
#38837=CARTESIAN_POINT('Ctrl Pts',(80.6212502168054,176.442955665551,52.0451065036207));
#38838=CARTESIAN_POINT('Ctrl Pts',(80.622100390063,176.332993858894,53.0243351757114));
#38839=CARTESIAN_POINT('Origin',(74.9879498948689,423.667006141107,53.0228109606356));
#38840=CARTESIAN_POINT('',(80.6374622679322,185.667006141107,53.0261725848653));
#38841=CARTESIAN_POINT('',(80.6375466782535,184.332993858894,53.0249433462478));
#38842=CARTESIAN_POINT('',(80.6314498948689,423.667006141107,53.0228109606222));
#38843=CARTESIAN_POINT('Ctrl Pts',(80.6374622679322,185.667006141107,53.0261725848653));
#38844=CARTESIAN_POINT('Ctrl Pts',(80.6388609160972,185.6441953028,53.2276980420194));
#38845=CARTESIAN_POINT('Ctrl Pts',(80.537213063289,185.409228454941,55.3020984961681));
#38846=CARTESIAN_POINT('Ctrl Pts',(77.9760801015144,184.962105597529,58.9940164661573));
#38847=CARTESIAN_POINT('Ctrl Pts',(71.5719371009017,184.325637568872,58.760591828347));
#38848=CARTESIAN_POINT('Ctrl Pts',(68.8685169582398,183.795247544992,54.1736876365801));
#38849=CARTESIAN_POINT('Ctrl Pts',(69.7441447209343,183.370935525887,50.3916003943771));
#38850=CARTESIAN_POINT('Ctrl Pts',(72.2528560934249,182.946623506783,47.4289537505847));
#38851=CARTESIAN_POINT('Ctrl Pts',(77.5460829854539,182.416233482901,46.8545674679323));
#38852=CARTESIAN_POINT('Ctrl Pts',(80.4599026306944,181.954335026085,50.4793096779496));
#38853=CARTESIAN_POINT('Ctrl Pts',(80.6383020329052,181.70459257882,52.6861303733431));
#38854=CARTESIAN_POINT('Ctrl Pts',(80.6352537257938,181.667006141107,53.0187032745236));
#38855=CARTESIAN_POINT('Ctrl Pts',(80.6375466782535,184.332993858894,53.0249433462478));
#38856=CARTESIAN_POINT('Ctrl Pts',(80.6380606391403,184.322161113512,53.1206316251517));
#38857=CARTESIAN_POINT('Ctrl Pts',(80.6157170314747,184.205250363353,54.1532044388168));
#38858=CARTESIAN_POINT('Ctrl Pts',(79.9867931126735,183.982261608419,56.094020531795));
#38859=CARTESIAN_POINT('Ctrl Pts',(77.2332563931867,183.557949589314,58.8306139288627));
#38860=CARTESIAN_POINT('Ctrl Pts',(71.9102716857639,183.027559565433,58.9489538491949));
#38861=CARTESIAN_POINT('Ctrl Pts',(68.3383237334809,182.391091536777,53.6283596662101));
#38862=CARTESIAN_POINT('Ctrl Pts',(70.8849370199572,181.754623508119,47.761106117269));
#38863=CARTESIAN_POINT('Ctrl Pts',(77.1959362348037,181.118155479463,46.7213021219764));
#38864=CARTESIAN_POINT('Ctrl Pts',(80.3896907770719,180.644278929721,50.2660677252129));
#38865=CARTESIAN_POINT('Ctrl Pts',(80.6357938532337,180.382558389531,52.5787551185917));
#38866=CARTESIAN_POINT('Ctrl Pts',(80.6313512644076,180.332993858894,53.0175461958891));
#38867=CARTESIAN_POINT('Origin',(74.9879498948689,423.667006141107,53.0228109606356));
#38868=CARTESIAN_POINT('',(80.6314498948689,189.667006141107,53.022810960627));
#38869=CARTESIAN_POINT('',(80.6291610643578,188.332993858894,53.0259379629415));
#38870=CARTESIAN_POINT('',(80.6314498948689,423.667006141107,53.0228109606222));
#38871=CARTESIAN_POINT('Ctrl Pts',(80.6242855516874,189.667006141107,53.0256421919302));
#38872=CARTESIAN_POINT('Ctrl Pts',(80.6282930065685,189.583798026781,53.7653643749688));
#38873=CARTESIAN_POINT('Ctrl Pts',(80.1488658331061,189.288433902902,56.3867402663278));
#38874=CARTESIAN_POINT('Ctrl Pts',(76.1712915211055,188.780913769471,59.5947950818913));
#38875=CARTESIAN_POINT('Ctrl Pts',(71.122455804744,188.25052374559,57.9044020975852));
#38876=CARTESIAN_POINT('Ctrl Pts',(69.3035327663159,187.826211726486,54.4747626315898));
#38877=CARTESIAN_POINT('Ctrl Pts',(69.2549135694621,187.40189970738,50.5929403713447));
#38878=CARTESIAN_POINT('Ctrl Pts',(72.8746450227851,186.871509683501,46.6883642435143));
#38879=CARTESIAN_POINT('Ctrl Pts',(78.9551331645321,186.25785249315,47.7857479804749));
#38880=CARTESIAN_POINT('Ctrl Pts',(80.6258525553586,185.856351312352,51.3533768865391));
#38881=CARTESIAN_POINT('Ctrl Pts',(80.6374622679322,185.667006141107,53.0261725848653));
#38882=CARTESIAN_POINT('Ctrl Pts',(80.6291610643578,188.332993858894,53.0259379629415));
#38883=CARTESIAN_POINT('Ctrl Pts',(80.6323067140524,188.261763837492,53.658494549645));
#38884=CARTESIAN_POINT('Ctrl Pts',(80.2325386454109,187.978377806538,56.1705775971628));
#38885=CARTESIAN_POINT('Ctrl Pts',(76.5502474625308,187.482835766032,59.515152526242));
#38886=CARTESIAN_POINT('Ctrl Pts',(70.3645745965685,186.846367737375,57.8403433343832));
#38887=CARTESIAN_POINT('Ctrl Pts',(68.4399397736334,186.209899708718,51.7406970957261));
#38888=CARTESIAN_POINT('Ctrl Pts',(72.5228993479575,185.573431680061,46.8173502104404));
#38889=CARTESIAN_POINT('Ctrl Pts',(78.7751754834161,184.947796396786,47.5858082695843));
#38890=CARTESIAN_POINT('Ctrl Pts',(80.6279948721579,184.534317123064,51.2466059099056));
#38891=CARTESIAN_POINT('Ctrl Pts',(80.6375466782535,184.332993858894,53.0249433462478));
#38892=CARTESIAN_POINT('Origin',(74.9879498948689,423.667006141107,53.0228109606356));
#38893=CARTESIAN_POINT('',(80.6314498948689,193.667006141107,53.0228109606274));
#38894=CARTESIAN_POINT('',(80.6217190853732,192.332993858894,53.0205375180906));
#38895=CARTESIAN_POINT('',(80.6314498948689,423.667006141107,53.0228109606222));
#38896=CARTESIAN_POINT('Ctrl Pts',(80.6314498948689,193.667006141107,53.0228109606274));
#38897=CARTESIAN_POINT('Ctrl Pts',(80.6314498948714,193.474221318505,54.7318077489466));
#38898=CARTESIAN_POINT('Ctrl Pts',(79.8060659192683,193.281436495902,56.4221521097277));
#38899=CARTESIAN_POINT('Ctrl Pts',(78.4584055093426,193.0886516733,57.4730952299793));
#38900=CARTESIAN_POINT('Ctrl Pts',(77.1107450994169,192.895866850697,58.5240383502309));
#38901=CARTESIAN_POINT('Ctrl Pts',(75.2702256751607,192.703082028095,58.9126397065624));
#38902=CARTESIAN_POINT('Ctrl Pts',(73.6127451627025,192.510297205493,58.4961923829948));
#38903=CARTESIAN_POINT('Ctrl Pts',(71.9552646502443,192.31751238289,58.0797450594272));
#38904=CARTESIAN_POINT('Ctrl Pts',(70.5170033810717,192.124727560288,56.8673394809161));
#38905=CARTESIAN_POINT('Ctrl Pts',(69.8261371496116,191.931942737685,55.3042099684593));
#38906=CARTESIAN_POINT('Ctrl Pts',(69.1352709181514,191.739157915083,53.7410804560025));
#38907=CARTESIAN_POINT('Ctrl Pts',(69.2068803054905,191.546373092481,51.8613477992527));
#38908=CARTESIAN_POINT('Ctrl Pts',(70.0146680415451,191.353588269878,50.3553102844593));
#38909=CARTESIAN_POINT('Ctrl Pts',(70.8224557775998,191.160803447276,48.849272769666));
#38910=CARTESIAN_POINT('Ctrl Pts',(72.3487890589419,190.968018624673,47.7498049531864));
#38911=CARTESIAN_POINT('Ctrl Pts',(74.0331492157635,190.775233802071,47.4606667775727));
#38912=CARTESIAN_POINT('Ctrl Pts',(75.7175093725851,190.582448979469,47.171528601959));
#38913=CARTESIAN_POINT('Ctrl Pts',(77.5231293307877,190.389664156866,47.6990315230386));
#38914=CARTESIAN_POINT('Ctrl Pts',(78.7869273705907,190.196879334264,48.8494595029988));
#38915=CARTESIAN_POINT('Ctrl Pts',(79.9447859852123,190.020254936545,49.9034514424912));
#38916=CARTESIAN_POINT('Ctrl Pts',(80.6314498948665,189.843630538826,51.4570729301863));
#38917=CARTESIAN_POINT('Ctrl Pts',(80.6314498948689,189.667006141107,53.022810960627));
#38918=CARTESIAN_POINT('Ctrl Pts',(80.6217190853732,192.332993858894,53.0205375180906));
#38919=CARTESIAN_POINT('Ctrl Pts',(80.6161145337634,192.201366561473,54.1905476069636));
#38920=CARTESIAN_POINT('Ctrl Pts',(79.6948479408142,191.8575832545,57.2532805854104));
#38921=CARTESIAN_POINT('Ctrl Pts',(74.65630346539,191.301643937974,59.6917110173807));
#38922=CARTESIAN_POINT('Ctrl Pts',(69.2035016326957,190.665175909317,56.3485305538422));
#38923=CARTESIAN_POINT('Ctrl Pts',(69.0577500836245,190.02870788066,49.9541064261852));
#38924=CARTESIAN_POINT('Ctrl Pts',(74.3725601345045,189.392239852003,46.3735577591653));
#38925=CARTESIAN_POINT('Ctrl Pts',(79.2578336803251,188.861849828122,48.4906956655628));
#38926=CARTESIAN_POINT('Ctrl Pts',(80.5210935629515,188.508767830419,51.4638814847399));
#38927=CARTESIAN_POINT('Ctrl Pts',(80.6276221128581,188.367841842269,52.7164712383355));
#38928=CARTESIAN_POINT('Ctrl Pts',(80.6291610643578,188.332993858894,53.0259379629415));
#38929=CARTESIAN_POINT('Origin',(74.9879498948689,423.667006141107,53.0228109606356));
#38930=CARTESIAN_POINT('',(80.640955218553,197.667006141107,53.0225373373321));
#38931=CARTESIAN_POINT('',(80.6392284044996,196.332993858894,53.0181925457554));
#38932=CARTESIAN_POINT('',(80.6314498948689,423.667006141107,53.0228109606222));
#38933=CARTESIAN_POINT('Ctrl Pts',(80.640955218553,197.667006141107,53.0225373373321));
#38934=CARTESIAN_POINT('Ctrl Pts',(80.6345183935671,197.463003474742,54.821619328168));
#38935=CARTESIAN_POINT('Ctrl Pts',(79.2099563276419,197.1529228036,57.5592190407096));
#38936=CARTESIAN_POINT('Ctrl Pts',(75.6295355167696,196.736764127683,58.8545456627842));
#38937=CARTESIAN_POINT('Ctrl Pts',(71.7791577583434,196.312452108578,58.3590671026649));
#38938=CARTESIAN_POINT('Ctrl Pts',(68.4199739824153,195.782062084697,54.2282009838377));
#38939=CARTESIAN_POINT('Ctrl Pts',(70.4301108370362,195.14559405604,48.1432289658392));
#38940=CARTESIAN_POINT('Ctrl Pts',(76.6257663738702,194.509126027384,46.5545956201064));
#38941=CARTESIAN_POINT('Ctrl Pts',(80.2598992249104,194.016263389073,49.9198215535398));
#38942=CARTESIAN_POINT('Ctrl Pts',(80.6312959048558,193.735556760314,52.4090928284891));
#38943=CARTESIAN_POINT('Ctrl Pts',(80.6265789855776,193.667006141107,53.018365003171));
#38944=CARTESIAN_POINT('Ctrl Pts',(80.6392284044996,196.332993858894,53.0181925457554));
#38945=CARTESIAN_POINT('Ctrl Pts',(80.6281979805195,196.140969285454,54.7138512508588));
#38946=CARTESIAN_POINT('Ctrl Pts',(78.9109854809454,195.73678870246,58.3085405343815));
#38947=CARTESIAN_POINT('Ctrl Pts',(72.8014733044529,195.120452109916,59.3267440686173));
#38948=CARTESIAN_POINT('Ctrl Pts',(68.498429651078,194.483984081258,54.5945438662197));
#38949=CARTESIAN_POINT('Ctrl Pts',(70.1632321105985,193.847516052601,48.4061702992275));
#38950=CARTESIAN_POINT('Ctrl Pts',(75.2398670646046,193.317126028721,46.8011942632874));
#38951=CARTESIAN_POINT('Ctrl Pts',(78.7289430044913,192.892814009616,48.5033273286335));
#38952=CARTESIAN_POINT('Ctrl Pts',(80.332017025861,192.600129287933,50.648315489177));
#38953=CARTESIAN_POINT('Ctrl Pts',(80.6251479130712,192.413522571025,52.3047330650381));
#38954=CARTESIAN_POINT('Ctrl Pts',(80.6217190853732,192.332993858894,53.0205375180906));
#38955=CARTESIAN_POINT('Origin',(74.9879498948689,423.667006141107,53.0228109606356));
#38956=CARTESIAN_POINT('',(80.6276048913152,201.667006141107,53.027244000928));
#38957=CARTESIAN_POINT('',(80.6340609079321,200.332993858894,53.0281408858031));
#38958=CARTESIAN_POINT('',(80.6314498948689,423.667006141107,53.0228109606222));
#38959=CARTESIAN_POINT('Ctrl Pts',(80.6276048913152,201.667006141107,53.027244000928));
#38960=CARTESIAN_POINT('Ctrl Pts',(80.6317528202149,201.614762208275,53.4905111224134));
#38961=CARTESIAN_POINT('Ctrl Pts',(80.4741758592005,201.456440270666,54.8920866086593));
#38962=CARTESIAN_POINT('Ctrl Pts',(79.2963758820999,201.192040328282,57.0050499361194));
#38963=CARTESIAN_POINT('Ctrl Pts',(76.064451658235,200.767728309176,59.1557646138185));
#38964=CARTESIAN_POINT('Ctrl Pts',(70.8195529427137,200.237338285297,58.2396816294403));
#38965=CARTESIAN_POINT('Ctrl Pts',(68.3471157639746,199.600870256639,52.3274410178494));
#38966=CARTESIAN_POINT('Ctrl Pts',(71.9831085027866,198.964402227983,47.0653634605732));
#38967=CARTESIAN_POINT('Ctrl Pts',(78.3759491980706,198.327934199325,47.2690575728888));
#38968=CARTESIAN_POINT('Ctrl Pts',(80.6079896926466,197.895468837034,51.0078303424387));
#38969=CARTESIAN_POINT('Ctrl Pts',(80.6412124781471,197.675159484294,52.9506337041384));
#38970=CARTESIAN_POINT('Ctrl Pts',(80.640955218553,197.667006141107,53.0225373373321));
#38971=CARTESIAN_POINT('Ctrl Pts',(80.6340609079321,200.332993858894,53.0281408858031));
#38972=CARTESIAN_POINT('Ctrl Pts',(80.6374212133726,200.292728018986,53.3847935610186));
#38973=CARTESIAN_POINT('Ctrl Pts',(80.444465303885,200.040306169526,55.6167934462686));
#38974=CARTESIAN_POINT('Ctrl Pts',(77.4708299078219,199.575728310514,59.2159974868797));
#38975=CARTESIAN_POINT('Ctrl Pts',(71.1190079787084,198.939260281857,58.4648239866103));
#38976=CARTESIAN_POINT('Ctrl Pts',(68.3180409606457,198.3027922532,52.7009608376928));
#38977=CARTESIAN_POINT('Ctrl Pts',(71.098459721967,197.77240222932,48.1603174867096));
#38978=CARTESIAN_POINT('Ctrl Pts',(74.8488389159196,197.348090210214,47.1575394509773));
#38979=CARTESIAN_POINT('Ctrl Pts',(78.6425415842146,196.92377819111,47.9813889218711));
#38980=CARTESIAN_POINT('Ctrl Pts',(80.5516622018494,196.58541274067,50.7907689994262));
#38981=CARTESIAN_POINT('Ctrl Pts',(80.6403848100141,196.353125295006,52.8404233973733));
#38982=CARTESIAN_POINT('Ctrl Pts',(80.6392284044996,196.332993858894,53.0181925457554));
#38983=CARTESIAN_POINT('Origin',(74.9879498948689,423.667006141107,53.0228109606356));
#38984=CARTESIAN_POINT('',(80.626574651087,205.667006141107,53.0221197938247));
#38985=CARTESIAN_POINT('',(80.6223425337288,204.332993858894,53.0236933593282));
#38986=CARTESIAN_POINT('',(80.6314498948689,423.667006141107,53.0228109606222));
#38987=CARTESIAN_POINT('Ctrl Pts',(80.626574651087,205.667006141107,53.0221197938247));
#38988=CARTESIAN_POINT('Ctrl Pts',(80.6265170704333,205.660442937031,53.0804789074155));
#38989=CARTESIAN_POINT('Ctrl Pts',(80.6105409825448,205.54780172818,54.0821013304582));
#38990=CARTESIAN_POINT('Ctrl Pts',(79.8222544701088,205.223004509775,56.947282442927));
#38991=CARTESIAN_POINT('Ctrl Pts',(75.2616679235261,204.692614485895,59.6948686777458));
#38992=CARTESIAN_POINT('Ctrl Pts',(69.5181641574838,204.056146457238,56.8523878495988));
#38993=CARTESIAN_POINT('Ctrl Pts',(68.8128385238247,203.419678428581,50.4953117049742));
#38994=CARTESIAN_POINT('Ctrl Pts',(73.7729845636653,202.783210399924,46.4571368186103));
#38995=CARTESIAN_POINT('Ctrl Pts',(79.361453787666,202.198986304099,48.2932371232192));
#38996=CARTESIAN_POINT('Ctrl Pts',(80.6149086050964,201.826918217827,51.6092418817071));
#38997=CARTESIAN_POINT('Ctrl Pts',(80.6276048913152,201.667006141107,53.027244000928));
#38998=CARTESIAN_POINT('Ctrl Pts',(80.6223425337288,204.332993858894,53.0236933593282));
#38999=CARTESIAN_POINT('Ctrl Pts',(80.6230594866242,204.232330742967,53.9192679121389));
#39000=CARTESIAN_POINT('Ctrl Pts',(79.9972097326935,203.919511617488,56.70082270821));
#39001=CARTESIAN_POINT('Ctrl Pts',(75.6353879853842,203.394536482455,59.668489377038));
#39002=CARTESIAN_POINT('Ctrl Pts',(69.7411399911392,202.758068453799,57.153459596108));
#39003=CARTESIAN_POINT('Ctrl Pts',(68.8629228367167,202.227678429917,51.902087877635));
#39004=CARTESIAN_POINT('Ctrl Pts',(71.0368999365241,201.803366410813,48.6857651951434));
#39005=CARTESIAN_POINT('Ctrl Pts',(74.4413565467986,201.379054391709,46.8201331300155));
#39006=CARTESIAN_POINT('Ctrl Pts',(79.1976249869001,200.888930207736,48.0791902280285));
#39007=CARTESIAN_POINT('Ctrl Pts',(80.6197161563126,200.504884028539,51.5056322534882));
#39008=CARTESIAN_POINT('Ctrl Pts',(80.6340609079321,200.332993858894,53.0281408858031));
#39009=CARTESIAN_POINT('Origin',(74.9879498948689,423.667006141107,53.0228109606356));
#39010=CARTESIAN_POINT('',(80.6311262248081,209.667006141107,53.0183737769086));
#39011=CARTESIAN_POINT('',(80.6305392456029,208.332993858894,53.0176923059613));
#39012=CARTESIAN_POINT('',(80.6314498948689,423.667006141107,53.0228109606222));
#39013=CARTESIAN_POINT('Ctrl Pts',(80.6311262248081,209.667006141107,53.0183737769086));
#39014=CARTESIAN_POINT('Ctrl Pts',(80.6168278466814,209.493967656236,54.5505890003982));
#39015=CARTESIAN_POINT('Ctrl Pts',(79.1885638263849,209.108773161812,57.9803147109756));
#39016=CARTESIAN_POINT('Ctrl Pts',(73.3694517075265,208.511422657837,59.5008055828234));
#39017=CARTESIAN_POINT('Ctrl Pts',(68.6683970655276,207.874954629179,55.1637564563535));
#39018=CARTESIAN_POINT('Ctrl Pts',(69.7653637905974,207.238486600523,48.8624258785963));
#39019=CARTESIAN_POINT('Ctrl Pts',(75.6735905312152,206.602018571865,46.3804373005538));
#39020=CARTESIAN_POINT('Ctrl Pts',(80.0013855133694,206.07819175206,49.3672640149237));
#39021=CARTESIAN_POINT('Ctrl Pts',(80.6274477196698,205.766520941808,52.1372477875521));
#39022=CARTESIAN_POINT('Ctrl Pts',(80.626574651087,205.667006141107,53.0221197938247));
#39023=CARTESIAN_POINT('Ctrl Pts',(80.6305392456029,208.332993858894,53.0176923059613));
#39024=CARTESIAN_POINT('Ctrl Pts',(80.6179689885373,208.171933466948,54.445179660362));
#39025=CARTESIAN_POINT('Ctrl Pts',(79.3448628719476,207.798717065448,57.7735864037716));
#39026=CARTESIAN_POINT('Ctrl Pts',(73.7352061577403,207.213344654398,59.5819163913665));
#39027=CARTESIAN_POINT('Ctrl Pts',(69.6286797739237,206.682954630516,56.1930196438724));
#39028=CARTESIAN_POINT('Ctrl Pts',(69.1609966055946,206.258642611412,52.3391654795781));
#39029=CARTESIAN_POINT('Ctrl Pts',(70.5080046768267,205.834330592307,48.6982221958113));
#39030=CARTESIAN_POINT('Ctrl Pts',(75.2874147618561,205.303940568427,46.3518592644304));
#39031=CARTESIAN_POINT('Ctrl Pts',(79.899510904419,204.768135655696,49.1506053771233));
#39032=CARTESIAN_POINT('Ctrl Pts',(80.6215484479093,204.444486752519,52.0317689843454));
#39033=CARTESIAN_POINT('Ctrl Pts',(80.6223425337288,204.332993858894,53.0236933593282));
#39034=CARTESIAN_POINT('Origin',(74.9879498948689,423.667006141107,53.0228109606356));
#39035=CARTESIAN_POINT('',(80.6382744059561,213.667006141107,53.0259194210108));
#39036=CARTESIAN_POINT('',(80.6406766150791,212.332993858894,53.0236886644395));
#39037=CARTESIAN_POINT('',(80.6314498948689,423.667006141107,53.0228109606222));
#39038=CARTESIAN_POINT('Ctrl Pts',(80.6382744059561,213.667006141107,53.0259194210108));
#39039=CARTESIAN_POINT('Ctrl Pts',(80.6395083226358,213.645726389769,53.2138936786102));
#39040=CARTESIAN_POINT('Ctrl Pts',(80.5450631830952,213.412290628878,55.2746757555776));
#39041=CARTESIAN_POINT('Ctrl Pts',(78.0159571360404,212.966698858435,58.9727077333983));
#39042=CARTESIAN_POINT('Ctrl Pts',(71.6194256917035,212.330230829778,58.7843319643082));
#39043=CARTESIAN_POINT('Ctrl Pts',(68.3174643030566,211.693762801121,53.3056650395866));
#39044=CARTESIAN_POINT('Ctrl Pts',(71.1496401123775,211.057294772464,47.5586365481913));
#39045=CARTESIAN_POINT('Ctrl Pts',(76.4416934236012,210.526904748583,46.9679457097492));
#39046=CARTESIAN_POINT('Ctrl Pts',(79.5342341192608,210.102592729479,49.3146003451081));
#39047=CARTESIAN_POINT('Ctrl Pts',(80.5273629254713,209.851319195245,51.3879369939694));
#39048=CARTESIAN_POINT('Ctrl Pts',(80.6343585529211,209.706123665788,52.6719972649662));
#39049=CARTESIAN_POINT('Ctrl Pts',(80.6311262248081,209.667006141107,53.0183737769086));
#39050=CARTESIAN_POINT('Ctrl Pts',(80.6406766150791,212.332993858894,53.0236886644395));
#39051=CARTESIAN_POINT('Ctrl Pts',(80.6409564956532,212.32369220048,53.1058016007408));
#39052=CARTESIAN_POINT('Ctrl Pts',(80.6016966775368,212.102234532514,55.0605671760039));
#39053=CARTESIAN_POINT('Ctrl Pts',(78.3435294198688,211.668620854996,58.7960171796599));
#39054=CARTESIAN_POINT('Ctrl Pts',(73.0203157428126,211.138230831115,58.9307022339566));
#39055=CARTESIAN_POINT('Ctrl Pts',(70.1404093382657,210.713918812011,56.3274859477036));
#39056=CARTESIAN_POINT('Ctrl Pts',(68.7697904747173,210.289606792905,52.6954344925807));
#39057=CARTESIAN_POINT('Ctrl Pts',(70.8397506710645,209.759216769025,47.7898625183533));
#39058=CARTESIAN_POINT('Ctrl Pts',(77.1560180005676,209.122748740368,46.7074779213906));
#39059=CARTESIAN_POINT('Ctrl Pts',(80.3767059902175,208.647341103658,50.2362176050114));
#39060=CARTESIAN_POINT('Ctrl Pts',(80.6345270978642,208.3840894765,52.5648289600087));
#39061=CARTESIAN_POINT('Ctrl Pts',(80.6305392456029,208.332993858894,53.0176923059613));
#39062=CARTESIAN_POINT('Origin',(74.9879498948689,423.667006141107,53.0228109606356));
#39063=CARTESIAN_POINT('',(80.6314498948689,217.667006141107,53.0228109606278));
#39064=CARTESIAN_POINT('',(80.6293939811109,216.332993858894,53.0260232150293));
#39065=CARTESIAN_POINT('',(80.6314498948689,423.667006141107,53.0228109606222));
#39066=CARTESIAN_POINT('Ctrl Pts',(80.6245279079042,217.667006141107,53.0258075780124));
#39067=CARTESIAN_POINT('Ctrl Pts',(80.628672686297,217.585329113749,53.7518430852284));
#39068=CARTESIAN_POINT('Ctrl Pts',(80.1610640643919,217.291496076839,56.3591821658415));
#39069=CARTESIAN_POINT('Ctrl Pts',(76.2187228071657,216.785507030377,59.5860802860795));
#39070=CARTESIAN_POINT('Ctrl Pts',(71.1576983282718,216.255117006495,57.9321749584298));
#39071=CARTESIAN_POINT('Ctrl Pts',(69.31426183066,215.830804987392,54.5157242093268));
#39072=CARTESIAN_POINT('Ctrl Pts',(69.2372749896401,215.406492968286,50.6344011155516));
#39073=CARTESIAN_POINT('Ctrl Pts',(72.829541004845,214.876102944406,46.7037054021372));
#39074=CARTESIAN_POINT('Ctrl Pts',(78.9315707928124,214.260914667087,47.7600025531877));
#39075=CARTESIAN_POINT('Ctrl Pts',(80.6272063537493,213.857882399321,51.3398178138765));
#39076=CARTESIAN_POINT('Ctrl Pts',(80.6382744059561,213.667006141107,53.0259194210108));
#39077=CARTESIAN_POINT('Ctrl Pts',(80.6293939811109,216.332993858894,53.0260232150293));
#39078=CARTESIAN_POINT('Ctrl Pts',(80.6326101171936,216.263294924461,53.6449102643575));
#39079=CARTESIAN_POINT('Ctrl Pts',(80.2440137931953,215.981439980475,56.1430625001089));
#39080=CARTESIAN_POINT('Ctrl Pts',(76.5965009308421,215.487429026938,59.503735860729));
#39081=CARTESIAN_POINT('Ctrl Pts',(70.4003730145984,214.85096099828,57.873534909508));
#39082=CARTESIAN_POINT('Ctrl Pts',(68.429181621647,214.214492969624,51.7880485052417));
#39083=CARTESIAN_POINT('Ctrl Pts',(72.4813418470979,213.578024940966,46.8351607156745));
#39084=CARTESIAN_POINT('Ctrl Pts',(78.7452529776764,212.950858570724,47.5606292096147));
#39085=CARTESIAN_POINT('Ctrl Pts',(80.6345728656489,212.535848210033,51.2329363413034));
#39086=CARTESIAN_POINT('Ctrl Pts',(80.6406766150791,212.332993858894,53.0236886644395));
#39087=CARTESIAN_POINT('Origin',(74.9879498948689,423.667006141107,53.0228109606356));
#39088=CARTESIAN_POINT('',(80.6314498948689,221.667006141107,53.0228109606282));
#39089=CARTESIAN_POINT('',(80.6215141333136,220.332993858894,53.0207205529598));
#39090=CARTESIAN_POINT('',(80.6314498948689,423.667006141107,53.0228109606222));
#39091=CARTESIAN_POINT('Ctrl Pts',(80.6314498948689,221.667006141107,53.0228109606279));
#39092=CARTESIAN_POINT('Ctrl Pts',(80.6314498948712,221.474221318505,54.7318077489469));
#39093=CARTESIAN_POINT('Ctrl Pts',(79.8060659192682,221.281436495902,56.4221521097277));
#39094=CARTESIAN_POINT('Ctrl Pts',(78.4584055093427,221.0886516733,57.4730952299792));
#39095=CARTESIAN_POINT('Ctrl Pts',(77.1107450994171,220.895866850698,58.5240383502307));
#39096=CARTESIAN_POINT('Ctrl Pts',(75.2702256751613,220.703082028095,58.9126397065623));
#39097=CARTESIAN_POINT('Ctrl Pts',(73.6127451627033,220.510297205493,58.496192382995));
#39098=CARTESIAN_POINT('Ctrl Pts',(71.9552646502452,220.31751238289,58.0797450594277));
#39099=CARTESIAN_POINT('Ctrl Pts',(70.5170033810726,220.124727560288,56.867339480917));
#39100=CARTESIAN_POINT('Ctrl Pts',(69.8261371496122,219.931942737686,55.3042099684606));
#39101=CARTESIAN_POINT('Ctrl Pts',(69.1352709181517,219.739157915083,53.7410804560042));
#39102=CARTESIAN_POINT('Ctrl Pts',(69.2068803054902,219.546373092481,51.8613477992546));
#39103=CARTESIAN_POINT('Ctrl Pts',(70.0146680415442,219.353588269878,50.3553102844611));
#39104=CARTESIAN_POINT('Ctrl Pts',(70.8224557775982,219.160803447276,48.8492727696676));
#39105=CARTESIAN_POINT('Ctrl Pts',(72.3487890589396,218.968018624674,47.7498049531877));
#39106=CARTESIAN_POINT('Ctrl Pts',(74.0331492157609,218.775233802071,47.4606667775732));
#39107=CARTESIAN_POINT('Ctrl Pts',(75.7175093725821,218.582448979469,47.1715286019587));
#39108=CARTESIAN_POINT('Ctrl Pts',(77.5231293307847,218.389664156867,47.6990315230373));
#39109=CARTESIAN_POINT('Ctrl Pts',(78.7869273705882,218.196879334264,48.8494595029966));
#39110=CARTESIAN_POINT('Ctrl Pts',(79.9447859852115,218.020254936545,49.9034514424892));
#39111=CARTESIAN_POINT('Ctrl Pts',(80.6314498948667,217.843630538826,51.4570729301857));
#39112=CARTESIAN_POINT('Ctrl Pts',(80.6314498948689,217.667006141107,53.0228109606278));
#39113=CARTESIAN_POINT('Ctrl Pts',(80.6215141333136,220.332993858894,53.0207205529598));
#39114=CARTESIAN_POINT('Ctrl Pts',(80.6163399326053,220.202897648442,54.1772185397082));
#39115=CARTESIAN_POINT('Ctrl Pts',(79.7114181348351,219.860645428437,57.2260257613491));
#39116=CARTESIAN_POINT('Ctrl Pts',(74.7044349299368,219.306237198879,59.6939299756169));
#39117=CARTESIAN_POINT('Ctrl Pts',(69.2276352050903,218.669769170223,56.3901794069435));
#39118=CARTESIAN_POINT('Ctrl Pts',(69.0357866029293,218.033301141565,49.9969717623945));
#39119=CARTESIAN_POINT('Ctrl Pts',(74.3245562273971,217.396833112908,46.3781728935986));
#39120=CARTESIAN_POINT('Ctrl Pts',(79.2251026994422,216.866443089028,48.4600028300045));
#39121=CARTESIAN_POINT('Ctrl Pts',(80.5151970792007,216.511830004356,51.4368566165362));
#39122=CARTESIAN_POINT('Ctrl Pts',(80.6277153321941,216.369372929237,52.702997681211));
#39123=CARTESIAN_POINT('Ctrl Pts',(80.6293939811109,216.332993858894,53.0260232150293));
#39124=CARTESIAN_POINT('Origin',(74.9879498948689,423.667006141107,53.0228109606356));
#39125=CARTESIAN_POINT('',(80.6407963231499,225.667006141107,53.0222595369741));
#39126=CARTESIAN_POINT('',(80.6389234508925,224.332993858894,53.0179829901466));
#39127=CARTESIAN_POINT('',(80.6314498948689,423.667006141107,53.0228109606222));
#39128=CARTESIAN_POINT('Ctrl Pts',(80.6407963231499,225.667006141107,53.0222595369741));
#39129=CARTESIAN_POINT('Ctrl Pts',(80.6334465165095,225.46453456171,54.8079251578411));
#39130=CARTESIAN_POINT('Ctrl Pts',(79.2294387037549,225.155984977538,57.533499672276));
#39131=CARTESIAN_POINT('Ctrl Pts',(75.6715948746436,224.741357388588,58.8497648206672));
#39132=CARTESIAN_POINT('Ctrl Pts',(71.8177424321106,224.317045369484,58.3820796919963));
#39133=CARTESIAN_POINT('Ctrl Pts',(68.4288418723472,223.786655345603,54.2755576487171));
#39134=CARTESIAN_POINT('Ctrl Pts',(70.395023167623,223.150187316946,48.1762408565892));
#39135=CARTESIAN_POINT('Ctrl Pts',(76.5790555611666,222.513719288289,46.5429470970313));
#39136=CARTESIAN_POINT('Ctrl Pts',(80.2487384158096,222.01932556301,49.8922375528076));
#39137=CARTESIAN_POINT('Ctrl Pts',(80.6309179385296,221.737087847282,52.3955344152688));
#39138=CARTESIAN_POINT('Ctrl Pts',(80.626235952703,221.667006141107,53.0185107809476));
#39139=CARTESIAN_POINT('Ctrl Pts',(80.6389234508925,224.332993858894,53.0179829901465));
#39140=CARTESIAN_POINT('Ctrl Pts',(80.6274057020489,224.142500372422,54.7003984290927));
#39141=CARTESIAN_POINT('Ctrl Pts',(78.9338615869445,223.739850876398,58.2827370241048));
#39142=CARTESIAN_POINT('Ctrl Pts',(72.8470130986032,223.125045370821,59.3423554510688));
#39143=CARTESIAN_POINT('Ctrl Pts',(68.5099388049065,222.488577342164,54.6413249332986));
#39144=CARTESIAN_POINT('Ctrl Pts',(70.1300482334095,221.852109313507,48.4411008882662));
#39145=CARTESIAN_POINT('Ctrl Pts',(75.1949720228243,221.321719289626,46.7995385915325));
#39146=CARTESIAN_POINT('Ctrl Pts',(78.6962367276934,220.897407270522,48.4764536776389));
#39147=CARTESIAN_POINT('Ctrl Pts',(80.3232136734672,220.60319146187,50.620979749766));
#39148=CARTESIAN_POINT('Ctrl Pts',(80.6247778246167,220.415053657994,52.2912450968989));
#39149=CARTESIAN_POINT('Ctrl Pts',(80.6215141333136,220.332993858894,53.0207205529598));
#39150=CARTESIAN_POINT('Origin',(74.9879498948689,423.667006141107,53.0228109606356));
#39151=CARTESIAN_POINT('',(80.6280038580037,229.667006141107,53.0272789318033));
#39152=CARTESIAN_POINT('',(80.6344810375604,228.332993858894,53.0280828052492));
#39153=CARTESIAN_POINT('',(80.6314498948689,423.667006141107,53.0228109606222));
#39154=CARTESIAN_POINT('Ctrl Pts',(80.6280038580037,229.667006141107,53.0272789318033));
#39155=CARTESIAN_POINT('Ctrl Pts',(80.6320769718372,229.616293295243,53.4768962186168));
#39156=CARTESIAN_POINT('Ctrl Pts',(80.4807879632803,229.459502444603,54.8647393944588));
#39157=CARTESIAN_POINT('Ctrl Pts',(79.3249956567615,229.196633589187,56.973860923079));
#39158=CARTESIAN_POINT('Ctrl Pts',(76.1086729866622,228.772321570083,59.1478380087876));
#39159=CARTESIAN_POINT('Ctrl Pts',(70.8573012407579,228.241931546201,58.2696208856052));
#39160=CARTESIAN_POINT('Ctrl Pts',(68.3422715097577,227.605463517545,52.3753728345039));
#39161=CARTESIAN_POINT('Ctrl Pts',(71.9402036438859,226.968995488888,47.087198498792));
#39162=CARTESIAN_POINT('Ctrl Pts',(78.3343475963114,226.332527460231,47.2447628702198));
#39163=CARTESIAN_POINT('Ctrl Pts',(80.6013028412971,225.89853101097,50.9805133951161));
#39164=CARTESIAN_POINT('Ctrl Pts',(80.6411478721884,225.676690571263,52.9368492584648));
#39165=CARTESIAN_POINT('Ctrl Pts',(80.6407963231499,225.667006141107,53.0222595369741));
#39166=CARTESIAN_POINT('Ctrl Pts',(80.6344810375604,228.332993858894,53.0280828052492));
#39167=CARTESIAN_POINT('Ctrl Pts',(80.6376880979176,228.294259105955,53.3711062959646));
#39168=CARTESIAN_POINT('Ctrl Pts',(80.4533246712096,228.043368343463,55.5892892119953));
#39169=CARTESIAN_POINT('Ctrl Pts',(77.5154492131354,227.58032157142,59.1979222716756));
#39170=CARTESIAN_POINT('Ctrl Pts',(71.1583728874286,226.943853542763,58.492596811605));
#39171=CARTESIAN_POINT('Ctrl Pts',(68.3158924128625,226.307385514106,52.7490927066299));
#39172=CARTESIAN_POINT('Ctrl Pts',(71.0634780017905,225.776995490225,48.1885067791575));
#39173=CARTESIAN_POINT('Ctrl Pts',(74.8065245107504,225.35268347112,47.1586958035716));
#39174=CARTESIAN_POINT('Ctrl Pts',(78.6060725394363,224.928371452016,47.955152209226));
#39175=CARTESIAN_POINT('Ctrl Pts',(80.5441433285849,224.588474914607,50.7633344776202));
#39176=CARTESIAN_POINT('Ctrl Pts',(80.6402332253356,224.354656381974,52.8266622056322));
#39177=CARTESIAN_POINT('Ctrl Pts',(80.6389234508925,224.332993858894,53.0179829901465));
#39178=CARTESIAN_POINT('Origin',(74.9879498948689,423.667006141107,53.0228109606356));
#39179=CARTESIAN_POINT('',(80.6265348678285,233.667006141107,53.0222797174675));
#39180=CARTESIAN_POINT('',(80.6223895405763,232.332993858894,53.0239051904298));
#39181=CARTESIAN_POINT('',(80.6314498948689,423.667006141107,53.0228109606222));
#39182=CARTESIAN_POINT('Ctrl Pts',(80.6265348678285,233.667006141107,53.0222797174675));
#39183=CARTESIAN_POINT('Ctrl Pts',(80.6265011449881,233.661974024,53.0670254804188));
#39184=CARTESIAN_POINT('Ctrl Pts',(80.6144193150399,233.550863902116,54.0550392157484));
#39185=CARTESIAN_POINT('Ctrl Pts',(79.8504433688653,233.227597770682,56.9123011334566));
#39186=CARTESIAN_POINT('Ctrl Pts',(75.3098000176901,232.697207746799,59.6927198950109));
#39187=CARTESIAN_POINT('Ctrl Pts',(69.5459368691264,232.060739718144,56.8917528765499));
#39188=CARTESIAN_POINT('Ctrl Pts',(68.7947633682085,231.424271689486,50.5399309481628));
#39189=CARTESIAN_POINT('Ctrl Pts',(73.7256447190361,230.78780366083,46.4660737412472));
#39190=CARTESIAN_POINT('Ctrl Pts',(79.3418961640255,230.202048478036,48.2665114230645));
#39191=CARTESIAN_POINT('Ctrl Pts',(80.6150371949788,229.828449304795,51.5959327709697));
#39192=CARTESIAN_POINT('Ctrl Pts',(80.6280038580037,229.667006141107,53.0272789318033));
#39193=CARTESIAN_POINT('Ctrl Pts',(80.6223895405763,232.332993858894,53.0239051904298));
#39194=CARTESIAN_POINT('Ctrl Pts',(80.6234035207467,232.233861829935,53.9058352652539));
#39195=CARTESIAN_POINT('Ctrl Pts',(80.0109577612122,231.922573791425,56.6733318748735));
#39196=CARTESIAN_POINT('Ctrl Pts',(75.683319836815,231.399129743361,59.6636450923455));
#39197=CARTESIAN_POINT('Ctrl Pts',(69.7710792277636,230.762661714704,57.1912079111794));
#39198=CARTESIAN_POINT('Ctrl Pts',(68.8549962387284,230.232271690823,51.9463092001141));
#39199=CARTESIAN_POINT('Ctrl Pts',(71.0057109233227,229.807959671719,48.71438496963));
#39200=CARTESIAN_POINT('Ctrl Pts',(74.3966183648981,229.383647652614,46.8242382530895));
#39201=CARTESIAN_POINT('Ctrl Pts',(79.1767330987352,228.891992381673,48.052771871417));
#39202=CARTESIAN_POINT('Ctrl Pts',(80.6201225508014,228.506415115507,51.4923155602383));
#39203=CARTESIAN_POINT('Ctrl Pts',(80.6344810375604,228.332993858894,53.0280828052492));
#39204=CARTESIAN_POINT('Origin',(74.9879498948689,423.667006141107,53.0228109606356));
#39205=CARTESIAN_POINT('',(80.6306964515364,237.667006141107,53.0183537100148));
#39206=CARTESIAN_POINT('',(80.6301424893571,236.332993858894,53.0176985262882));
#39207=CARTESIAN_POINT('',(80.6314498948689,423.667006141107,53.0228109606222));
#39208=CARTESIAN_POINT('Ctrl Pts',(80.6306964515364,237.667006141107,53.0183537100148));
#39209=CARTESIAN_POINT('Ctrl Pts',(80.6164849814828,237.495498743204,54.5372715917522));
#39210=CARTESIAN_POINT('Ctrl Pts',(79.2093644293768,237.111835335749,57.9538528736901));
#39211=CARTESIAN_POINT('Ctrl Pts',(73.4162169892982,236.516015918742,59.5123312044275));
#39212=CARTESIAN_POINT('Ctrl Pts',(68.6840167868883,235.879547890085,55.2092875510666));
#39213=CARTESIAN_POINT('Ctrl Pts',(69.735477959311,235.243079861428,48.9002200414177));
#39214=CARTESIAN_POINT('Ctrl Pts',(75.6256505593195,234.60661183277,46.3756604014124));
#39215=CARTESIAN_POINT('Ctrl Pts',(79.987591280419,234.081253925998,49.3398271333882));
#39216=CARTESIAN_POINT('Ctrl Pts',(80.6272120290057,233.768052028776,52.1237761173741));
#39217=CARTESIAN_POINT('Ctrl Pts',(80.6265348678285,233.667006141107,53.0222797174675));
#39218=CARTESIAN_POINT('Ctrl Pts',(80.6301424893571,236.332993858894,53.0176985262882));
#39219=CARTESIAN_POINT('Ctrl Pts',(80.6177952448289,236.173464553916,54.431871326041));
#39220=CARTESIAN_POINT('Ctrl Pts',(79.3643926740058,235.801779239385,57.7468592758642));
#39221=CARTESIAN_POINT('Ctrl Pts',(73.7825598716915,235.217937915303,59.5907868730799));
#39222=CARTESIAN_POINT('Ctrl Pts',(69.6516937528243,234.687547891422,56.2316030971915));
#39223=CARTESIAN_POINT('Ctrl Pts',(69.1562151927476,234.263235872318,52.3812253387187));
#39224=CARTESIAN_POINT('Ctrl Pts',(70.4769197368907,233.838923853213,48.7306572468295));
#39225=CARTESIAN_POINT('Ctrl Pts',(75.2392757088466,233.308533829332,46.3498724752568));
#39226=CARTESIAN_POINT('Ctrl Pts',(79.8846817431793,232.771197829634,49.1231713686024));
#39227=CARTESIAN_POINT('Ctrl Pts',(80.6212334654278,232.446017839488,52.018385090529));
#39228=CARTESIAN_POINT('Ctrl Pts',(80.6223895405763,232.332993858894,53.0239051904298));
#39229=CARTESIAN_POINT('Origin',(74.9879498948689,423.667006141107,53.0228109606356));
#39230=CARTESIAN_POINT('',(80.639219222663,241.667006141107,53.0250766137249));
#39231=CARTESIAN_POINT('',(80.6409723448486,240.332993858894,53.0233040863504));
#39232=CARTESIAN_POINT('',(80.6314498948689,423.667006141107,53.0228109606222));
#39233=CARTESIAN_POINT('Ctrl Pts',(80.6392192226631,241.667006141107,53.0250766137249));
#39234=CARTESIAN_POINT('Ctrl Pts',(80.6404467163709,241.647257476737,53.1993468669158));
#39235=CARTESIAN_POINT('Ctrl Pts',(80.554786019131,241.415352802815,55.2448933528202));
#39236=CARTESIAN_POINT('Ctrl Pts',(78.0566544293302,240.97129211934,58.9530107718744));
#39237=CARTESIAN_POINT('Ctrl Pts',(71.6622303016729,240.334824090684,58.8072592228149));
#39238=CARTESIAN_POINT('Ctrl Pts',(68.3190498381245,239.698356062027,53.3544573901267));
#39239=CARTESIAN_POINT('Ctrl Pts',(71.1106908750382,239.06188803337,47.586071571299));
#39240=CARTESIAN_POINT('Ctrl Pts',(76.3977930505111,238.531498009489,46.9578032223369));
#39241=CARTESIAN_POINT('Ctrl Pts',(79.507433526864,238.107185990384,49.2818178510052));
#39242=CARTESIAN_POINT('Ctrl Pts',(80.5215624825551,237.854381369182,51.3606053507983));
#39243=CARTESIAN_POINT('Ctrl Pts',(80.6340646824947,237.707654752757,52.6583581421423));
#39244=CARTESIAN_POINT('Ctrl Pts',(80.6306964515364,237.667006141107,53.0183537100148));
#39245=CARTESIAN_POINT('Ctrl Pts',(80.6409723448486,240.332993858894,53.0233040863504));
#39246=CARTESIAN_POINT('Ctrl Pts',(80.6411761736531,240.325223287449,53.091891390677));
#39247=CARTESIAN_POINT('Ctrl Pts',(80.6087082900944,240.105296706451,55.0329578157609));
#39248=CARTESIAN_POINT('Ctrl Pts',(78.3846879127202,239.673214115902,58.7720233877865));
#39249=CARTESIAN_POINT('Ctrl Pts',(73.0631846035857,239.14282409202,58.9445721144314));
#39250=CARTESIAN_POINT('Ctrl Pts',(70.1642998769843,238.718512072917,56.3624460082323));
#39251=CARTESIAN_POINT('Ctrl Pts',(68.7676494101067,238.294200053811,52.740253942672));
#39252=CARTESIAN_POINT('Ctrl Pts',(70.8020690104725,237.763810029931,47.8199584818442));
#39253=CARTESIAN_POINT('Ctrl Pts',(77.1104133983672,237.127342001273,46.6919843165582));
#39254=CARTESIAN_POINT('Ctrl Pts',(80.3669121402635,236.650403277595,50.2087018539011));
#39255=CARTESIAN_POINT('Ctrl Pts',(80.6342156895141,236.385620563468,52.5511807654309));
#39256=CARTESIAN_POINT('Ctrl Pts',(80.6301424893571,236.332993858894,53.0176985262882));
#39257=CARTESIAN_POINT('Origin',(74.9879498948689,423.667006141107,53.0228109606356));
#39258=CARTESIAN_POINT('',(80.6314498948689,245.667006141107,53.022810960629));
#39259=CARTESIAN_POINT('',(80.6268649774404,244.332993858894,53.0288741209513));
#39260=CARTESIAN_POINT('',(80.6314498948689,423.667006141107,53.0228109606222));
#39261=CARTESIAN_POINT('Ctrl Pts',(80.6242644646922,245.667006141107,53.0259519424172));
#39262=CARTESIAN_POINT('Ctrl Pts',(80.6283838704355,245.586860200718,53.7390185694659));
#39263=CARTESIAN_POINT('Ctrl Pts',(80.1722574471451,245.294558250776,56.3347096625558));
#39264=CARTESIAN_POINT('Ctrl Pts',(76.2700637597904,244.790100291282,59.5708210818689));
#39265=CARTESIAN_POINT('Ctrl Pts',(70.1704175211297,244.153632262625,57.6461862589446));
#39266=CARTESIAN_POINT('Ctrl Pts',(68.4956083292596,243.517164233968,51.4605133929858));
#39267=CARTESIAN_POINT('Ctrl Pts',(72.0753836691866,242.986774210088,47.5192725924447));
#39268=CARTESIAN_POINT('Ctrl Pts',(75.9470751017479,242.562462190983,47.234819894324));
#39269=CARTESIAN_POINT('Ctrl Pts',(79.3537682695749,242.157898836248,48.6822702297702));
#39270=CARTESIAN_POINT('Ctrl Pts',(80.627259993364,241.859413486289,51.3271958794769));
#39271=CARTESIAN_POINT('Ctrl Pts',(80.6392192226631,241.667006141107,53.0250766137249));
#39272=CARTESIAN_POINT('Ctrl Pts',(80.6268649774404,244.332993858894,53.0288741209513));
#39273=CARTESIAN_POINT('Ctrl Pts',(80.6315087751579,244.264826011429,53.6345321579813));
#39274=CARTESIAN_POINT('Ctrl Pts',(80.2623979033779,243.984502154412,56.11878604849));
#39275=CARTESIAN_POINT('Ctrl Pts',(77.4178204841707,243.598100292619,58.7558472860377));
#39276=CARTESIAN_POINT('Ctrl Pts',(73.5359982239256,243.173788273515,58.7072280891914));
#39277=CARTESIAN_POINT('Ctrl Pts',(70.1063587579266,242.74947625441,56.8883050507697));
#39278=CARTESIAN_POINT('Ctrl Pts',(68.415965773611,242.21908623053,51.8394693344116));
#39279=CARTESIAN_POINT('Ctrl Pts',(72.4391053296256,241.582618201872,46.8512950444875));
#39280=CARTESIAN_POINT('Ctrl Pts',(78.719845174171,240.953920744661,47.5364073786828));
#39281=CARTESIAN_POINT('Ctrl Pts',(80.6356111381715,240.537379297001,51.2192866672693));
#39282=CARTESIAN_POINT('Ctrl Pts',(80.6409723448486,240.332993858894,53.0233040863504));
#39283=CARTESIAN_POINT('Origin',(74.9879498948689,423.667006141107,53.0228109606356));
#39284=CARTESIAN_POINT('',(80.6314498948689,249.667006141107,53.0228109606291));
#39285=CARTESIAN_POINT('',(80.6227681821118,248.332993858894,53.0188409701825));
#39286=CARTESIAN_POINT('',(80.6314498948689,423.667006141107,53.0228109606222));
#39287=CARTESIAN_POINT('Ctrl Pts',(80.6314498948689,249.667006141107,53.0228109606291));
#39288=CARTESIAN_POINT('Ctrl Pts',(80.6314498948709,249.474221318505,54.7318077489481));
#39289=CARTESIAN_POINT('Ctrl Pts',(79.8060659192675,249.281436495902,56.4221521097287));
#39290=CARTESIAN_POINT('Ctrl Pts',(78.4584055093417,249.0886516733,57.4730952299799));
#39291=CARTESIAN_POINT('Ctrl Pts',(77.110745099416,248.895866850697,58.5240383502311));
#39292=CARTESIAN_POINT('Ctrl Pts',(75.2702256751601,248.703082028095,58.9126397065624));
#39293=CARTESIAN_POINT('Ctrl Pts',(73.6127451627021,248.510297205493,58.4961923829947));
#39294=CARTESIAN_POINT('Ctrl Pts',(71.9552646502442,248.31751238289,58.079745059427));
#39295=CARTESIAN_POINT('Ctrl Pts',(70.5170033810718,248.124727560288,56.8673394809161));
#39296=CARTESIAN_POINT('Ctrl Pts',(69.8261371496117,247.931942737685,55.3042099684595));
#39297=CARTESIAN_POINT('Ctrl Pts',(69.1352709181516,247.739157915083,53.741080456003));
#39298=CARTESIAN_POINT('Ctrl Pts',(69.2068803054904,247.546373092481,51.8613477992534));
#39299=CARTESIAN_POINT('Ctrl Pts',(70.0146680415447,247.353588269878,50.3553102844601));
#39300=CARTESIAN_POINT('Ctrl Pts',(70.8224557775991,247.160803447276,48.8492727696668));
#39301=CARTESIAN_POINT('Ctrl Pts',(72.3487890589407,246.968018624674,47.7498049531871));
#39302=CARTESIAN_POINT('Ctrl Pts',(74.0331492157621,246.775233802071,47.460666777573));
#39303=CARTESIAN_POINT('Ctrl Pts',(75.7175093725834,246.582448979469,47.1715286019588));
#39304=CARTESIAN_POINT('Ctrl Pts',(77.5231293307858,246.389664156866,47.6990315230378));
#39305=CARTESIAN_POINT('Ctrl Pts',(78.7869273705891,246.196879334264,48.8494595029974));
#39306=CARTESIAN_POINT('Ctrl Pts',(79.9447859852121,246.020254936545,49.9034514424903));
#39307=CARTESIAN_POINT('Ctrl Pts',(80.6314498948671,245.843630538826,51.4570729301869));
#39308=CARTESIAN_POINT('Ctrl Pts',(80.6314498948689,245.667006141107,53.022810960629));
#39309=CARTESIAN_POINT('Ctrl Pts',(80.6227681821118,248.332993858894,53.0188409701825));
#39310=CARTESIAN_POINT('Ctrl Pts',(80.6158591604151,248.20442873541,54.1611132958689));
#39311=CARTESIAN_POINT('Ctrl Pts',(79.9981558131614,247.96978560715,56.2521292880647));
#39312=CARTESIAN_POINT('Ctrl Pts',(77.6191604611375,247.629064474113,58.2666161345652));
#39313=CARTESIAN_POINT('Ctrl Pts',(73.8370732189359,247.204752455009,59.1422438972669));
#39314=CARTESIAN_POINT('Ctrl Pts',(69.2501690271641,246.674362431128,56.4388237546138));
#39315=CARTESIAN_POINT('Ctrl Pts',(69.0167443893414,246.037894402471,50.0346807540015));
#39316=CARTESIAN_POINT('Ctrl Pts',(74.2720958288138,245.401426373814,46.3889730468402));
#39317=CARTESIAN_POINT('Ctrl Pts',(79.5510126640985,244.833126192622,48.5682043349156));
#39318=CARTESIAN_POINT('Ctrl Pts',(80.6170560730475,244.476982020982,51.7495673678552));
#39319=CARTESIAN_POINT('Ctrl Pts',(80.6268649774404,244.332993858894,53.0288741209513));
#39320=CARTESIAN_POINT('Origin',(74.9879498948689,423.667006141107,53.0228109606356));
#39321=CARTESIAN_POINT('',(80.6393328775357,253.667006141107,53.0210292745041));
#39322=CARTESIAN_POINT('',(80.6374739721345,252.332993858894,53.0206546444271));
#39323=CARTESIAN_POINT('',(80.6314498948689,423.667006141107,53.0228109606222));
#39324=CARTESIAN_POINT('Ctrl Pts',(80.6393328775358,253.667006141107,53.0210292745041));
#39325=CARTESIAN_POINT('Ctrl Pts',(80.6320814513646,253.466065648679,54.7946984432943));
#39326=CARTESIAN_POINT('Ctrl Pts',(78.779047218355,253.052969146698,58.4542935954325));
#39327=CARTESIAN_POINT('Ctrl Pts',(72.531846601885,252.427716635165,59.2323865748476));
#39328=CARTESIAN_POINT('Ctrl Pts',(69.1307639245367,251.897326611285,55.1359482250076));
#39329=CARTESIAN_POINT('Ctrl Pts',(69.3913142509957,251.47301459218,51.2625748355938));
#39330=CARTESIAN_POINT('Ctrl Pts',(71.3948305414538,251.048702573075,47.9373935833451));
#39331=CARTESIAN_POINT('Ctrl Pts',(76.5284508786805,250.518312549195,46.5252630067303));
#39332=CARTESIAN_POINT('Ctrl Pts',(80.2381453491283,250.022387736946,49.8676147702881));
#39333=CARTESIAN_POINT('Ctrl Pts',(80.6311954971923,249.738618934251,52.3828494633525));
#39334=CARTESIAN_POINT('Ctrl Pts',(80.6264700991543,249.667006141107,53.0189018164475));
#39335=CARTESIAN_POINT('Ctrl Pts',(80.6374739721345,252.332993858894,53.0206546444271));
#39336=CARTESIAN_POINT('Ctrl Pts',(80.6341057873527,252.250109464167,53.7534226942952));
#39337=CARTESIAN_POINT('Ctrl Pts',(80.2883165046266,252.061147064663,55.4282110155384));
#39338=CARTESIAN_POINT('Ctrl Pts',(78.1317232526417,251.660028655607,58.3976286937398));
#39339=CARTESIAN_POINT('Ctrl Pts',(72.8959148267621,251.129638631727,59.3643140922468));
#39340=CARTESIAN_POINT('Ctrl Pts',(68.5203052848772,250.493170603069,54.6822658470019));
#39341=CARTESIAN_POINT('Ctrl Pts',(70.0974900542959,249.856702574413,48.4836860385676));
#39342=CARTESIAN_POINT('Ctrl Pts',(76.1615187036544,249.220234545756,46.4496113157072));
#39343=CARTESIAN_POINT('Ctrl Pts',(80.1472802315439,248.712331640583,49.6536433732334));
#39344=CARTESIAN_POINT('Ctrl Pts',(80.6272603120911,248.416584744962,52.276154670448));
#39345=CARTESIAN_POINT('Ctrl Pts',(80.6227681821118,248.332993858894,53.0188409701825));
#39346=CARTESIAN_POINT('Origin',(74.9879498948689,423.667006141107,53.0228109606356));
#39347=CARTESIAN_POINT('',(80.6321203983526,257.667006141107,53.0274094678416));
#39348=CARTESIAN_POINT('',(80.6352358645235,256.332993858894,53.0260672585175));
#39349=CARTESIAN_POINT('',(80.6314498948689,423.667006141107,53.0228109606222));
#39350=CARTESIAN_POINT('Ctrl Pts',(80.6321203983526,257.667006141107,53.0274094678416));
#39351=CARTESIAN_POINT('Ctrl Pts',(80.6362361148136,257.617824382212,53.4631731254976));
#39352=CARTESIAN_POINT('Ctrl Pts',(80.3908316677195,257.356486613764,55.774500525636));
#39353=CARTESIAN_POINT('Ctrl Pts',(77.2053896188859,256.882992835764,59.321559547837));
#39354=CARTESIAN_POINT('Ctrl Pts',(71.9514325914311,256.352602811883,58.458943708744));
#39355=CARTESIAN_POINT('Ctrl Pts',(69.608268828627,255.928290792779,55.3637068087443));
#39356=CARTESIAN_POINT('Ctrl Pts',(68.9405046437633,255.503978773674,51.5394423200026));
#39357=CARTESIAN_POINT('Ctrl Pts',(71.8904013482855,254.973588749793,47.1070298882851));
#39358=CARTESIAN_POINT('Ctrl Pts',(78.2977346304908,254.337120721136,47.2237125544275));
#39359=CARTESIAN_POINT('Ctrl Pts',(80.5923227223968,253.901593184907,50.9507676211459));
#39360=CARTESIAN_POINT('Ctrl Pts',(80.639737616737,253.678221658231,52.9220317220709));
#39361=CARTESIAN_POINT('Ctrl Pts',(80.6393328775358,253.667006141107,53.0210292745041));
#39362=CARTESIAN_POINT('Ctrl Pts',(80.6352358645235,256.332993858894,53.0260672585175));
#39363=CARTESIAN_POINT('Ctrl Pts',(80.6372806134956,256.295790192923,53.3554066374292));
#39364=CARTESIAN_POINT('Ctrl Pts',(80.4548977293209,256.0464305174,55.5599296850919));
#39365=CARTESIAN_POINT('Ctrl Pts',(77.5667687190911,255.584914832326,59.1824348262834));
#39366=CARTESIAN_POINT('Ctrl Pts',(71.193045766207,254.948446803668,58.5167093921053));
#39367=CARTESIAN_POINT('Ctrl Pts',(68.3192351039939,254.311978775012,52.8025939123332));
#39368=CARTESIAN_POINT('Ctrl Pts',(71.5637615965536,253.675510746354,47.2905206837289));
#39369=CARTESIAN_POINT('Ctrl Pts',(77.9675186861103,253.039042717698,47.0467384616874));
#39370=CARTESIAN_POINT('Ctrl Pts',(80.5301405732545,252.591537088544,50.7363783348355));
#39371=CARTESIAN_POINT('Ctrl Pts',(80.6384164941214,252.356187468943,52.8156035433032));
#39372=CARTESIAN_POINT('Ctrl Pts',(80.6374739721345,252.332993858894,53.0206546444271));
#39373=CARTESIAN_POINT('Origin',(74.9879498948689,423.667006141107,53.0228109606356));
#39374=CARTESIAN_POINT('',(80.622068675635,261.667006141107,53.0231071599436));
#39375=CARTESIAN_POINT('',(80.6208495127526,260.332993858894,53.0251315510043));
#39376=CARTESIAN_POINT('',(80.6314498948689,423.667006141107,53.0228109606222));
#39377=CARTESIAN_POINT('Ctrl Pts',(80.6220686756351,261.667006141107,53.0231071599436));
#39378=CARTESIAN_POINT('Ctrl Pts',(80.6212211316863,261.557427106192,53.9989613352296));
#39379=CARTESIAN_POINT('Ctrl Pts',(79.9158201063165,261.235692061725,56.8646493578844));
#39380=CARTESIAN_POINT('Ctrl Pts',(76.2600105715705,260.807879012482,59.1182057980456));
#39381=CARTESIAN_POINT('Ctrl Pts',(72.4612951821995,260.383566993377,58.317787609226));
#39382=CARTESIAN_POINT('Ctrl Pts',(69.4494584547942,259.959254974273,55.8683494259096));
#39383=CARTESIAN_POINT('Ctrl Pts',(68.7701667585371,259.428864950391,50.5875603443804));
#39384=CARTESIAN_POINT('Ctrl Pts',(73.6841987474315,258.792396921735,46.4741889478306));
#39385=CARTESIAN_POINT('Ctrl Pts',(79.3157785783291,258.205110651973,48.2397007920277));
#39386=CARTESIAN_POINT('Ctrl Pts',(80.6184820938021,257.829980391764,51.5834136213084));
#39387=CARTESIAN_POINT('Ctrl Pts',(80.6321203983526,257.667006141107,53.0274094678416));
#39388=CARTESIAN_POINT('Ctrl Pts',(80.6208495127526,260.332993858894,53.0251315510043));
#39389=CARTESIAN_POINT('Ctrl Pts',(80.6234734375329,260.235392916904,53.8929902989329));
#39390=CARTESIAN_POINT('Ctrl Pts',(80.0293014250823,259.925635965362,56.6440798635399));
#39391=CARTESIAN_POINT('Ctrl Pts',(75.7253090599096,259.403723004267,59.6591140566951));
#39392=CARTESIAN_POINT('Ctrl Pts',(69.8086851766418,258.76725497561,57.2294092881355));
#39393=CARTESIAN_POINT('Ctrl Pts',(68.64387461178,258.130786946953,50.9402821796723));
#39394=CARTESIAN_POINT('Ctrl Pts',(73.3188397393547,257.494318918296,46.5571057413125));
#39395=CARTESIAN_POINT('Ctrl Pts',(78.4794664963865,256.963928894415,47.8671065072692));
#39396=CARTESIAN_POINT('Ctrl Pts',(80.3671424458033,256.576820541282,50.8638740355873));
#39397=CARTESIAN_POINT('Ctrl Pts',(80.6314504651601,256.4018681977,52.4163684190792));
#39398=CARTESIAN_POINT('Ctrl Pts',(80.6352358645235,256.332993858894,53.0260672585175));
#39399=CARTESIAN_POINT('Origin',(74.9879498948689,423.667006141107,53.0228109606356));
#39400=CARTESIAN_POINT('',(80.6335139906277,265.667006141107,53.0179319616114));
#39401=CARTESIAN_POINT('',(80.6304551573619,264.332993858894,53.0160315296102));
#39402=CARTESIAN_POINT('',(80.6314498948689,423.667006141107,53.0228109606222));
#39403=CARTESIAN_POINT('Ctrl Pts',(80.6335139906277,265.667006141107,53.0179319616114));
#39404=CARTESIAN_POINT('Ctrl Pts',(80.6183865584892,265.497029830172,54.5213633042316));
#39405=CARTESIAN_POINT('Ctrl Pts',(79.6079955865199,265.220975514462,56.9782353383759));
#39406=CARTESIAN_POINT('Ctrl Pts',(76.5523955207542,264.838843193976,58.677302240125));
#39407=CARTESIAN_POINT('Ctrl Pts',(72.6723019530944,264.414531174871,58.8029278451709));
#39408=CARTESIAN_POINT('Ctrl Pts',(68.6966783295341,263.88414115099,55.2613763015696));
#39409=CARTESIAN_POINT('Ctrl Pts',(69.7095077253019,263.247673122334,48.9335242766798));
#39410=CARTESIAN_POINT('Ctrl Pts',(75.5720466440224,262.611205093676,46.3760761608992));
#39411=CARTESIAN_POINT('Ctrl Pts',(79.9816199514584,262.084316099935,49.3072022180086));
#39412=CARTESIAN_POINT('Ctrl Pts',(80.6228620618353,261.769583115745,52.1096097097592));
#39413=CARTESIAN_POINT('Ctrl Pts',(80.6220686756351,261.667006141107,53.0231071599436));
#39414=CARTESIAN_POINT('Ctrl Pts',(80.6304551573619,264.332993858894,53.0160315296102));
#39415=CARTESIAN_POINT('Ctrl Pts',(80.6177187628455,264.174995640884,54.417397186382));
#39416=CARTESIAN_POINT('Ctrl Pts',(79.3805880254645,263.804841413322,57.7237302943176));
#39417=CARTESIAN_POINT('Ctrl Pts',(73.83600196959,263.222531176209,59.5949695472677));
#39418=CARTESIAN_POINT('Ctrl Pts',(68.8326175982397,262.586063147551,55.6104936380737));
#39419=CARTESIAN_POINT('Ctrl Pts',(69.4880334727284,261.949595118895,49.2357022951904));
#39420=CARTESIAN_POINT('Ctrl Pts',(74.2432971283764,261.419205095013,46.8407830695233));
#39421=CARTESIAN_POINT('Ctrl Pts',(77.959377089695,260.994893075909,47.9640183999525));
#39422=CARTESIAN_POINT('Ctrl Pts',(80.1081444486407,260.668181998794,50.0419592388654));
#39423=CARTESIAN_POINT('Ctrl Pts',(80.6177697896028,260.447548926456,52.0065182520312));
#39424=CARTESIAN_POINT('Ctrl Pts',(80.6208495127526,260.332993858894,53.0251315510043));
#39425=CARTESIAN_POINT('Origin',(74.9879498948689,423.667006141107,53.0228109606356));
#39426=CARTESIAN_POINT('',(80.6362260843705,269.667006141107,53.025791082417));
#39427=CARTESIAN_POINT('',(80.6409957355089,268.332993858894,53.0245822494549));
#39428=CARTESIAN_POINT('',(80.6314498948689,423.667006141107,53.0228109606222));
#39429=CARTESIAN_POINT('Ctrl Pts',(80.6362260843705,269.667006141107,53.025791082417));
#39430=CARTESIAN_POINT('Ctrl Pts',(80.6373722385248,269.648788563706,53.1867844897909));
#39431=CARTESIAN_POINT('Ctrl Pts',(80.5960317434328,269.524492981528,54.2848165324738));
#39432=CARTESIAN_POINT('Ctrl Pts',(79.8769093444932,269.294119394574,56.2660866575358));
#39433=CARTESIAN_POINT('Ctrl Pts',(77.0298250182992,268.86980737547,58.9052188493705));
#39434=CARTESIAN_POINT('Ctrl Pts',(71.7059457747086,268.339417351589,58.8382835682292));
#39435=CARTESIAN_POINT('Ctrl Pts',(68.3212808918114,267.702949322932,53.396631405116));
#39436=CARTESIAN_POINT('Ctrl Pts',(71.0704926838037,267.066481294275,47.6215350456437));
#39437=CARTESIAN_POINT('Ctrl Pts',(77.413848888673,266.430013265619,46.8019403308202));
#39438=CARTESIAN_POINT('Ctrl Pts',(80.4345171486351,265.963521547895,50.3987411432354));
#39439=CARTESIAN_POINT('Ctrl Pts',(80.637267869771,265.709185839725,52.6448547923503));
#39440=CARTESIAN_POINT('Ctrl Pts',(80.6335139906277,265.667006141107,53.0179319616114));
#39441=CARTESIAN_POINT('Ctrl Pts',(80.6409957355089,268.332993858894,53.0245822494549));
#39442=CARTESIAN_POINT('Ctrl Pts',(80.6411428885357,268.326754374417,53.0796608730736));
#39443=CARTESIAN_POINT('Ctrl Pts',(80.6157117197006,268.108358880388,55.0073374956178));
#39444=CARTESIAN_POINT('Ctrl Pts',(78.4277792530005,267.677807376808,58.7401378270421));
#39445=CARTESIAN_POINT('Ctrl Pts',(72.0375055083273,267.04133934815,59.0127270905129));
#39446=CARTESIAN_POINT('Ctrl Pts',(68.3522149334259,266.404871319494,53.7700018438139));
#39447=CARTESIAN_POINT('Ctrl Pts',(70.3720114990969,265.874481295612,48.8436855359119));
#39448=CARTESIAN_POINT('Ctrl Pts',(73.9141788037828,265.450169276508,47.2549883740677));
#39449=CARTESIAN_POINT('Ctrl Pts',(77.7907517378467,265.025857257403,47.4625701009125));
#39450=CARTESIAN_POINT('Ctrl Pts',(80.3585521621098,264.653465451532,50.1793413821216));
#39451=CARTESIAN_POINT('Ctrl Pts',(80.6348208711523,264.387151650437,52.535678839113));
#39452=CARTESIAN_POINT('Ctrl Pts',(80.6304551573619,264.332993858894,53.0160315296102));
#39453=CARTESIAN_POINT('Origin',(74.9879498948689,423.667006141107,53.0228109606356));
#39454=CARTESIAN_POINT('',(80.6281690978408,273.667006141107,53.0254425033022));
#39455=CARTESIAN_POINT('',(80.6267765454294,272.332993858894,53.0274331835911));
#39456=CARTESIAN_POINT('',(80.6314498948689,423.667006141107,53.0228109606222));
#39457=CARTESIAN_POINT('Ctrl Pts',(80.6281690978408,273.667006141107,53.0254425033022));
#39458=CARTESIAN_POINT('Ctrl Pts',(80.6310061674789,273.588391287686,53.723925770271));
#39459=CARTESIAN_POINT('Ctrl Pts',(80.1764188506617,273.297620424713,56.303244467039));
#39460=CARTESIAN_POINT('Ctrl Pts',(76.3234123534648,272.794693552187,59.5655789311586));
#39461=CARTESIAN_POINT('Ctrl Pts',(70.1997566345717,272.158225523531,57.6765645663912));
#39462=CARTESIAN_POINT('Ctrl Pts',(68.4885131854145,271.521757494873,51.5136472948276));
#39463=CARTESIAN_POINT('Ctrl Pts',(72.740299548083,270.885289466217,46.7353404645114));
#39464=CARTESIAN_POINT('Ctrl Pts',(78.8886131272501,270.267039014961,47.7092368751911));
#39465=CARTESIAN_POINT('Ctrl Pts',(80.6240244982427,269.860944573258,51.3119073796098));
#39466=CARTESIAN_POINT('Ctrl Pts',(80.6362260843705,269.667006141107,53.025791082417));
#39467=CARTESIAN_POINT('Ctrl Pts',(80.6267765454294,272.332993858894,53.0274331835911));
#39468=CARTESIAN_POINT('Ctrl Pts',(80.6311474818016,272.266357098398,53.6190577687339));
#39469=CARTESIAN_POINT('Ctrl Pts',(80.2718050755859,271.987564328349,56.0888874902184));
#39470=CARTESIAN_POINT('Ctrl Pts',(76.6881265535354,271.496615548749,59.4798704036303));
#39471=CARTESIAN_POINT('Ctrl Pts',(70.4679411286712,270.860147520092,57.9381739632954));
#39472=CARTESIAN_POINT('Ctrl Pts',(68.7625597545307,270.329757496211,52.8943812533468));
#39473=CARTESIAN_POINT('Ctrl Pts',(70.3951339519087,269.905445477106,49.3722214931296));
#39474=CARTESIAN_POINT('Ctrl Pts',(73.4580535169106,269.481133458002,46.9869685453763));
#39475=CARTESIAN_POINT('Ctrl Pts',(78.694248321282,268.956982918598,47.5040608083218));
#39476=CARTESIAN_POINT('Ctrl Pts',(80.6361393663569,268.53891038397,51.2068681700428));
#39477=CARTESIAN_POINT('Ctrl Pts',(80.6409957355089,268.332993858894,53.0245822494549));
#39478=CARTESIAN_POINT('Origin',(74.9879498948689,423.667006141107,53.0228109606356));
#39479=CARTESIAN_POINT('',(80.6228988645023,277.667006141107,53.0197320148476));
#39480=CARTESIAN_POINT('',(80.6235335168385,276.332993858894,53.0199012860661));
#39481=CARTESIAN_POINT('',(80.6314498948689,423.667006141107,53.0228109606222));
#39482=CARTESIAN_POINT('Ctrl Pts',(80.6228988645023,277.667006141107,53.0197320148476));
#39483=CARTESIAN_POINT('Ctrl Pts',(80.6152243194595,277.527994011667,54.2547852777675));
#39484=CARTESIAN_POINT('Ctrl Pts',(79.6128226704193,277.176825872674,57.3844444804395));
#39485=CARTESIAN_POINT('Ctrl Pts',(74.4244720439219,276.613501724129,59.6761341928656));
#39486=CARTESIAN_POINT('Ctrl Pts',(69.0912915673428,275.977033695473,56.1452576101099));
#39487=CARTESIAN_POINT('Ctrl Pts',(69.1681105982651,275.340565666815,49.7496339286456));
#39488=CARTESIAN_POINT('Ctrl Pts',(74.6042813775611,274.704097638159,46.3561722901173));
#39489=CARTESIAN_POINT('Ctrl Pts',(79.412935102352,274.173707614278,48.6420025303696));
#39490=CARTESIAN_POINT('Ctrl Pts',(80.5477416441213,273.828010448594,51.5942741654804));
#39491=CARTESIAN_POINT('Ctrl Pts',(80.6271780017631,273.694469292462,52.7814357940699));
#39492=CARTESIAN_POINT('Ctrl Pts',(80.6281690978408,273.667006141107,53.0254425033022));
#39493=CARTESIAN_POINT('Ctrl Pts',(80.6235335168385,276.332993858894,53.0199012860661));
#39494=CARTESIAN_POINT('Ctrl Pts',(80.6187897801916,276.205959822378,54.1494403880117));
#39495=CARTESIAN_POINT('Ctrl Pts',(79.7423703700239,275.86676977631,57.1728458637594));
#39496=CARTESIAN_POINT('Ctrl Pts',(74.7984951898932,275.315423720691,59.6977925792757));
#39497=CARTESIAN_POINT('Ctrl Pts',(70.2035816423413,274.78503369681,57.008008197077));
#39498=CARTESIAN_POINT('Ctrl Pts',(69.1265928622935,274.360721677705,53.2782624880387));
#39499=CARTESIAN_POINT('Ctrl Pts',(69.8750124991416,273.936409658601,49.4689612484914));
#39500=CARTESIAN_POINT('Ctrl Pts',(74.2184942159277,273.406019634719,46.389620879493));
#39501=CARTESIAN_POINT('Ctrl Pts',(79.5357846862319,272.836188366559,48.5447931610259));
#39502=CARTESIAN_POINT('Ctrl Pts',(80.6172314328848,272.47851310795,51.7354621346952));
#39503=CARTESIAN_POINT('Ctrl Pts',(80.6267765454294,272.332993858894,53.0274331835911));
#39504=CARTESIAN_POINT('Origin',(74.9879498948689,423.667006141107,53.0228109606356));
#39505=CARTESIAN_POINT('',(80.64045763597,281.667006141107,53.0193177463791));
#39506=CARTESIAN_POINT('',(80.6380317763782,280.332993858894,53.0185653928147));
#39507=CARTESIAN_POINT('',(80.6314498948689,423.667006141107,53.0228109606222));
#39508=CARTESIAN_POINT('Ctrl Pts',(80.64045763597,281.667006141107,53.0193177463791));
#39509=CARTESIAN_POINT('Ctrl Pts',(80.6324997205414,281.467596735647,54.7789712462744));
#39510=CARTESIAN_POINT('Ctrl Pts',(78.7982860972629,281.056031320635,58.432189503605));
#39511=CARTESIAN_POINT('Ctrl Pts',(72.5834632791282,280.432309896071,59.2468527844925));
#39512=CARTESIAN_POINT('Ctrl Pts',(68.4476732525639,279.795841867414,54.3678012071275));
#39513=CARTESIAN_POINT('Ctrl Pts',(70.326780909695,279.159373838757,48.2410982563761));
#39514=CARTESIAN_POINT('Ctrl Pts',(75.4561843501935,278.628983814876,46.8137262387156));
#39515=CARTESIAN_POINT('Ctrl Pts',(78.8839251560877,278.204671795772,48.6362247583429));
#39516=CARTESIAN_POINT('Ctrl Pts',(80.3728574180272,277.919371906107,50.7801947467159));
#39517=CARTESIAN_POINT('Ctrl Pts',(80.6269369725781,277.740150021219,52.3698852125657));
#39518=CARTESIAN_POINT('Ctrl Pts',(80.6228988645023,277.667006141107,53.0197320148476));
#39519=CARTESIAN_POINT('Ctrl Pts',(80.6380317763782,280.332993858894,53.0185653928147));
#39520=CARTESIAN_POINT('Ctrl Pts',(80.6252133547052,280.145562546359,54.675591025712));
#39521=CARTESIAN_POINT('Ctrl Pts',(78.9779451679485,279.745975224272,58.2324232018638));
#39522=CARTESIAN_POINT('Ctrl Pts',(73.9889689229884,279.240309897408,59.1688677132986));
#39523=CARTESIAN_POINT('Ctrl Pts',(70.7301472839238,278.815997878304,57.0591309024144));
#39524=CARTESIAN_POINT('Ctrl Pts',(68.7973374677702,278.391685859198,53.6923588428567));
#39525=CARTESIAN_POINT('Ctrl Pts',(70.0574457782005,277.861295835319,48.5193232177926));
#39526=CARTESIAN_POINT('Ctrl Pts',(76.1199198830696,277.224827806661,46.4423200012274));
#39527=CARTESIAN_POINT('Ctrl Pts',(80.1305528088605,276.71539381452,49.6241218867143));
#39528=CARTESIAN_POINT('Ctrl Pts',(80.626712162767,276.418115831931,52.2630285642579));
#39529=CARTESIAN_POINT('Ctrl Pts',(80.6235335168385,276.332993858894,53.0199012860661));
#39530=CARTESIAN_POINT('Origin',(74.9879498948689,423.667006141107,53.0228109606356));
#39531=CARTESIAN_POINT('',(80.6320072490403,285.667006141107,53.0282647722842));
#39532=CARTESIAN_POINT('',(80.6355667283407,284.332993858894,53.029097899403));
#39533=CARTESIAN_POINT('',(80.6314498948689,423.667006141107,53.0228109606222));
#39534=CARTESIAN_POINT('Ctrl Pts',(80.6320072490403,285.667006141107,53.0282647722843));
#39535=CARTESIAN_POINT('Ctrl Pts',(80.6360246717883,285.61935546918,53.4507321318154));
#39536=CARTESIAN_POINT('Ctrl Pts',(80.4001389358992,285.359548787701,55.7495394486793));
#39537=CARTESIAN_POINT('Ctrl Pts',(77.2538459713296,284.887586096669,59.2986350086054));
#39538=CARTESIAN_POINT('Ctrl Pts',(70.9320055672451,284.251118068013,58.3269162510927));
#39539=CARTESIAN_POINT('Ctrl Pts',(68.3332775512137,283.614650039355,52.4690883829723));
#39540=CARTESIAN_POINT('Ctrl Pts',(71.2699962732185,283.084260015475,48.0279338393853));
#39541=CARTESIAN_POINT('Ctrl Pts',(75.0529945743877,282.65994799637,47.1562505598691));
#39542=CARTESIAN_POINT('Ctrl Pts',(78.8157359444728,282.235635977266,48.1115961875279));
#39543=CARTESIAN_POINT('Ctrl Pts',(80.5864453672283,281.904655358845,50.9229722937909));
#39544=CARTESIAN_POINT('Ctrl Pts',(80.6409663200872,281.679752745199,52.9068375629505));
#39545=CARTESIAN_POINT('Ctrl Pts',(80.64045763597,281.667006141107,53.0193177463791));
#39546=CARTESIAN_POINT('Ctrl Pts',(80.6355667283407,284.332993858894,53.029097899403));
#39547=CARTESIAN_POINT('Ctrl Pts',(80.6383807082737,284.297321279892,53.3447008893674));
#39548=CARTESIAN_POINT('Ctrl Pts',(80.4703213599792,284.049492691337,55.5336961519382));
#39549=CARTESIAN_POINT('Ctrl Pts',(78.2638620892544,283.695586098007,58.3181273708052));
#39550=CARTESIAN_POINT('Ctrl Pts',(74.4200471881275,283.271274078902,58.8621814970761));
#39551=CARTESIAN_POINT('Ctrl Pts',(70.7530948079326,282.846962059797,57.5876744834349));
#39552=CARTESIAN_POINT('Ctrl Pts',(68.3123700687952,282.316572035917,52.8557580344726));
#39553=CARTESIAN_POINT('Ctrl Pts',(71.5275734779309,281.68010400726,47.3122932630761));
#39554=CARTESIAN_POINT('Ctrl Pts',(77.9173327360281,281.043635978603,47.0278990613398));
#39555=CARTESIAN_POINT('Ctrl Pts',(80.5292436010146,280.594599262481,50.7076804397306));
#39556=CARTESIAN_POINT('Ctrl Pts',(80.6397226976433,280.357718555911,52.7999815491162));
#39557=CARTESIAN_POINT('Ctrl Pts',(80.6380317763782,280.332993858894,53.0185653928147));
#39558=CARTESIAN_POINT('Origin',(74.9879498948689,423.667006141107,53.0228109606356));
#39559=CARTESIAN_POINT('',(80.6223389969519,289.667006141107,53.0226618801889));
#39560=CARTESIAN_POINT('',(80.620338754176,288.332993858894,53.0230516208103));
#39561=CARTESIAN_POINT('',(80.6314498948689,423.667006141107,53.0228109606222));
#39562=CARTESIAN_POINT('Ctrl Pts',(80.6223389969519,289.667006141107,53.0226618801889));
#39563=CARTESIAN_POINT('Ctrl Pts',(80.6214784739939,289.558958193161,53.9839632426538));
#39564=CARTESIAN_POINT('Ctrl Pts',(79.9289801677415,289.238754235662,56.8332978081037));
#39565=CARTESIAN_POINT('Ctrl Pts',(75.4037717530398,288.706394268611,59.6869920433574));
#39566=CARTESIAN_POINT('Ctrl Pts',(69.6005983433171,288.069926239955,56.9684054601267));
#39567=CARTESIAN_POINT('Ctrl Pts',(68.9056248589062,287.539536216073,51.6896572763087));
#39568=CARTESIAN_POINT('Ctrl Pts',(71.1901917605342,287.115224196969,48.5509215501885));
#39569=CARTESIAN_POINT('Ctrl Pts',(74.6574983630918,286.690912177864,46.8048709179623));
#39570=CARTESIAN_POINT('Ctrl Pts',(79.2961199120551,286.20817282591,48.2071989139687));
#39571=CARTESIAN_POINT('Ctrl Pts',(80.6181378226749,285.831511478732,51.5697725243201));
#39572=CARTESIAN_POINT('Ctrl Pts',(80.6320072490403,285.667006141107,53.0282647722843));
#39573=CARTESIAN_POINT('Ctrl Pts',(80.620338754176,288.332993858894,53.0230516208103));
#39574=CARTESIAN_POINT('Ctrl Pts',(80.6214818087189,288.236924003872,53.8774821547362));
#39575=CARTESIAN_POINT('Ctrl Pts',(80.2371756449924,288.034776144075,55.674607152298));
#39576=CARTESIAN_POINT('Ctrl Pts',(78.3882223800832,287.726550279501,57.8039100782516));
#39577=CARTESIAN_POINT('Ctrl Pts',(74.7839532242394,287.302238260396,59.246183193397));
#39578=CARTESIAN_POINT('Ctrl Pts',(69.8383632853863,286.771848236515,57.2740496561053));
#39579=CARTESIAN_POINT('Ctrl Pts',(68.6308295619551,286.135380207858,50.9804499754289));
#39580=CARTESIAN_POINT('Ctrl Pts',(73.268595959504,285.498912179202,46.5757903654038));
#39581=CARTESIAN_POINT('Ctrl Pts',(79.1354669206025,284.898116729547,48.0014226755356));
#39582=CARTESIAN_POINT('Ctrl Pts',(80.6216450875187,284.509477289444,51.4677109764803));
#39583=CARTESIAN_POINT('Ctrl Pts',(80.6355667283407,284.332993858894,53.029097899403));
#39584=CARTESIAN_POINT('Origin',(74.9879498948689,423.667006141107,53.0228109606356));
#39585=CARTESIAN_POINT('',(80.6324604068353,293.667006141107,53.0178216104937));
#39586=CARTESIAN_POINT('',(80.631774688763,292.332993858894,53.0191408716922));
#39587=CARTESIAN_POINT('',(80.6314498948689,423.667006141107,53.0228109606222));
#39588=CARTESIAN_POINT('Ctrl Pts',(80.6324604068353,293.667006141107,53.0178216104937));
#39589=CARTESIAN_POINT('Ctrl Pts',(80.6191313922384,293.498560917141,54.5094386793754));
#39590=CARTESIAN_POINT('Ctrl Pts',(79.2484550408878,293.117959683623,57.9019599664741));
#39591=CARTESIAN_POINT('Ctrl Pts',(73.5077494891626,292.525202440553,59.5343606573951));
#39592=CARTESIAN_POINT('Ctrl Pts',(69.5216244297834,291.994812416672,56.0046329705635));
#39593=CARTESIAN_POINT('Ctrl Pts',(69.188310236716,291.570500397568,52.1368416712381));
#39594=CARTESIAN_POINT('Ctrl Pts',(70.6611837554908,291.146188378463,48.5449686940674));
#39595=CARTESIAN_POINT('Ctrl Pts',(75.519336798809,290.615798354582,46.3663178409258));
#39596=CARTESIAN_POINT('Ctrl Pts',(79.9690770453548,290.087378273871,49.2830760364057));
#39597=CARTESIAN_POINT('Ctrl Pts',(80.623168141594,289.771114202713,52.0964136416258));
#39598=CARTESIAN_POINT('Ctrl Pts',(80.6223389969519,289.667006141107,53.0226618801889));
#39599=CARTESIAN_POINT('Ctrl Pts',(80.631774688763,292.332993858894,53.0191408716922));
#39600=CARTESIAN_POINT('Ctrl Pts',(80.6289723051447,292.282604732629,53.4660254458849));
#39601=CARTESIAN_POINT('Ctrl Pts',(80.4572238746464,292.126137601588,54.8559768464921));
#39602=CARTESIAN_POINT('Ctrl Pts',(78.9147710729384,291.757514460995,57.8552070562179));
#39603=CARTESIAN_POINT('Ctrl Pts',(73.8876807942301,291.227124437114,59.6092121479762));
#39604=CARTESIAN_POINT('Ctrl Pts',(68.849107759653,290.590656408457,55.6493742208554));
#39605=CARTESIAN_POINT('Ctrl Pts',(69.4623515772426,289.9541883798,49.2827553804812));
#39606=CARTESIAN_POINT('Ctrl Pts',(75.145158953817,289.317720351143,46.3475205075674));
#39607=CARTESIAN_POINT('Ctrl Pts',(79.8562903143711,288.777322177508,49.0697980922682));
#39608=CARTESIAN_POINT('Ctrl Pts',(80.6189575424913,288.449080013425,51.9905991936166));
#39609=CARTESIAN_POINT('Ctrl Pts',(80.620338754176,288.332993858894,53.0230516208103));
#39610=CARTESIAN_POINT('Origin',(74.9879498948689,423.667006141107,53.0228109606356));
#39611=CARTESIAN_POINT('',(80.6398778085108,297.667006141107,53.0246601447562));
#39612=CARTESIAN_POINT('',(80.6388022101255,296.332993858894,53.0227366527281));
#39613=CARTESIAN_POINT('',(80.6314498948689,423.667006141107,53.0228109606222));
#39614=CARTESIAN_POINT('Ctrl Pts',(80.6398778085108,297.667006141107,53.0246601447562));
#39615=CARTESIAN_POINT('Ctrl Pts',(80.6407234024158,297.650319650674,53.1720103840775));
#39616=CARTESIAN_POINT('Ctrl Pts',(80.5684082111312,297.421477150689,55.1921130767689));
#39617=CARTESIAN_POINT('Ctrl Pts',(78.1402065526217,296.980478641151,58.909622547401));
#39618=CARTESIAN_POINT('Ctrl Pts',(72.8161519838604,296.450088617271,58.8585003306135));
#39619=CARTESIAN_POINT('Ctrl Pts',(70.0282823888382,296.025776598166,56.1568913641665));
#39620=CARTESIAN_POINT('Ctrl Pts',(68.7850071190202,295.601464579061,52.4792325314445));
#39621=CARTESIAN_POINT('Ctrl Pts',(71.0242980864921,295.071074555181,47.6487308499217));
#39622=CARTESIAN_POINT('Ctrl Pts',(77.3744534912965,294.434606526524,46.7867210073652));
#39623=CARTESIAN_POINT('Ctrl Pts',(80.4223038359955,293.966583721832,50.3688767351797));
#39624=CARTESIAN_POINT('Ctrl Pts',(80.6359192267734,293.710716926693,52.63075362281));
#39625=CARTESIAN_POINT('Ctrl Pts',(80.6324604068353,293.667006141107,53.0178216104937));
#39626=CARTESIAN_POINT('Ctrl Pts',(80.6388022101255,296.332993858894,53.0227366527281));
#39627=CARTESIAN_POINT('Ctrl Pts',(80.638798598822,296.328285461386,53.0643189418008));
#39628=CARTESIAN_POINT('Ctrl Pts',(80.6158508992825,296.111421054325,54.9794472511519));
#39629=CARTESIAN_POINT('Ctrl Pts',(78.4761358999726,295.682400637713,58.717003711871));
#39630=CARTESIAN_POINT('Ctrl Pts',(72.0754506158946,295.045932609055,59.0312687720055));
#39631=CARTESIAN_POINT('Ctrl Pts',(68.3636791850171,294.409464580399,53.8223671331437));
#39632=CARTESIAN_POINT('Ctrl Pts',(70.7294688552404,293.772996551742,47.8798977243302));
#39633=CARTESIAN_POINT('Ctrl Pts',(77.0211072714768,293.136528523085,46.6621864805733));
#39634=CARTESIAN_POINT('Ctrl Pts',(80.3413046990379,292.656527625469,50.1541699818498));
#39635=CARTESIAN_POINT('Ctrl Pts',(80.6348718172991,292.388682737405,52.5252545393511));
#39636=CARTESIAN_POINT('Ctrl Pts',(80.631774688763,292.332993858894,53.0191408716922));
#39637=CARTESIAN_POINT('Origin',(74.9879498948689,423.667006141107,53.0228109606356));
#39638=CARTESIAN_POINT('',(80.6249680425302,301.667006141107,53.0279939180991));
#39639=CARTESIAN_POINT('',(80.6269504670759,300.332993858894,53.0280711906708));
#39640=CARTESIAN_POINT('',(80.6314498948689,423.667006141107,53.0228109606222));
#39641=CARTESIAN_POINT('Ctrl Pts',(80.6249680425302,301.667006141107,53.0279939180991));
#39642=CARTESIAN_POINT('Ctrl Pts',(80.6292423549922,301.589922374655,53.7134873977605));
#39643=CARTESIAN_POINT('Ctrl Pts',(80.1958374117308,301.30068259865,56.2795585259795));
#39644=CARTESIAN_POINT('Ctrl Pts',(77.1748718396303,300.905364817869,58.8528494679402));
#39645=CARTESIAN_POINT('Ctrl Pts',(73.2985174821482,300.481052798765,58.6412253160407));
#39646=CARTESIAN_POINT('Ctrl Pts',(69.9483047892701,300.05674077966,56.6798526337298));
#39647=CARTESIAN_POINT('Ctrl Pts',(68.4714694295786,299.526350755779,51.5644711374421));
#39648=CARTESIAN_POINT('Ctrl Pts',(72.700576392418,298.889882727122,46.7496825719188));
#39649=CARTESIAN_POINT('Ctrl Pts',(78.8584126251663,298.270101188898,47.6845510583783));
#39650=CARTESIAN_POINT('Ctrl Pts',(80.629972320317,297.862475660226,51.2985643825386));
#39651=CARTESIAN_POINT('Ctrl Pts',(80.6398778085108,297.667006141107,53.0246601447562));
#39652=CARTESIAN_POINT('Ctrl Pts',(80.6269504670759,300.332993858894,53.0280711906708));
#39653=CARTESIAN_POINT('Ctrl Pts',(80.6321628473983,300.267888185366,53.6055090465738));
#39654=CARTESIAN_POINT('Ctrl Pts',(80.28646611962,299.990626502287,56.0591348011215));
#39655=CARTESIAN_POINT('Ctrl Pts',(76.728933306676,299.501208809654,59.4689876632131));
#39656=CARTESIAN_POINT('Ctrl Pts',(70.5109339842768,298.864740780998,57.9701921918225));
#39657=CARTESIAN_POINT('Ctrl Pts',(68.40045667283,298.22827275234,51.9323292456896));
#39658=CARTESIAN_POINT('Ctrl Pts',(72.3521401674818,297.591804723684,46.8873582654032));
#39659=CARTESIAN_POINT('Ctrl Pts',(77.6521973570184,297.061414699802,47.3948662159206));
#39660=CARTESIAN_POINT('Ctrl Pts',(80.1698643867066,296.641811078207,50.2930805494598));
#39661=CARTESIAN_POINT('Ctrl Pts',(80.6388799598091,296.434363466162,52.1274893195652));
#39662=CARTESIAN_POINT('Ctrl Pts',(80.6388022101255,296.332993858894,53.0227366527281));
#39663=CARTESIAN_POINT('Origin',(74.9879498948689,423.667006141107,53.0228109606356));
#39664=CARTESIAN_POINT('',(80.6245874480474,305.667006141107,53.0180653057103));
#39665=CARTESIAN_POINT('',(80.6234016113781,304.332993858894,53.0188635924083));
#39666=CARTESIAN_POINT('',(80.6314498948689,423.667006141107,53.0228109606222));
#39667=CARTESIAN_POINT('Ctrl Pts',(80.6245874480474,305.667006141107,53.0180653057103));
#39668=CARTESIAN_POINT('Ctrl Pts',(80.615226689223,305.529525098635,54.238624327565));
#39669=CARTESIAN_POINT('Ctrl Pts',(79.9225057346746,305.285966051388,56.4096693070596));
#39670=CARTESIAN_POINT('Ctrl Pts',(77.3965832675933,304.936328999363,58.372506935359));
#39671=CARTESIAN_POINT('Ctrl Pts',(73.5810548415566,304.512016980259,59.0885032457832));
#39672=CARTESIAN_POINT('Ctrl Pts',(69.1117501822202,303.981626956378,56.1948055431484));
#39673=CARTESIAN_POINT('Ctrl Pts',(69.1475242377325,303.345158927721,49.7865097594955));
#39674=CARTESIAN_POINT('Ctrl Pts',(74.551368128498,302.708690899064,46.3647595285971));
#39675=CARTESIAN_POINT('Ctrl Pts',(79.6527817257398,302.149306636859,48.7261596244971));
#39676=CARTESIAN_POINT('Ctrl Pts',(80.6174782557889,301.802078384207,51.8268182855386));
#39677=CARTESIAN_POINT('Ctrl Pts',(80.6249680425302,301.667006141107,53.0279939180991));
#39678=CARTESIAN_POINT('Ctrl Pts',(80.6234016113781,304.332993858894,53.0188635924083));
#39679=CARTESIAN_POINT('Ctrl Pts',(80.6185287438372,304.207490909347,54.1357754126701));
#39680=CARTESIAN_POINT('Ctrl Pts',(79.7563688183985,303.869831950248,57.149097718398));
#39681=CARTESIAN_POINT('Ctrl Pts',(74.8519499260711,303.320016981596,59.6937746480561));
#39682=CARTESIAN_POINT('Ctrl Pts',(69.2993505210926,302.683548952939,56.5191024939194));
#39683=CARTESIAN_POINT('Ctrl Pts',(68.9747335748927,302.047080924282,50.1189338655102));
#39684=CARTESIAN_POINT('Ctrl Pts',(73.3090500016354,301.516690900401,47.0267062469374));
#39685=CARTESIAN_POINT('Ctrl Pts',(77.1529760290398,301.092378881297,47.569974672562));
#39686=CARTESIAN_POINT('Ctrl Pts',(79.8362973275973,300.733172535719,49.4675012984646));
#39687=CARTESIAN_POINT('Ctrl Pts',(80.6151775717754,300.480044194919,51.7238464412254));
#39688=CARTESIAN_POINT('Ctrl Pts',(80.6269504670759,300.332993858894,53.0280711906708));
#39689=CARTESIAN_POINT('Origin',(74.9879498948689,423.667006141107,53.0228109606356));
#39690=CARTESIAN_POINT('',(80.6384239058391,309.667006141107,53.0216495976625));
#39691=CARTESIAN_POINT('',(80.6380282624043,308.332993858894,53.019732459396));
#39692=CARTESIAN_POINT('',(80.6314498948689,423.667006141107,53.0228109606222));
#39693=CARTESIAN_POINT('Ctrl Pts',(80.6384239058391,309.667006141107,53.0216495976625));
#39694=CARTESIAN_POINT('Ctrl Pts',(80.6362110086977,309.575205827392,53.8327216460468));
#39695=CARTESIAN_POINT('Ctrl Pts',(80.233271064791,309.377327508901,55.5847876132963));
#39696=CARTESIAN_POINT('Ctrl Pts',(77.9031908065171,308.967293180857,58.5249330072815));
#39697=CARTESIAN_POINT('Ctrl Pts',(72.6313994367438,308.436903156976,59.2708460623881));
#39698=CARTESIAN_POINT('Ctrl Pts',(68.456311111176,307.80043512832,54.4091414120066));
#39699=CARTESIAN_POINT('Ctrl Pts',(70.2924624355432,307.163967099663,48.28227828701));
#39700=CARTESIAN_POINT('Ctrl Pts',(76.4365765807934,306.527499071006,46.5047055575397));
#39701=CARTESIAN_POINT('Ctrl Pts',(80.2166985631924,306.02851208482,49.8141896419487));
#39702=CARTESIAN_POINT('Ctrl Pts',(80.6296718898329,305.741681108187,52.3550996841352));
#39703=CARTESIAN_POINT('Ctrl Pts',(80.6245874480474,305.667006141107,53.0180653057103));
#39704=CARTESIAN_POINT('Ctrl Pts',(80.6380282624043,308.332993858894,53.019732459396));
#39705=CARTESIAN_POINT('Ctrl Pts',(80.6251916315742,308.147093633328,54.662633693795));
#39706=CARTESIAN_POINT('Ctrl Pts',(79.000792842538,307.749037398208,58.1998731366368));
#39707=CARTESIAN_POINT('Ctrl Pts',(72.985687726908,307.138825153538,59.39267465869));
#39708=CARTESIAN_POINT('Ctrl Pts',(68.5438343362777,306.50235712488,54.7734243851087));
#39709=CARTESIAN_POINT('Ctrl Pts',(69.7885723489147,305.971967101,49.5966688556199));
#39710=CARTESIAN_POINT('Ctrl Pts',(73.0469626822795,305.547655081895,47.4862659742077));
#39711=CARTESIAN_POINT('Ctrl Pts',(76.909836648915,305.123343062791,47.1001149618732));
#39712=CARTESIAN_POINT('Ctrl Pts',(80.1195933644604,304.718455988457,49.5935387681186));
#39713=CARTESIAN_POINT('Ctrl Pts',(80.626766065241,304.419646918899,52.2476958443102));
#39714=CARTESIAN_POINT('Ctrl Pts',(80.6234016113781,304.332993858894,53.0188635924083));
#39715=CARTESIAN_POINT('Origin',(74.9879498948689,423.667006141107,53.0228109606356));
#39716=CARTESIAN_POINT('',(80.6335754169153,313.667006141107,53.0264184895274));
#39717=CARTESIAN_POINT('',(80.634904065444,312.332993858894,53.0272790553122));
#39718=CARTESIAN_POINT('',(80.6314498948689,423.667006141107,53.0228109606222));
#39719=CARTESIAN_POINT('Ctrl Pts',(80.6335754169154,313.667006141107,53.0264184895274));
#39720=CARTESIAN_POINT('Ctrl Pts',(80.6362304506285,313.620886556148,53.4350520299685));
#39721=CARTESIAN_POINT('Ctrl Pts',(80.4021920393429,313.362610961638,55.7197413552384));
#39722=CARTESIAN_POINT('Ctrl Pts',(77.3057707044781,312.892179357576,59.2853168000712));
#39723=CARTESIAN_POINT('Ctrl Pts',(70.9656350492383,312.255711328918,58.3524639140331));
#39724=CARTESIAN_POINT('Ctrl Pts',(68.3343700832684,311.619243300261,52.5226827760076));
#39725=CARTESIAN_POINT('Ctrl Pts',(71.8075564021643,310.982775271605,47.1517535982347));
#39726=CARTESIAN_POINT('Ctrl Pts',(78.2159016640937,310.346307242947,47.1771630008298));
#39727=CARTESIAN_POINT('Ctrl Pts',(80.5733624654555,309.907717532782,50.8955937917629));
#39728=CARTESIAN_POINT('Ctrl Pts',(80.6387680774488,309.681283832168,52.8955036656214));
#39729=CARTESIAN_POINT('Ctrl Pts',(80.6384239058391,309.667006141107,53.0216495976625));
#39730=CARTESIAN_POINT('Ctrl Pts',(80.634904065444,312.332993858894,53.0272790553122));
#39731=CARTESIAN_POINT('Ctrl Pts',(80.6374670364689,312.29885236686,53.3292671667975));
#39732=CARTESIAN_POINT('Ctrl Pts',(80.4774639995193,312.052554865274,55.5050485344305));
#39733=CARTESIAN_POINT('Ctrl Pts',(77.6531438362427,311.594101354136,59.1449803944151));
#39734=CARTESIAN_POINT('Ctrl Pts',(71.2705853255733,310.95763332548,58.5701051977721));
#39735=CARTESIAN_POINT('Ctrl Pts',(68.8158168069635,310.427243301598,53.8454589621013));
#39736=CARTESIAN_POINT('Ctrl Pts',(69.8920431913756,310.002931282494,50.1154931906856));
#39737=CARTESIAN_POINT('Ctrl Pts',(72.5552930136327,309.578619263389,47.2909563665877));
#39738=CARTESIAN_POINT('Ctrl Pts',(77.8716307581055,309.048229239508,46.9998833192451));
#39739=CARTESIAN_POINT('Ctrl Pts',(80.521218131808,308.597661436418,50.6823624775674));
#39740=CARTESIAN_POINT('Ctrl Pts',(80.6398412553964,308.35924964288,52.7876958398109));
#39741=CARTESIAN_POINT('Ctrl Pts',(80.6380282624043,308.332993858894,53.019732459396));
#39742=CARTESIAN_POINT('Origin',(74.9879498948689,423.667006141107,53.0228109606356));
#39743=CARTESIAN_POINT('',(80.6203056371871,317.667006141107,53.0239157025499));
#39744=CARTESIAN_POINT('',(80.6314498948689,316.332993858894,53.022810960631));
#39745=CARTESIAN_POINT('',(80.6314498948689,423.667006141107,53.0228109606222));
#39746=CARTESIAN_POINT('Ctrl Pts',(80.6203056371871,317.667006141107,53.0239157025499));
#39747=CARTESIAN_POINT('Ctrl Pts',(80.6211875158354,317.560489280129,53.9712705130797));
#39748=CARTESIAN_POINT('Ctrl Pts',(79.9483727986063,317.241816409599,56.8042629861476));
#39749=CARTESIAN_POINT('Ctrl Pts',(75.4459142368694,316.710987529517,59.6842286762946));
#39750=CARTESIAN_POINT('Ctrl Pts',(69.6365665351741,316.07451950086,57.0081526834969));
#39751=CARTESIAN_POINT('Ctrl Pts',(68.7369456197939,315.438051472203,50.6756503623739));
#39752=CARTESIAN_POINT('Ctrl Pts',(73.5918912351737,314.801583443546,46.4927043065974));
#39753=CARTESIAN_POINT('Ctrl Pts',(78.6929398225512,314.271193419665,48.0183103636822));
#39754=CARTESIAN_POINT('Ctrl Pts',(80.4125372384092,313.893000985519,51.0209339978467));
#39755=CARTESIAN_POINT('Ctrl Pts',(80.6301237027218,313.726964560925,52.4951686660161));
#39756=CARTESIAN_POINT('Ctrl Pts',(80.6335754169154,313.667006141107,53.0264184895274));
#39757=CARTESIAN_POINT('Ctrl Pts',(80.622881869106,316.332993858894,53.0242648148771));
#39758=CARTESIAN_POINT('Ctrl Pts',(80.6254517968293,316.238455090841,53.8652024741767));
#39759=CARTESIAN_POINT('Ctrl Pts',(80.0544782228084,315.931760313236,56.5905993295512));
#39760=CARTESIAN_POINT('Ctrl Pts',(75.8188643388059,315.412909526078,59.6485829067018));
#39761=CARTESIAN_POINT('Ctrl Pts',(70.8674386639765,314.882519502197,57.6911472579929));
#39762=CARTESIAN_POINT('Ctrl Pts',(69.2341445588646,314.458207483093,54.1693212752611));
#39763=CARTESIAN_POINT('Ctrl Pts',(69.3927639357589,314.033895463987,50.2904364123513));
#39764=CARTESIAN_POINT('Ctrl Pts',(73.2157203846311,313.503505440107,46.5846066102391));
#39765=CARTESIAN_POINT('Ctrl Pts',(79.1179469702306,312.901178903483,47.9787113040824));
#39766=CARTESIAN_POINT('Ctrl Pts',(80.6215406761124,312.511008376413,51.4527061599728));
#39767=CARTESIAN_POINT('Ctrl Pts',(80.634904065444,312.332993858894,53.0272790553122));
#39768=CARTESIAN_POINT('Origin',(74.9879498948689,423.667006141107,53.0228109606356));
#39769=CARTESIAN_POINT('',(80.6329360039533,321.667006141107,53.0160580430196));
#39770=CARTESIAN_POINT('',(80.6314498948689,320.332993858894,53.0228109606313));
#39771=CARTESIAN_POINT('',(80.6314498948689,423.667006141107,53.0228109606222));
#39772=CARTESIAN_POINT('Ctrl Pts',(80.6329360039533,321.667006141107,53.0160580430195));
#39773=CARTESIAN_POINT('Ctrl Pts',(80.6191346339023,321.50009200411,54.4947146401021));
#39774=CARTESIAN_POINT('Ctrl Pts',(79.2652823955181,321.121021857561,57.8790253272329));
#39775=CARTESIAN_POINT('Ctrl Pts',(73.5609687392484,320.529795701458,59.5407843643785));
#39776=CARTESIAN_POINT('Ctrl Pts',(68.7293595293914,319.893327672802,55.3496680594258));
#39777=CARTESIAN_POINT('Ctrl Pts',(69.6519568295469,319.256859644144,49.0080319254632));
#39778=CARTESIAN_POINT('Ctrl Pts',(74.5036175039259,318.726469620264,46.8149611940725));
#39779=CARTESIAN_POINT('Ctrl Pts',(78.1692388187073,318.302157601159,48.0932914577593));
#39780=CARTESIAN_POINT('Ctrl Pts',(80.1726242007646,317.984362443032,50.2005331564451));
#39781=CARTESIAN_POINT('Ctrl Pts',(80.6194310253304,317.772645289682,52.0843672154471));
#39782=CARTESIAN_POINT('Ctrl Pts',(80.6203056371871,317.667006141107,53.0239157025499));
#39783=CARTESIAN_POINT('Ctrl Pts',(80.6314498948689,320.332993858894,53.0228109606313));
#39784=CARTESIAN_POINT('Ctrl Pts',(80.6314498948702,320.140209036291,54.7318077489503));
#39785=CARTESIAN_POINT('Ctrl Pts',(79.8060659192661,319.947424213689,56.4221521097307));
#39786=CARTESIAN_POINT('Ctrl Pts',(78.4584055093399,319.754639391087,57.4730952299814));
#39787=CARTESIAN_POINT('Ctrl Pts',(77.1107450994137,319.561854568484,58.5240383502321));
#39788=CARTESIAN_POINT('Ctrl Pts',(75.2702256751575,319.369069745882,58.9126397065625));
#39789=CARTESIAN_POINT('Ctrl Pts',(73.6127451626997,319.176284923279,58.4961923829941));
#39790=CARTESIAN_POINT('Ctrl Pts',(71.9552646502418,318.983500100677,58.0797450594257));
#39791=CARTESIAN_POINT('Ctrl Pts',(70.51700338107,318.790715278075,56.867339480914));
#39792=CARTESIAN_POINT('Ctrl Pts',(69.8261371496106,318.597930455472,55.3042099684571));
#39793=CARTESIAN_POINT('Ctrl Pts',(69.1352709181512,318.40514563287,53.7410804560001));
#39794=CARTESIAN_POINT('Ctrl Pts',(69.206880305491,318.212360810268,51.8613477992505));
#39795=CARTESIAN_POINT('Ctrl Pts',(70.0146680415461,318.019575987665,50.3553102844576));
#39796=CARTESIAN_POINT('Ctrl Pts',(70.8224557776012,317.826791165063,48.8492727696646));
#39797=CARTESIAN_POINT('Ctrl Pts',(72.3487890589435,317.63400634246,47.7498049531857));
#39798=CARTESIAN_POINT('Ctrl Pts',(74.033149215765,317.441221519858,47.4606667775725));
#39799=CARTESIAN_POINT('Ctrl Pts',(75.7175093725865,317.248436697255,47.1715286019592));
#39800=CARTESIAN_POINT('Ctrl Pts',(77.5231293307887,317.055651874653,47.6990315230392));
#39801=CARTESIAN_POINT('Ctrl Pts',(78.7869273705914,316.862867052051,48.8494595029995));
#39802=CARTESIAN_POINT('Ctrl Pts',(79.9447859852136,316.686242654332,49.9034514424928));
#39803=CARTESIAN_POINT('Ctrl Pts',(80.6314498948676,316.509618256613,51.4570729301893));
#39804=CARTESIAN_POINT('Ctrl Pts',(80.6314498948689,316.332993858894,53.022810960631));
#39805=CARTESIAN_POINT('Origin',(74.9879498948689,423.667006141107,53.0228109606356));
#39806=CARTESIAN_POINT('',(80.6399041832245,325.667006141107,53.0259007613615));
#39807=CARTESIAN_POINT('',(80.641309217006,324.332993858894,53.0246324837175));
#39808=CARTESIAN_POINT('',(80.6314498948689,423.667006141107,53.0228109606222));
#39809=CARTESIAN_POINT('Ctrl Pts',(80.6399041832245,325.667006141107,53.0259007613615));
#39810=CARTESIAN_POINT('Ctrl Pts',(80.6406482967255,325.651850737642,53.1597610770503));
#39811=CARTESIAN_POINT('Ctrl Pts',(80.5759040625624,325.424539324626,55.1666404955042));
#39812=CARTESIAN_POINT('Ctrl Pts',(78.1845991508713,324.985071902057,58.8795750880781));
#39813=CARTESIAN_POINT('Ctrl Pts',(71.7885153548133,324.3486038734,58.8835136441829));
#39814=CARTESIAN_POINT('Ctrl Pts',(68.3266868515903,323.712135844743,53.4906222074762));
#39815=CARTESIAN_POINT('Ctrl Pts',(70.5516205825161,323.181745820863,48.6534907822217));
#39816=CARTESIAN_POINT('Ctrl Pts',(74.1573917987538,322.757433801757,47.2149770274767));
#39817=CARTESIAN_POINT('Ctrl Pts',(78.0218245725355,322.333121782654,47.5852029360215));
#39818=CARTESIAN_POINT('Ctrl Pts',(80.4145538626956,321.969645895769,50.3398610757797));
#39819=CARTESIAN_POINT('Ctrl Pts',(80.6366768484148,321.712248013662,52.6152699820339));
#39820=CARTESIAN_POINT('Ctrl Pts',(80.6329360039533,321.667006141107,53.0160580430195));
#39821=CARTESIAN_POINT('Ctrl Pts',(80.641309217006,324.332993858894,53.0246324837175));
#39822=CARTESIAN_POINT('Ctrl Pts',(80.6413395611219,324.329816548354,53.0526541263013));
#39823=CARTESIAN_POINT('Ctrl Pts',(80.627934128378,324.114483228262,54.9516482048753));
#39824=CARTESIAN_POINT('Ctrl Pts',(79.0332371365105,323.793071903394,57.7564805437124));
#39825=CARTESIAN_POINT('Ctrl Pts',(75.3173868460731,323.36875988429,58.8804754304867));
#39826=CARTESIAN_POINT('Ctrl Pts',(71.4989396689043,322.944447865185,58.1802118789516));
#39827=CARTESIAN_POINT('Ctrl Pts',(68.3650037426683,322.414057841304,53.8759562937844));
#39828=CARTESIAN_POINT('Ctrl Pts',(70.6970252219288,321.777589812648,47.9069353980174));
#39829=CARTESIAN_POINT('Ctrl Pts',(76.9686349527099,321.14112178399,46.6512225235155));
#39830=CARTESIAN_POINT('Ctrl Pts',(80.3386907684742,320.659589799406,50.1238895100213));
#39831=CARTESIAN_POINT('Ctrl Pts',(80.6339788010566,320.390213824374,52.5096602373864));
#39832=CARTESIAN_POINT('Ctrl Pts',(80.6293902184787,320.332993858894,53.0175789310935));
#39833=CARTESIAN_POINT('Origin',(74.9879498948689,423.667006141107,53.0228109606356));
#39834=CARTESIAN_POINT('',(80.6249975362087,329.667006141107,53.0267352952636));
#39835=CARTESIAN_POINT('',(80.6248446978252,328.332993858894,53.0267008926206));
#39836=CARTESIAN_POINT('',(80.6314498948689,423.667006141107,53.0228109606222));
#39837=CARTESIAN_POINT('Ctrl Pts',(80.6249975362087,329.667006141107,53.0267352952636));
#39838=CARTESIAN_POINT('Ctrl Pts',(80.6290331419222,329.591453461623,53.6980665132406));
#39839=CARTESIAN_POINT('Ctrl Pts',(80.2059687603599,329.303744772587,56.2493246988747));
#39840=CARTESIAN_POINT('Ctrl Pts',(76.4154107889894,328.803880073999,59.5455843521308));
#39841=CARTESIAN_POINT('Ctrl Pts',(70.265470501402,328.167412045342,57.7439825390367));
#39842=CARTESIAN_POINT('Ctrl Pts',(68.7734481583349,327.637022021461,52.6330100425361));
#39843=CARTESIAN_POINT('Ctrl Pts',(70.5525225770171,327.212710002356,49.182531510618));
#39844=CARTESIAN_POINT('Ctrl Pts',(73.7129266627949,326.788397983251,46.9280351364722));
#39845=CARTESIAN_POINT('Ctrl Pts',(78.8341602790448,326.273163362835,47.6520772747905));
#39846=CARTESIAN_POINT('Ctrl Pts',(80.6302316719622,325.864006747195,51.2858901186813));
#39847=CARTESIAN_POINT('Ctrl Pts',(80.6399041832245,325.667006141107,53.0259007613615));
#39848=CARTESIAN_POINT('Ctrl Pts',(80.6248446978252,328.332993858894,53.0267008926206));
#39849=CARTESIAN_POINT('Ctrl Pts',(80.6292140414995,328.269419272335,53.5910781635921));
#39850=CARTESIAN_POINT('Ctrl Pts',(80.4218299720533,328.099766681,55.094490841645));
#39851=CARTESIAN_POINT('Ctrl Pts',(79.0777073227094,327.824036084888,57.2293113977682));
#39852=CARTESIAN_POINT('Ctrl Pts',(75.7356073875843,327.399724065784,59.2044761782546));
#39853=CARTESIAN_POINT('Ctrl Pts',(70.5470739238278,326.869334041903,58.0097833191163));
#39854=CARTESIAN_POINT('Ctrl Pts',(68.3936911683374,326.232866013246,51.97401681086));
#39855=CARTESIAN_POINT('Ctrl Pts',(72.3053343322745,325.596397984589,46.9134880641335));
#39856=CARTESIAN_POINT('Ctrl Pts',(78.6463794007935,324.963107266471,47.4553532968724));
#39857=CARTESIAN_POINT('Ctrl Pts',(80.6393134177985,324.541972557907,51.1815874497272));
#39858=CARTESIAN_POINT('Ctrl Pts',(80.641309217006,324.332993858894,53.0246324837175));
#39859=CARTESIAN_POINT('Origin',(74.9879498948689,423.667006141107,53.0228109606356));
#39860=CARTESIAN_POINT('',(80.6248818348672,333.667006141107,53.0189479369226));
#39861=CARTESIAN_POINT('',(80.6272015301536,332.332993858894,53.0209924349646));
#39862=CARTESIAN_POINT('',(80.6314498948689,423.667006141107,53.0228109606222));
#39863=CARTESIAN_POINT('Ctrl Pts',(80.6248818348672,333.667006141107,53.0189479369226));
#39864=CARTESIAN_POINT('Ctrl Pts',(80.6177572981036,333.531056185603,54.2270097895939));
#39865=CARTESIAN_POINT('Ctrl Pts',(79.6454537625307,333.182950220548,57.3314456583965));
#39866=CARTESIAN_POINT('Ctrl Pts',(74.5182936803783,332.622688245941,59.6839441776349));
#39867=CARTESIAN_POINT('Ctrl Pts',(70.0404139918865,332.09229822206,56.8035337854184));
#39868=CARTESIAN_POINT('Ctrl Pts',(69.1210358704998,331.667986202955,53.0318429502156));
#39869=CARTESIAN_POINT('Ctrl Pts',(70.0287967856483,331.24367418385,49.257339273258));
#39870=CARTESIAN_POINT('Ctrl Pts',(74.4977866088157,330.71328415997,46.3631553653794));
#39871=CARTESIAN_POINT('Ctrl Pts',(79.6381532999905,330.152368810796,48.7025815115751));
#39872=CARTESIAN_POINT('Ctrl Pts',(80.6177009428506,329.803609471175,51.8129321504717));
#39873=CARTESIAN_POINT('Ctrl Pts',(80.6249975362087,329.667006141107,53.0267352952636));
#39874=CARTESIAN_POINT('Ctrl Pts',(80.6272015301536,332.332993858894,53.0209924349646));
#39875=CARTESIAN_POINT('Ctrl Pts',(80.6267710083896,332.315100001092,53.1800532435297));
#39876=CARTESIAN_POINT('Ctrl Pts',(80.5787897955094,332.191128138513,54.282321197091));
#39877=CARTESIAN_POINT('Ctrl Pts',(79.605919036016,331.855000266382,57.199692285326));
#39878=CARTESIAN_POINT('Ctrl Pts',(74.9051964886825,331.324610242502,59.6999678831728));
#39879=CARTESIAN_POINT('Ctrl Pts',(69.3215782779007,330.688142213844,56.5550128262509));
#39880=CARTESIAN_POINT('Ctrl Pts',(68.9565293265754,330.051674185188,50.1693536823915));
#39881=CARTESIAN_POINT('Ctrl Pts',(74.1251200219098,329.415206156531,46.4016523058858));
#39882=CARTESIAN_POINT('Ctrl Pts',(79.5013040728498,328.842312714433,48.4920436759634));
#39883=CARTESIAN_POINT('Ctrl Pts',(80.6146330183506,328.481575281887,51.7076836159886));
#39884=CARTESIAN_POINT('Ctrl Pts',(80.6248446978252,328.332993858894,53.0267008926206));
#39885=CARTESIAN_POINT('Origin',(74.9879498948689,423.667006141107,53.0228109606356));
#39886=CARTESIAN_POINT('',(80.6397967405656,337.667006141107,53.0196325004034));
#39887=CARTESIAN_POINT('',(80.6340573567893,336.332993858894,53.0189717794449));
#39888=CARTESIAN_POINT('',(80.6314498948689,423.667006141107,53.0228109606222));
#39889=CARTESIAN_POINT('Ctrl Pts',(80.6397967405657,337.667006141107,53.0196325004034));
#39890=CARTESIAN_POINT('Ctrl Pts',(80.6298465402105,337.470658909584,54.7539666249281));
#39891=CARTESIAN_POINT('Ctrl Pts',(78.8441868361869,337.062155668509,58.3826150558032));
#39892=CARTESIAN_POINT('Ctrl Pts',(73.7316982178695,336.547574422658,59.1214836287799));
#39893=CARTESIAN_POINT('Ctrl Pts',(70.5643676301849,336.123262403554,56.8767286678197));
#39894=CARTESIAN_POINT('Ctrl Pts',(68.7746777925706,335.698950384449,53.4317441727057));
#39895=CARTESIAN_POINT('Ctrl Pts',(70.2509566334843,335.168560360568,48.3162020395523));
#39896=CARTESIAN_POINT('Ctrl Pts',(76.3953207281506,334.532092331911,46.4956734058825));
#39897=CARTESIAN_POINT('Ctrl Pts',(80.2009776432158,334.031574258758,49.7845397703628));
#39898=CARTESIAN_POINT('Ctrl Pts',(80.6288754576064,333.743212195156,52.3417750279739));
#39899=CARTESIAN_POINT('Ctrl Pts',(80.6248818348672,333.667006141107,53.0189479369226));
#39900=CARTESIAN_POINT('Ctrl Pts',(80.6340573567893,336.332993858894,53.0189717794449));
#39901=CARTESIAN_POINT('Ctrl Pts',(80.6200188883937,336.148624720296,54.649623440592));
#39902=CARTESIAN_POINT('Ctrl Pts',(79.0297907033757,335.752099572145,58.1744941480767));
#39903=CARTESIAN_POINT('Ctrl Pts',(73.0260170282693,335.143418414444,59.4052115080782));
#39904=CARTESIAN_POINT('Ctrl Pts',(68.5631518514559,334.506950385786,54.8234282469443));
#39905=CARTESIAN_POINT('Ctrl Pts',(69.9948378458387,333.87048235713,48.5896349674149));
#39906=CARTESIAN_POINT('Ctrl Pts',(76.0271136359725,333.234014328472,46.4264929411948));
#39907=CARTESIAN_POINT('Ctrl Pts',(80.0993015055047,332.721518162394,49.5705266949811));
#39908=CARTESIAN_POINT('Ctrl Pts',(80.6293232187766,332.421178005868,52.2371121853679));
#39909=CARTESIAN_POINT('Ctrl Pts',(80.6272015301536,332.332993858894,53.0209924349646));
#39910=CARTESIAN_POINT('Origin',(74.9879498948689,423.667006141107,53.0228109606356));
#39911=CARTESIAN_POINT('',(80.6331187968458,341.667006141107,53.029546473955));
#39912=CARTESIAN_POINT('',(80.636192681801,340.332993858894,53.0268230851199));
#39913=CARTESIAN_POINT('',(80.6314498948689,423.667006141107,53.0228109606222));
#39914=CARTESIAN_POINT('Ctrl Pts',(80.6331187968458,341.667006141107,53.029546473955));
#39915=CARTESIAN_POINT('Ctrl Pts',(80.6368032847626,341.622417643117,53.4245109340992));
#39916=CARTESIAN_POINT('Ctrl Pts',(80.4185029699366,341.365673135575,55.6940048042392));
#39917=CARTESIAN_POINT('Ctrl Pts',(78.0385523165719,341.002850623257,58.4510520619348));
#39918=CARTESIAN_POINT('Ctrl Pts',(74.1752777672687,340.578538604152,58.8331746118364));
#39919=CARTESIAN_POINT('Ctrl Pts',(70.5650945300378,340.154226585048,57.4057696657705));
#39920=CARTESIAN_POINT('Ctrl Pts',(68.3252780582827,339.623836561167,52.5755116286618));
#39921=CARTESIAN_POINT('Ctrl Pts',(71.7704857081252,338.98736853251,47.1719869564409));
#39922=CARTESIAN_POINT('Ctrl Pts',(78.1665513135014,338.350900503852,47.1562322701325));
#39923=CARTESIAN_POINT('Ctrl Pts',(80.5728490636616,337.910779706719,50.8672957569095));
#39924=CARTESIAN_POINT('Ctrl Pts',(80.6405978749007,337.682814919137,52.8799936422873));
#39925=CARTESIAN_POINT('Ctrl Pts',(80.6397967405657,337.667006141107,53.0196325004034));
#39926=CARTESIAN_POINT('Ctrl Pts',(80.636192681801,340.332993858894,53.0268230851199));
#39927=CARTESIAN_POINT('Ctrl Pts',(80.6388801598045,340.300383453829,53.3149409966799));
#39928=CARTESIAN_POINT('Ctrl Pts',(80.4886957225858,340.055617039212,55.4751882644889));
#39929=CARTESIAN_POINT('Ctrl Pts',(77.6918131141847,339.598694615041,59.1280006392838));
#39930=CARTESIAN_POINT('Ctrl Pts',(71.3179589210744,338.962226586385,58.5951909515068));
#39931=CARTESIAN_POINT('Ctrl Pts',(68.3112066114293,338.325758557728,52.9498969833543));
#39932=CARTESIAN_POINT('Ctrl Pts',(71.4471267602236,337.689290529071,47.3611995095039));
#39933=CARTESIAN_POINT('Ctrl Pts',(76.762576521389,337.158900505191,47.0543373764116));
#39934=CARTESIAN_POINT('Ctrl Pts',(79.7257358927106,336.734588486085,49.5624431211091));
#39935=CARTESIAN_POINT('Ctrl Pts',(80.5669914044514,336.494645605579,51.5901499444678));
#39936=CARTESIAN_POINT('Ctrl Pts',(80.6361731399006,336.360780729848,52.773210977911));
#39937=CARTESIAN_POINT('Ctrl Pts',(80.6340573567893,336.332993858894,53.0189717794449));
#39938=CARTESIAN_POINT('Origin',(74.9879498948689,423.667006141107,53.0228109606356));
#39939=CARTESIAN_POINT('',(80.6202872556143,345.667006141106,53.0217977506596));
#39940=CARTESIAN_POINT('',(80.6311256770026,344.332993858894,53.022857263151));
#39941=CARTESIAN_POINT('',(80.6314498948689,423.667006141107,53.0228109606222));
#39942=CARTESIAN_POINT('Ctrl Pts',(80.6202875021214,345.667006141106,53.0217977730345));
#39943=CARTESIAN_POINT('Ctrl Pts',(80.6195633400336,345.562020367097,53.9555423965643));
#39944=CARTESIAN_POINT('Ctrl Pts',(80.1771837543004,345.350956588312,55.833457101896));
#39945=CARTESIAN_POINT('Ctrl Pts',(78.1844014847269,345.033814804751,57.942512067397));
#39946=CARTESIAN_POINT('Ctrl Pts',(74.5227334601851,344.609502785646,59.2321225374558));
#39947=CARTESIAN_POINT('Ctrl Pts',(69.664343426917,344.079112761766,57.0540002229753));
#39948=CARTESIAN_POINT('Ctrl Pts',(68.7222249177504,343.442644733109,50.7152347794114));
#39949=CARTESIAN_POINT('Ctrl Pts',(73.540906987327,342.806176704451,46.5092620559193));
#39950=CARTESIAN_POINT('Ctrl Pts',(79.2566196418042,342.214297173785,48.1552669397766));
#39951=CARTESIAN_POINT('Ctrl Pts',(80.6192721660009,341.834573652669,51.5452351666445));
#39952=CARTESIAN_POINT('Ctrl Pts',(80.6331187968458,341.667006141107,53.029546473955));
#39953=CARTESIAN_POINT('Ctrl Pts',(80.6225970303475,344.332993858894,53.0240752641163));
#39954=CARTESIAN_POINT('Ctrl Pts',(80.625144122426,344.239986177809,53.8521759519026));
#39955=CARTESIAN_POINT('Ctrl Pts',(80.0664343193197,343.934822487172,56.5663239398779));
#39956=CARTESIAN_POINT('Ctrl Pts',(75.8710807057947,343.417502786984,59.6364584021908));
#39957=CARTESIAN_POINT('Ctrl Pts',(69.8992144031925,342.781034758326,57.3458872283867));
#39958=CARTESIAN_POINT('Ctrl Pts',(68.6021616848208,342.14456672967,51.0701252125357));
#39959=CARTESIAN_POINT('Ctrl Pts',(72.4140943662755,341.614176705789,47.3529569671835));
#39960=CARTESIAN_POINT('Ctrl Pts',(76.2959066074933,341.189864686684,47.3035443132344));
#39961=CARTESIAN_POINT('Ctrl Pts',(79.5033506359083,340.798163072644,48.9021958940077));
#39962=CARTESIAN_POINT('Ctrl Pts',(80.6213960283487,340.512539463381,51.440510235231));
#39963=CARTESIAN_POINT('Ctrl Pts',(80.636192681801,340.332993858894,53.0268230851199));
#39964=CARTESIAN_POINT('Origin',(74.9879498948689,423.667006141107,53.0228109606356));
#39965=CARTESIAN_POINT('',(80.633451427705,349.667006141107,53.0191888592032));
#39966=CARTESIAN_POINT('',(80.6314498948689,348.332993858894,53.0228109606318));
#39967=CARTESIAN_POINT('',(80.6314498948689,423.667006141107,53.0228109606222));
#39968=CARTESIAN_POINT('Ctrl Pts',(80.633451427705,349.667006141107,53.0191888592032));
#39969=CARTESIAN_POINT('Ctrl Pts',(80.6300364855632,349.607701095854,53.5446842132234));
#39970=CARTESIAN_POINT('Ctrl Pts',(80.415720372531,349.442318045826,55.0131729290342));
#39971=CARTESIAN_POINT('Ctrl Pts',(78.7083308692968,349.064778986245,58.0158803567333));
#39972=CARTESIAN_POINT('Ctrl Pts',(73.6120037259175,348.534388962364,59.557185057255));
#39973=CARTESIAN_POINT('Ctrl Pts',(68.7442020401091,347.897920933707,55.3892069645249));
#39974=CARTESIAN_POINT('Ctrl Pts',(69.6243212317588,347.26145290505,49.0539647712928));
#39975=CARTESIAN_POINT('Ctrl Pts',(75.4254018924481,346.624984876393,46.3600147705323));
#39976=CARTESIAN_POINT('Ctrl Pts',(79.9422591554384,346.093502621745,49.2296317104394));
#39977=CARTESIAN_POINT('Ctrl Pts',(80.6210267320052,345.77417637665,52.0686245247025));
#39978=CARTESIAN_POINT('Ctrl Pts',(80.6202875021214,345.667006141106,53.0217977730345));
#39979=CARTESIAN_POINT('Ctrl Pts',(80.6314498948689,348.332993858894,53.0228109606315));
#39980=CARTESIAN_POINT('Ctrl Pts',(80.6314498948701,348.140209036291,54.7318077489505));
#39981=CARTESIAN_POINT('Ctrl Pts',(79.806065919266,347.947424213689,56.4221521097309));
#39982=CARTESIAN_POINT('Ctrl Pts',(78.4584055093397,347.754639391087,57.4730952299815));
#39983=CARTESIAN_POINT('Ctrl Pts',(77.1107450994134,347.561854568484,58.5240383502321));
#39984=CARTESIAN_POINT('Ctrl Pts',(75.2702256751573,347.369069745882,58.9126397065625));
#39985=CARTESIAN_POINT('Ctrl Pts',(73.6127451626995,347.176284923279,58.496192382994));
#39986=CARTESIAN_POINT('Ctrl Pts',(71.9552646502417,346.983500100677,58.0797450594256));
#39987=CARTESIAN_POINT('Ctrl Pts',(70.5170033810699,346.790715278075,56.8673394809138));
#39988=CARTESIAN_POINT('Ctrl Pts',(69.8261371496105,346.597930455472,55.3042099684569));
#39989=CARTESIAN_POINT('Ctrl Pts',(69.1352709181512,346.40514563287,53.7410804559999));
#39990=CARTESIAN_POINT('Ctrl Pts',(69.206880305491,346.212360810267,51.8613477992503));
#39991=CARTESIAN_POINT('Ctrl Pts',(70.0146680415462,346.019575987665,50.3553102844574));
#39992=CARTESIAN_POINT('Ctrl Pts',(70.8224557776013,345.826791165063,48.8492727696645));
#39993=CARTESIAN_POINT('Ctrl Pts',(72.3487890589437,345.63400634246,47.7498049531856));
#39994=CARTESIAN_POINT('Ctrl Pts',(74.0331492157652,345.441221519858,47.4606667775724));
#39995=CARTESIAN_POINT('Ctrl Pts',(75.7175093725867,345.248436697255,47.1715286019592));
#39996=CARTESIAN_POINT('Ctrl Pts',(77.5231293307889,345.055651874653,47.6990315230393));
#39997=CARTESIAN_POINT('Ctrl Pts',(78.7869273705916,344.862867052051,48.8494595029997));
#39998=CARTESIAN_POINT('Ctrl Pts',(79.9447859852139,344.686242654332,49.9034514424931));
#39999=CARTESIAN_POINT('Ctrl Pts',(80.6314498948679,344.509618256613,51.4570729301901));
#40000=CARTESIAN_POINT('Ctrl Pts',(80.6314498948689,344.332993858894,53.022810960632));
#40001=CARTESIAN_POINT('Origin',(74.9879498948689,423.667006141107,53.0228109606356));
#40002=CARTESIAN_POINT('',(80.6384731862346,353.667006141107,53.0238923963884));
#40003=CARTESIAN_POINT('',(80.6400049607223,352.332993858894,53.0230790512102));
#40004=CARTESIAN_POINT('',(80.6314498948689,423.667006141107,53.0228109606222));
#40005=CARTESIAN_POINT('Ctrl Pts',(80.6384731862346,353.667006141107,53.0238923963884));
#40006=CARTESIAN_POINT('Ctrl Pts',(80.6387817559317,353.653381824611,53.1442610157386));
#40007=CARTESIAN_POINT('Ctrl Pts',(80.5763907092171,353.427601498563,55.1383710357438));
#40008=CARTESIAN_POINT('Ctrl Pts',(78.2338848228655,352.989665162963,58.858492509318));
#40009=CARTESIAN_POINT('Ctrl Pts',(71.8256481706415,352.353197134305,58.9036327676611));
#40010=CARTESIAN_POINT('Ctrl Pts',(68.3359414908884,351.716729105649,53.5434228158304));
#40011=CARTESIAN_POINT('Ctrl Pts',(70.9492443786796,351.080261076991,47.7055677769413));
#40012=CARTESIAN_POINT('Ctrl Pts',(77.2864777741945,350.443793048335,46.7531983504033));
#40013=CARTESIAN_POINT('Ctrl Pts',(80.3981784562209,349.972708069706,50.314162070502));
#40014=CARTESIAN_POINT('Ctrl Pts',(80.6361447390397,349.71377910063,52.604738911161));
#40015=CARTESIAN_POINT('Ctrl Pts',(80.633451427705,349.667006141107,53.0191888592032));
#40016=CARTESIAN_POINT('Ctrl Pts',(80.6400049607223,352.332993858894,53.0230790512102));
#40017=CARTESIAN_POINT('Ctrl Pts',(80.6400149165888,352.331347635322,53.0376053373019));
#40018=CARTESIAN_POINT('Ctrl Pts',(80.6333577017943,352.117545402199,54.9241879694794));
#40019=CARTESIAN_POINT('Ctrl Pts',(78.5557872721241,351.691587159524,58.6668125349179));
#40020=CARTESIAN_POINT('Ctrl Pts',(72.1602274420798,351.055119130866,59.0722124537102));
#40021=CARTESIAN_POINT('Ctrl Pts',(69.0135210149437,350.524729106987,54.7772841430609));
#40022=CARTESIAN_POINT('Ctrl Pts',(69.5082125339175,350.100417087881,50.9268051874641));
#40023=CARTESIAN_POINT('Ctrl Pts',(71.7094642650518,349.676105068777,47.7290874540463));
#40024=CARTESIAN_POINT('Ctrl Pts',(76.9191944454673,349.145715044897,46.6305056503264));
#40025=CARTESIAN_POINT('Ctrl Pts',(80.3288397250378,348.662651973343,50.0990734332697));
#40026=CARTESIAN_POINT('Ctrl Pts',(80.634222125101,348.391744911342,52.4971262155878));
#40027=CARTESIAN_POINT('Ctrl Pts',(80.6295592093353,348.332993858894,53.0182528091584));
#40028=CARTESIAN_POINT('Origin',(74.9879498948689,423.667006141107,53.0228109606356));
#40029=CARTESIAN_POINT('',(80.6247365158406,357.667006141107,53.0276029024325));
#40030=CARTESIAN_POINT('',(80.6314498948689,356.332993858894,53.0228109606318));
#40031=CARTESIAN_POINT('',(80.6314498948689,423.667006141107,53.0228109606222));
#40032=CARTESIAN_POINT('Ctrl Pts',(80.6247365158406,357.667006141107,53.0276029024325));
#40033=CARTESIAN_POINT('Ctrl Pts',(80.6298460758694,357.592984548592,53.6847268621822));
#40034=CARTESIAN_POINT('Ctrl Pts',(80.221616630998,357.306806946524,56.2196666780232));
#40035=CARTESIAN_POINT('Ctrl Pts',(76.4566386365349,356.808473334904,59.5364252185682));
#40036=CARTESIAN_POINT('Ctrl Pts',(70.3070805562703,356.172005306247,57.777778336482));
#40037=CARTESIAN_POINT('Ctrl Pts',(68.4520736285264,355.53553727759,51.6565976712477));
#40038=CARTESIAN_POINT('Ctrl Pts',(72.6121732175607,354.899069248933,46.7820611760358));
#40039=CARTESIAN_POINT('Ctrl Pts',(77.886236228337,354.368679225053,47.5117391122231));
#40040=CARTESIAN_POINT('Ctrl Pts',(80.2290853076505,353.957991522444,50.4493699279292));
#40041=CARTESIAN_POINT('Ctrl Pts',(80.6363792531857,353.759459829387,52.2070791040902));
#40042=CARTESIAN_POINT('Ctrl Pts',(80.6384731862346,353.667006141107,53.0238923963884));
#40043=CARTESIAN_POINT('Ctrl Pts',(80.6287180057221,356.332993858894,53.0272649993926));
#40044=CARTESIAN_POINT('Ctrl Pts',(80.6334767749213,356.270950359303,53.5777950154488));
#40045=CARTESIAN_POINT('Ctrl Pts',(80.3064394217103,355.99675085016,56.0057811601085));
#40046=CARTESIAN_POINT('Ctrl Pts',(76.8197874993998,355.510395331466,59.4443095151045));
#40047=CARTESIAN_POINT('Ctrl Pts',(71.6277284938853,354.980005307585,58.2650326962652));
#40048=CARTESIAN_POINT('Ctrl Pts',(69.4763532374749,354.55569328848,55.0335481469374));
#40049=CARTESIAN_POINT('Ctrl Pts',(69.0414601665085,354.131381269376,51.175857658671));
#40050=CARTESIAN_POINT('Ctrl Pts',(72.2544222487035,353.600991245494,46.9302663935378));
#40051=CARTESIAN_POINT('Ctrl Pts',(78.6263988188862,352.966169440409,47.4335374279615));
#40052=CARTESIAN_POINT('Ctrl Pts',(80.6387318606642,352.543503644875,51.1655395103507));
#40053=CARTESIAN_POINT('Ctrl Pts',(80.6400049607223,352.332993858894,53.0230790512102));
#40054=CARTESIAN_POINT('Origin',(74.9879498948689,423.667006141107,53.0228109606356));
#40055=CARTESIAN_POINT('',(80.6248445340874,361.667006141107,53.0177036455054));
#40056=CARTESIAN_POINT('',(80.6314498948689,360.332993858894,53.0228109606317));
#40057=CARTESIAN_POINT('',(80.6314498948689,423.667006141107,53.0228109606222));
#40058=CARTESIAN_POINT('Ctrl Pts',(80.6248445340874,361.667006141107,53.0177036455054));
#40059=CARTESIAN_POINT('Ctrl Pts',(80.6175315928956,361.532587272572,54.2131392197305));
#40060=CARTESIAN_POINT('Ctrl Pts',(79.6600387342728,361.186012394485,57.3078556520816));
#40061=CARTESIAN_POINT('Ctrl Pts',(74.5718700069468,360.627281506846,59.6821750471879));
#40062=CARTESIAN_POINT('Ctrl Pts',(69.1575163315875,359.990813478189,56.2770792017615));
#40063=CARTESIAN_POINT('Ctrl Pts',(69.1020116217968,359.354345449532,49.8689239398295));
#40064=CARTESIAN_POINT('Ctrl Pts',(73.5623855454864,358.823955425652,46.9614791866025));
#40065=CARTESIAN_POINT('Ctrl Pts',(77.3801004030129,358.399643406547,47.665724281053));
#40066=CARTESIAN_POINT('Ctrl Pts',(79.9167858955864,358.049352979957,49.6244288636624));
#40067=CARTESIAN_POINT('Ctrl Pts',(80.615201377891,357.805140558144,51.801319705639));
#40068=CARTESIAN_POINT('Ctrl Pts',(80.6247365158406,357.667006141107,53.0276029024325));
#40069=CARTESIAN_POINT('Ctrl Pts',(80.6314498948689,360.332993858894,53.0228109606319));
#40070=CARTESIAN_POINT('Ctrl Pts',(80.63144989487,360.140209036291,54.7318077489509));
#40071=CARTESIAN_POINT('Ctrl Pts',(79.8060659192657,359.947424213689,56.4221521097313));
#40072=CARTESIAN_POINT('Ctrl Pts',(78.4584055093394,359.754639391086,57.4730952299818));
#40073=CARTESIAN_POINT('Ctrl Pts',(77.110745099413,359.561854568484,58.5240383502323));
#40074=CARTESIAN_POINT('Ctrl Pts',(75.2702256751568,359.369069745882,58.9126397065626));
#40075=CARTESIAN_POINT('Ctrl Pts',(73.612745162699,359.176284923279,58.4961923829939));
#40076=CARTESIAN_POINT('Ctrl Pts',(71.9552646502412,358.983500100677,58.0797450594253));
#40077=CARTESIAN_POINT('Ctrl Pts',(70.5170033810695,358.790715278075,56.8673394809134));
#40078=CARTESIAN_POINT('Ctrl Pts',(69.8261371496103,358.597930455472,55.3042099684563));
#40079=CARTESIAN_POINT('Ctrl Pts',(69.1352709181511,358.40514563287,53.7410804559993));
#40080=CARTESIAN_POINT('Ctrl Pts',(69.2068803054912,358.212360810267,51.8613477992496));
#40081=CARTESIAN_POINT('Ctrl Pts',(70.0146680415465,358.019575987665,50.3553102844568));
#40082=CARTESIAN_POINT('Ctrl Pts',(70.8224557776019,357.826791165063,48.849272769664));
#40083=CARTESIAN_POINT('Ctrl Pts',(72.3487890589444,357.63400634246,47.7498049531853));
#40084=CARTESIAN_POINT('Ctrl Pts',(74.033149215766,357.441221519858,47.4606667775723));
#40085=CARTESIAN_POINT('Ctrl Pts',(75.7175093725876,357.248436697255,47.1715286019593));
#40086=CARTESIAN_POINT('Ctrl Pts',(77.5231293307897,357.055651874653,47.6990315230396));
#40087=CARTESIAN_POINT('Ctrl Pts',(78.7869273705922,356.862867052051,48.8494595030002));
#40088=CARTESIAN_POINT('Ctrl Pts',(79.9447859852141,356.686242654332,49.9034514424936));
#40089=CARTESIAN_POINT('Ctrl Pts',(80.6314498948678,356.509618256613,51.4570729301902));
#40090=CARTESIAN_POINT('Ctrl Pts',(80.6314498948689,356.332993858894,53.0228109606318));
#40091=CARTESIAN_POINT('Origin',(74.9879498948689,423.667006141107,53.0228109606356));
#40092=CARTESIAN_POINT('',(80.6397711584222,365.667006141107,53.0208691915594));
#40093=CARTESIAN_POINT('',(80.6370474885153,364.332993858893,53.0191872378647));
#40094=CARTESIAN_POINT('',(80.6314498948689,423.667006141107,53.0228109606222));
#40095=CARTESIAN_POINT('Ctrl Pts',(80.6397711584222,365.667006141107,53.0208691915594));
#40096=CARTESIAN_POINT('Ctrl Pts',(80.6296050747201,365.472189996553,54.7412732581942));
#40097=CARTESIAN_POINT('Ctrl Pts',(78.8683419814859,365.065217842446,58.3501341198079));
#40098=CARTESIAN_POINT('Ctrl Pts',(72.7199018846829,364.446089678788,59.302952324055));
#40099=CARTESIAN_POINT('Ctrl Pts',(68.4759904733059,363.809621650131,54.5012077904277));
#40100=CARTESIAN_POINT('Ctrl Pts',(69.9370688277395,363.279231626249,49.3813034383522));
#40101=CARTESIAN_POINT('Ctrl Pts',(73.2812266717887,362.854919607146,47.4096249147279));
#40102=CARTESIAN_POINT('Ctrl Pts',(77.1569110752008,362.43060758804,47.1860666637397));
#40103=CARTESIAN_POINT('Ctrl Pts',(80.19079143513,362.034636432695,49.7542817042191));
#40104=CARTESIAN_POINT('Ctrl Pts',(80.6290737553782,361.744743282125,52.3263591577539));
#40105=CARTESIAN_POINT('Ctrl Pts',(80.6248445340874,361.667006141107,53.0177036455054));
#40106=CARTESIAN_POINT('Ctrl Pts',(80.6370474885153,364.332993858894,53.0191872378647));
#40107=CARTESIAN_POINT('Ctrl Pts',(80.6226904770127,364.150155807264,54.6340249277856));
#40108=CARTESIAN_POINT('Ctrl Pts',(79.4660425813718,363.86123975086,57.1999674524242));
#40109=CARTESIAN_POINT('Ctrl Pts',(76.2070166523586,363.466245689677,58.7616817543507));
#40110=CARTESIAN_POINT('Ctrl Pts',(72.3264382459639,363.041933670573,58.6520500150618));
#40111=CARTESIAN_POINT('Ctrl Pts',(68.572635003179,362.511543646692,54.8761882926657));
#40112=CARTESIAN_POINT('Ctrl Pts',(69.9668979799986,361.875075618035,48.6213049695892));
#40113=CARTESIAN_POINT('Ctrl Pts',(75.9735829643599,361.238607589378,46.4236610182017));
#40114=CARTESIAN_POINT('Ctrl Pts',(80.094404819463,360.724580336331,49.5385639086073));
#40115=CARTESIAN_POINT('Ctrl Pts',(80.6259624255451,360.422709092836,52.2223601240696));
#40116=CARTESIAN_POINT('Ctrl Pts',(80.622923341824,360.332993858894,53.0210345647259));
#40117=CARTESIAN_POINT('Origin',(74.9879498948689,423.667006141107,53.0228109606356));
#40118=CARTESIAN_POINT('',(80.6326307703874,369.667006141107,53.0277774696284));
#40119=CARTESIAN_POINT('',(80.6332290564755,368.332993858894,53.0268706649991));
#40120=CARTESIAN_POINT('',(80.6314498948689,423.667006141107,53.0228109606222));
#40121=CARTESIAN_POINT('Ctrl Pts',(80.6326307703874,369.667006141107,53.0277774696284));
#40122=CARTESIAN_POINT('Ctrl Pts',(80.6360347096095,369.623948730086,53.409029713798));
#40123=CARTESIAN_POINT('Ctrl Pts',(80.4262099310797,369.368735309512,55.6650143801684));
#40124=CARTESIAN_POINT('Ctrl Pts',(77.3936427899844,368.901365879386,59.2515234291501));
#40125=CARTESIAN_POINT('Ctrl Pts',(71.0408633993679,368.26489785073,58.4090694850156));
#40126=CARTESIAN_POINT('Ctrl Pts',(68.7867101717712,367.734507826848,53.5854853654303));
#40127=CARTESIAN_POINT('Ctrl Pts',(70.0186562199422,367.310195807744,49.904015982041));
#40128=CARTESIAN_POINT('Ctrl Pts',(72.7981944809444,366.885883788639,47.1938361094012));
#40129=CARTESIAN_POINT('Ctrl Pts',(78.1220664110398,366.355493764758,47.126321635835));
#40130=CARTESIAN_POINT('Ctrl Pts',(80.565317102736,365.913841880656,50.8418338582383));
#40131=CARTESIAN_POINT('Ctrl Pts',(80.6406760039593,365.684346006105,52.8677423840958));
#40132=CARTESIAN_POINT('Ctrl Pts',(80.6397711584222,365.667006141107,53.0208691915594));
#40133=CARTESIAN_POINT('Ctrl Pts',(80.6332290564755,368.332993858894,53.0268706649991));
#40134=CARTESIAN_POINT('Ctrl Pts',(80.6356848743043,368.301914540797,53.3018404448554));
#40135=CARTESIAN_POINT('Ctrl Pts',(80.5560664743386,368.164757217925,54.5142151899356));
#40136=CARTESIAN_POINT('Ctrl Pts',(79.6714791919269,367.921521890276,56.5562674935186));
#40137=CARTESIAN_POINT('Ctrl Pts',(76.6697640348178,367.497209871172,59.0180989260132));
#40138=CARTESIAN_POINT('Ctrl Pts',(71.359714904182,366.96681984729,58.6288062823227));
#40139=CARTESIAN_POINT('Ctrl Pts',(68.3108789861652,366.330351818634,52.9921286989546));
#40140=CARTESIAN_POINT('Ctrl Pts',(71.4048542721186,365.693883789976,47.3941629641248));
#40141=CARTESIAN_POINT('Ctrl Pts',(77.7862076759328,365.05741576132,46.9603056442045));
#40142=CARTESIAN_POINT('Ctrl Pts',(80.506338760825,364.603785784292,50.6294404889205));
#40143=CARTESIAN_POINT('Ctrl Pts',(80.6393496255999,364.362311816816,52.7602491064219));
#40144=CARTESIAN_POINT('Ctrl Pts',(80.6370474885153,364.332993858894,53.0191872378647));
#40145=CARTESIAN_POINT('Origin',(74.9879498948689,423.667006141107,53.0228109606356));
#40146=CARTESIAN_POINT('',(80.6223565140898,373.667006141107,53.0230511363488));
#40147=CARTESIAN_POINT('',(80.6269596911125,372.332993858894,53.0243158257365));
#40148=CARTESIAN_POINT('',(80.6314498948689,423.667006141107,53.0228109606222));
#40149=CARTESIAN_POINT('Ctrl Pts',(80.6223565140898,373.667006141107,53.0230511363488));
#40150=CARTESIAN_POINT('Ctrl Pts',(80.623318383652,373.563551454066,53.9434812983077));
#40151=CARTESIAN_POINT('Ctrl Pts',(79.9750770611082,373.247940757473,56.7508149175562));
#40152=CARTESIAN_POINT('Ctrl Pts',(75.5398292911409,372.720174051328,59.677636414875));
#40153=CARTESIAN_POINT('Ctrl Pts',(70.6749913177946,372.189784027447,57.5139538999746));
#40154=CARTESIAN_POINT('Ctrl Pts',(69.1910655822406,371.765472008342,53.9266328524801));
#40155=CARTESIAN_POINT('Ctrl Pts',(69.5124694584528,371.341159989238,50.0578336285873));
#40156=CARTESIAN_POINT('Ctrl Pts',(73.4877077677736,370.810769965357,46.5158495918775));
#40157=CARTESIAN_POINT('Ctrl Pts',(79.2397454683978,370.217359347721,48.1323470424996));
#40158=CARTESIAN_POINT('Ctrl Pts',(80.6192625408933,369.836104739638,51.5304923647657));
#40159=CARTESIAN_POINT('Ctrl Pts',(80.6326307703874,369.667006141107,53.0277774696284));
#40160=CARTESIAN_POINT('Ctrl Pts',(80.6269596911125,372.332993858894,53.0243158257365));
#40161=CARTESIAN_POINT('Ctrl Pts',(80.6287591076907,372.241517264778,53.837559733299));
#40162=CARTESIAN_POINT('Ctrl Pts',(80.071596577785,371.93788466111,56.5341906247379));
#40163=CARTESIAN_POINT('Ctrl Pts',(75.9246488708189,371.422096047889,59.6344573307068));
#40164=CARTESIAN_POINT('Ctrl Pts',(69.926659556592,370.785628019232,57.377986896543));
#40165=CARTESIAN_POINT('Ctrl Pts',(68.5918611198335,370.149159990575,51.1227317801111));
#40166=CARTESIAN_POINT('Ctrl Pts',(73.125273998855,369.512691961918,46.610739857829));
#40167=CARTESIAN_POINT('Ctrl Pts',(79.0768627736854,368.907303251357,47.9272954751586));
#40168=CARTESIAN_POINT('Ctrl Pts',(80.6189207834984,368.51407055035,51.4248207798587));
#40169=CARTESIAN_POINT('Ctrl Pts',(80.6332290564755,368.332993858894,53.0268706649991));
#40170=CARTESIAN_POINT('Origin',(74.9879498948689,423.667006141107,53.0228109606356));
#40171=CARTESIAN_POINT('',(80.6318252954934,377.667006141106,53.0173586745867));
#40172=CARTESIAN_POINT('',(80.625604522174,376.332993858894,53.0187133256936));
#40173=CARTESIAN_POINT('',(80.6314498948689,423.667006141107,53.0228109606222));
#40174=CARTESIAN_POINT('Ctrl Pts',(80.6318252954934,377.667006141107,53.0173586745867));
#40175=CARTESIAN_POINT('Ctrl Pts',(80.6180275057674,377.503154178046,54.4701804610813));
#40176=CARTESIAN_POINT('Ctrl Pts',(79.3046541470043,377.127146205434,57.8270528744592));
#40177=CARTESIAN_POINT('Ctrl Pts',(74.676644657417,376.645060228046,59.2417389742301));
#40178=CARTESIAN_POINT('Ctrl Pts',(71.2039784868037,376.220748208941,57.5063722827453));
#40179=CARTESIAN_POINT('Ctrl Pts',(68.9097584028537,375.796436189837,54.3746855019773));
#40180=CARTESIAN_POINT('Ctrl Pts',(69.5884755901131,375.266046165955,49.0938225505349));
#40181=CARTESIAN_POINT('Ctrl Pts',(75.3832511001032,374.629578137299,46.3573811711787));
#40182=CARTESIAN_POINT('Ctrl Pts',(79.9227890716234,374.096564795682,49.2006142598981));
#40183=CARTESIAN_POINT('Ctrl Pts',(80.6213458639541,373.775707463618,52.0559419724561));
#40184=CARTESIAN_POINT('Ctrl Pts',(80.6223565140898,373.667006141107,53.0230511363488));
#40185=CARTESIAN_POINT('Ctrl Pts',(80.625604522174,376.332993858894,53.0187133256936));
#40186=CARTESIAN_POINT('Ctrl Pts',(80.6145961714162,376.181119988758,54.3665391394491));
#40187=CARTESIAN_POINT('Ctrl Pts',(79.4615473568344,375.817090109071,57.6115233426936));
#40188=CARTESIAN_POINT('Ctrl Pts',(74.0224987859417,375.240904219831,59.6297861745523));
#40189=CARTESIAN_POINT('Ctrl Pts',(68.9129848210706,374.604436191174,55.7823493029185));
#40190=CARTESIAN_POINT('Ctrl Pts',(69.3770612241408,373.967968162517,49.4031223489269));
#40191=CARTESIAN_POINT('Ctrl Pts',(75.0088003293896,373.331500133859,46.3451738071356));
#40192=CARTESIAN_POINT('Ctrl Pts',(79.6701661503711,372.80111010998,48.9180786276028));
#40193=CARTESIAN_POINT('Ctrl Pts',(80.5885727818433,372.46827468499,51.8214716448624));
#40194=CARTESIAN_POINT('Ctrl Pts',(80.6266724698768,372.347595269554,52.8945065736976));
#40195=CARTESIAN_POINT('Ctrl Pts',(80.6269596911125,372.332993858894,53.0243158257365));
#40196=CARTESIAN_POINT('Origin',(74.9879498948689,423.667006141107,53.0228109606356));
#40197=CARTESIAN_POINT('',(80.6405446979746,381.667006141107,53.0261965417875));
#40198=CARTESIAN_POINT('',(80.6413661730645,380.332993858894,53.021596719646));
#40199=CARTESIAN_POINT('',(80.6314498948689,423.667006141107,53.0228109606222));
#40200=CARTESIAN_POINT('Ctrl Pts',(80.6405446979746,381.667006141107,53.0261965417875));
#40201=CARTESIAN_POINT('Ctrl Pts',(80.6410056141965,381.654912911579,53.1329056124629));
#40202=CARTESIAN_POINT('Ctrl Pts',(80.5894057523151,381.4306636725,55.1109627377459));
#40203=CARTESIAN_POINT('Ctrl Pts',(78.8308391867579,381.100336428644,57.9222168919113));
#40204=CARTESIAN_POINT('Ctrl Pts',(75.0710571136364,380.67602440954,58.8891432847));
#40205=CARTESIAN_POINT('Ctrl Pts',(71.2853928743543,380.251712390435,58.0291118004746));
#40206=CARTESIAN_POINT('Ctrl Pts',(68.3350139784818,379.721322366554,53.5970203186811));
#40207=CARTESIAN_POINT('Ctrl Pts',(70.9156937160722,379.084854337897,47.7312188622881));
#40208=CARTESIAN_POINT('Ctrl Pts',(77.2345122810668,378.448386309241,46.7400400786665));
#40209=CARTESIAN_POINT('Ctrl Pts',(80.3960885854519,377.975770243644,50.2843313906369));
#40210=CARTESIAN_POINT('Ctrl Pts',(80.6358929249802,377.715310187599,52.589062486923));
#40211=CARTESIAN_POINT('Ctrl Pts',(80.6318252954934,377.667006141107,53.0173586745867));
#40212=CARTESIAN_POINT('Ctrl Pts',(80.6413661730645,380.332993858894,53.021596719646));
#40213=CARTESIAN_POINT('Ctrl Pts',(80.6413665147454,380.332878722291,53.0226120523518));
#40214=CARTESIAN_POINT('Ctrl Pts',(80.6414404313821,380.120607576137,54.8945283089342));
#40215=CARTESIAN_POINT('Ctrl Pts',(78.5914140932141,379.696180420429,58.6441331442757));
#40216=CARTESIAN_POINT('Ctrl Pts',(72.2108730876569,379.059712391772,59.0897786478119));
#40217=CARTESIAN_POINT('Ctrl Pts',(68.3782131572467,378.423244363116,53.9691711353926));
#40218=CARTESIAN_POINT('Ctrl Pts',(70.6249796526406,377.786776334458,47.9675401113284));
#40219=CARTESIAN_POINT('Ctrl Pts',(75.8314238903965,377.256386310578,46.8534894251665));
#40220=CARTESIAN_POINT('Ctrl Pts',(79.1424775432099,376.832074291473,48.8802680501344));
#40221=CARTESIAN_POINT('Ctrl Pts',(80.4376648879746,376.559636142504,51.0099478466897));
#40222=CARTESIAN_POINT('Ctrl Pts',(80.6299739830598,376.393275998311,52.4837310832435));
#40223=CARTESIAN_POINT('Ctrl Pts',(80.625604522174,376.332993858894,53.0187133256936));
#40224=CARTESIAN_POINT('Origin',(74.9879498948689,423.667006141107,53.0228109606356));
#40225=CARTESIAN_POINT('',(80.6230176733859,385.667006141107,53.0259542642868));
#40226=CARTESIAN_POINT('',(80.6314498948689,384.332993858894,53.0228109606314));
#40227=CARTESIAN_POINT('',(80.6314498948689,423.667006141107,53.0228109606222));
#40228=CARTESIAN_POINT('Ctrl Pts',(80.6230176733859,385.667006141107,53.0259542642868));
#40229=CARTESIAN_POINT('Ctrl Pts',(80.6270946479354,385.59451563556,53.6699647111595));
#40230=CARTESIAN_POINT('Ctrl Pts',(80.3763420788995,385.415947125237,55.2537571332483));
#40231=CARTESIAN_POINT('Ctrl Pts',(78.897412769893,385.131300610139,57.3973808566349));
#40232=CARTESIAN_POINT('Ctrl Pts',(75.4752995936722,384.706988591033,59.2304245810384));
#40233=CARTESIAN_POINT('Ctrl Pts',(70.3415256590186,384.176598567153,57.8188525070491));
#40234=CARTESIAN_POINT('Ctrl Pts',(68.4435630952913,383.540130538496,51.6979642757119));
#40235=CARTESIAN_POINT('Ctrl Pts',(72.5643111612702,382.903662509839,46.8062019332478));
#40236=CARTESIAN_POINT('Ctrl Pts',(78.788125715371,382.279287710709,47.6025595677669));
#40237=CARTESIAN_POINT('Ctrl Pts',(80.632919590016,381.867068921132,51.2608688197568));
#40238=CARTESIAN_POINT('Ctrl Pts',(80.6405446979746,381.667006141107,53.0261965417875));
#40239=CARTESIAN_POINT('Ctrl Pts',(80.6285307903321,384.332993858894,53.0278704034178));
#40240=CARTESIAN_POINT('Ctrl Pts',(80.6332236772202,384.272481446272,53.5652251748871));
#40241=CARTESIAN_POINT('Ctrl Pts',(80.3164791190338,383.999813024097,55.9810146677916));
#40242=CARTESIAN_POINT('Ctrl Pts',(76.8695434714302,383.514988592372,59.4243621885054));
#40243=CARTESIAN_POINT('Ctrl Pts',(70.6181705596548,382.878520563713,58.0714985012323));
#40244=CARTESIAN_POINT('Ctrl Pts',(68.3790371462131,382.242052535058,52.0670154934588));
#40245=CARTESIAN_POINT('Ctrl Pts',(71.5793749741399,381.711662511176,47.8118999463395));
#40246=CARTESIAN_POINT('Ctrl Pts',(75.4082269213871,381.287350492072,47.1709626229601));
#40247=CARTESIAN_POINT('Ctrl Pts',(79.1051881256536,380.863153609569,48.3521518125064));
#40248=CARTESIAN_POINT('Ctrl Pts',(80.6407369179058,380.545034731844,51.1517132196232));
#40249=CARTESIAN_POINT('Ctrl Pts',(80.6413661730645,380.332993858894,53.021596719646));
#40250=CARTESIAN_POINT('Origin',(74.9879498948689,423.667006141107,53.0228109606356));
#40251=CARTESIAN_POINT('',(80.6280910915538,389.667006141107,53.0202293524412));
#40252=CARTESIAN_POINT('',(80.6314498948689,388.332993858894,53.0228109606314));
#40253=CARTESIAN_POINT('',(80.6314498948689,423.667006141107,53.0228109606222));
#40254=CARTESIAN_POINT('Ctrl Pts',(80.6280910915538,389.667006141107,53.0202293524411));
#40255=CARTESIAN_POINT('Ctrl Pts',(80.6271443157921,389.640196364317,53.2584401382313));
#40256=CARTESIAN_POINT('Ctrl Pts',(80.5499860677044,389.507308582751,54.4398090922248));
#40257=CARTESIAN_POINT('Ctrl Pts',(79.4264024191887,389.162264791632,57.3899743166933));
#40258=CARTESIAN_POINT('Ctrl Pts',(74.6248094448821,388.631874767752,59.6905993277034));
#40259=CARTESIAN_POINT('Ctrl Pts',(69.1782161333895,387.995406739095,56.3138914734408));
#40260=CARTESIAN_POINT('Ctrl Pts',(69.0817056595131,387.358938710438,49.9185346290693));
#40261=CARTESIAN_POINT('Ctrl Pts',(74.4039894636263,386.72247068178,46.3712541852796));
#40262=CARTESIAN_POINT('Ctrl Pts',(79.6053973880414,386.15849315867,48.6495978495524));
#40263=CARTESIAN_POINT('Ctrl Pts',(80.615162676363,385.806671645112,51.7851566871539));
#40264=CARTESIAN_POINT('Ctrl Pts',(80.6230176733859,385.667006141107,53.0259542642868));
#40265=CARTESIAN_POINT('Ctrl Pts',(80.6314498948689,388.332993858894,53.0228109606315));
#40266=CARTESIAN_POINT('Ctrl Pts',(80.6314498948701,388.140209036291,54.7318077489505));
#40267=CARTESIAN_POINT('Ctrl Pts',(79.806065919266,387.947424213689,56.4221521097309));
#40268=CARTESIAN_POINT('Ctrl Pts',(78.4584055093398,387.754639391087,57.4730952299815));
#40269=CARTESIAN_POINT('Ctrl Pts',(77.1107450994135,387.561854568484,58.5240383502321));
#40270=CARTESIAN_POINT('Ctrl Pts',(75.2702256751574,387.369069745882,58.9126397065625));
#40271=CARTESIAN_POINT('Ctrl Pts',(73.6127451626996,387.176284923279,58.4961923829941));
#40272=CARTESIAN_POINT('Ctrl Pts',(71.9552646502418,386.983500100677,58.0797450594256));
#40273=CARTESIAN_POINT('Ctrl Pts',(70.51700338107,386.790715278075,56.867339480914));
#40274=CARTESIAN_POINT('Ctrl Pts',(69.8261371496106,386.597930455472,55.3042099684571));
#40275=CARTESIAN_POINT('Ctrl Pts',(69.1352709181512,386.40514563287,53.7410804560002));
#40276=CARTESIAN_POINT('Ctrl Pts',(69.206880305491,386.212360810268,51.8613477992506));
#40277=CARTESIAN_POINT('Ctrl Pts',(70.014668041546,386.019575987665,50.3553102844577));
#40278=CARTESIAN_POINT('Ctrl Pts',(70.8224557776011,385.826791165063,48.8492727696647));
#40279=CARTESIAN_POINT('Ctrl Pts',(72.3487890589434,385.63400634246,47.7498049531858));
#40280=CARTESIAN_POINT('Ctrl Pts',(74.0331492157648,385.441221519858,47.4606667775725));
#40281=CARTESIAN_POINT('Ctrl Pts',(75.7175093725863,385.248436697256,47.1715286019592));
#40282=CARTESIAN_POINT('Ctrl Pts',(77.5231293307885,385.055651874653,47.6990315230391));
#40283=CARTESIAN_POINT('Ctrl Pts',(78.7869273705912,384.862867052051,48.8494595029993));
#40284=CARTESIAN_POINT('Ctrl Pts',(79.9447859852136,384.686242654332,49.9034514424927));
#40285=CARTESIAN_POINT('Ctrl Pts',(80.6314498948677,384.509618256613,51.4570729301894));
#40286=CARTESIAN_POINT('Ctrl Pts',(80.6314498948689,384.332993858894,53.0228109606314));
#40287=CARTESIAN_POINT('Origin',(74.9879498948689,423.667006141107,53.0228109606356));
#40288=CARTESIAN_POINT('',(80.6360923571988,393.667006141107,53.0197627911133));
#40289=CARTESIAN_POINT('',(80.6356989504312,392.332993858894,53.0186124760575));
#40290=CARTESIAN_POINT('',(80.6314498948689,423.667006141107,53.0228109606222));
#40291=CARTESIAN_POINT('Ctrl Pts',(80.6360923571988,393.667006141107,53.0197627911133));
#40292=CARTESIAN_POINT('Ctrl Pts',(80.6237110197019,393.473721083521,54.7279555626006));
#40293=CARTESIAN_POINT('Ctrl Pts',(78.8984604558714,393.068280016383,58.3253991383234));
#40294=CARTESIAN_POINT('Ctrl Pts',(72.7596690106956,392.450682939694,59.3171720578613));
#40295=CARTESIAN_POINT('Ctrl Pts',(68.4931906324375,391.814214911036,54.5519789152622));
#40296=CARTESIAN_POINT('Ctrl Pts',(70.1854506547193,391.177746882379,48.3838220223643));
#40297=CARTESIAN_POINT('Ctrl Pts',(76.3032611663828,390.541278853722,46.4759621802336));
#40298=CARTESIAN_POINT('Ctrl Pts',(80.1713126028281,390.037698606631,49.7306407766893));
#40299=CARTESIAN_POINT('Ctrl Pts',(80.6308904150066,389.746274369093,52.3159136460942));
#40300=CARTESIAN_POINT('Ctrl Pts',(80.6280910915538,389.667006141107,53.0202293524411));
#40301=CARTESIAN_POINT('Ctrl Pts',(80.6356989504312,392.332993858894,53.0186124760575));
#40302=CARTESIAN_POINT('Ctrl Pts',(80.6226233173025,392.151686894233,54.621714738745));
#40303=CARTESIAN_POINT('Ctrl Pts',(79.071569540894,391.75822392002,58.1232600357524));
#40304=CARTESIAN_POINT('Ctrl Pts',(73.1160470792531,391.152604936255,59.4327448560289));
#40305=CARTESIAN_POINT('Ctrl Pts',(69.3510454836729,390.622214912373,55.6680491820767));
#40306=CARTESIAN_POINT('Ctrl Pts',(69.2526248134902,390.197902893269,51.7871702535196));
#40307=CARTESIAN_POINT('Ctrl Pts',(70.9403623007099,389.773590874164,48.2911081744554));
#40308=CARTESIAN_POINT('Ctrl Pts',(75.9215609897948,389.243200850283,46.4107278533347));
#40309=CARTESIAN_POINT('Ctrl Pts',(80.082648031994,388.727642510268,49.5142379536945));
#40310=CARTESIAN_POINT('Ctrl Pts',(80.6262685739933,388.424240179805,52.2093882971212));
#40311=CARTESIAN_POINT('Ctrl Pts',(80.6232078042707,388.332993858894,53.0209321700845));
#40312=CARTESIAN_POINT('Origin',(74.9879498948689,423.667006141107,53.0228109606356));
#40313=CARTESIAN_POINT('',(80.6337031614845,397.667006141107,53.0276437365256));
#40314=CARTESIAN_POINT('',(80.6372725134855,396.332993858893,53.0262406841596));
#40315=CARTESIAN_POINT('',(80.6314498948689,423.667006141107,53.0228109606222));
#40316=CARTESIAN_POINT('Ctrl Pts',(80.6337031614845,397.667006141107,53.0276437365256));
#40317=CARTESIAN_POINT('Ctrl Pts',(80.6373890898133,397.625479817054,53.3949129559387));
#40318=CARTESIAN_POINT('Ctrl Pts',(80.4383554548793,397.371797483449,55.6351493604705));
#40319=CARTESIAN_POINT('Ctrl Pts',(77.4329911410624,396.905959140291,59.2361828813744));
#40320=CARTESIAN_POINT('Ctrl Pts',(71.0871415122597,396.269491111636,58.436122929515));
#40321=CARTESIAN_POINT('Ctrl Pts',(68.3201615171243,395.633023082977,52.6695186301911));
#40322=CARTESIAN_POINT('Ctrl Pts',(71.6880557805561,394.996555054321,47.2174710456321));
#40323=CARTESIAN_POINT('Ctrl Pts',(77.0117036986669,394.46616503044,47.1341441224853));
#40324=CARTESIAN_POINT('Ctrl Pts',(79.8669002864431,394.041853011336,49.7644977739172));
#40325=CARTESIAN_POINT('Ctrl Pts',(80.5941763410107,393.810826049817,51.7491572431493));
#40326=CARTESIAN_POINT('Ctrl Pts',(80.637301181244,393.685877093074,52.852987230998));
#40327=CARTESIAN_POINT('Ctrl Pts',(80.6360923571988,393.667006141107,53.0197627911133));
#40328=CARTESIAN_POINT('Ctrl Pts',(80.6372725134855,396.332993858894,53.0262406841596));
#40329=CARTESIAN_POINT('Ctrl Pts',(80.6394471176278,396.303445627766,53.2874601812273));
#40330=CARTESIAN_POINT('Ctrl Pts',(80.5040174270057,396.061741387085,55.4222191120998));
#40331=CARTESIAN_POINT('Ctrl Pts',(77.7778399493888,395.607881136854,59.0897530386598));
#40332=CARTESIAN_POINT('Ctrl Pts',(72.4666579798875,395.077491112972,58.7162338035805));
#40333=CARTESIAN_POINT('Ctrl Pts',(69.8475504599716,394.653179093868,55.8507175000904));
#40334=CARTESIAN_POINT('Ctrl Pts',(68.8293227947622,394.228867074763,52.1045033700332));
#40335=CARTESIAN_POINT('Ctrl Pts',(71.3570971813203,393.698477050882,47.4185107128847));
#40336=CARTESIAN_POINT('Ctrl Pts',(77.7478064874976,393.062009022225,46.942727991698));
#40337=CARTESIAN_POINT('Ctrl Pts',(80.495439138097,392.606847958229,50.5995879290105));
#40338=CARTESIAN_POINT('Ctrl Pts',(80.6379237452377,392.363842903785,52.7458475893924));
#40339=CARTESIAN_POINT('Ctrl Pts',(80.6356989504312,392.332993858894,53.0186124760575));
#40340=CARTESIAN_POINT('Origin',(74.9879498948689,423.667006141107,53.0228109606356));
#40341=CARTESIAN_POINT('',(80.6220844309609,401.667006141107,53.022623341048));
#40342=CARTESIAN_POINT('',(80.6229913075356,400.332993858894,53.0262785622937));
#40343=CARTESIAN_POINT('',(80.6314498948689,423.667006141107,53.0228109606222));
#40344=CARTESIAN_POINT('Ctrl Pts',(80.6220844309609,401.667006141107,53.022623341048));
#40345=CARTESIAN_POINT('Ctrl Pts',(80.62301189764,401.565082541034,53.9302973036867));
#40346=CARTESIAN_POINT('Ctrl Pts',(79.9875795301274,401.25100293141,56.7266784249494));
#40347=CARTESIAN_POINT('Ctrl Pts',(75.5925088429904,400.724767312234,59.6677158495928));
#40348=CARTESIAN_POINT('Ctrl Pts',(69.7221234542071,400.088299283577,57.1283303225627));
#40349=CARTESIAN_POINT('Ctrl Pts',(68.6898157193372,399.451831254919,50.8036267423682));
#40350=CARTESIAN_POINT('Ctrl Pts',(72.6545162366563,398.921441231039,47.2498512386062));
#40351=CARTESIAN_POINT('Ctrl Pts',(76.5349782081459,398.497129211934,47.3635296330406));
#40352=CARTESIAN_POINT('Ctrl Pts',(79.6010285553096,398.114343516882,49.0560694265861));
#40353=CARTESIAN_POINT('Ctrl Pts',(80.6185578577317,397.837635826606,51.5185520258631));
#40354=CARTESIAN_POINT('Ctrl Pts',(80.6337031614845,397.667006141107,53.0276437365256));
#40355=CARTESIAN_POINT('Ctrl Pts',(80.6229913075356,400.332993858894,53.0262785622937));
#40356=CARTESIAN_POINT('Ctrl Pts',(80.6259200030489,400.243048351746,53.8269052679644));
#40357=CARTESIAN_POINT('Ctrl Pts',(80.0921841224516,399.940946835046,56.5114176061463));
#40358=CARTESIAN_POINT('Ctrl Pts',(76.817716662541,399.53276731357,58.9746115424238));
#40359=CARTESIAN_POINT('Ctrl Pts',(72.9612986351318,399.108455294466,58.5285757956383));
#40360=CARTESIAN_POINT('Ctrl Pts',(69.7360426834167,398.684143275361,56.3678740736957));
#40361=CARTESIAN_POINT('Ctrl Pts',(68.5717701362819,398.153753251481,51.1724299186502));
#40362=CARTESIAN_POINT('Ctrl Pts',(73.0847550464725,397.517285222823,46.622649502512));
#40363=CARTESIAN_POINT('Ctrl Pts',(79.0482790583822,396.910365425296,47.9016912192682));
#40364=CARTESIAN_POINT('Ctrl Pts',(80.6238334812249,396.515601637318,51.4119067555371));
#40365=CARTESIAN_POINT('Ctrl Pts',(80.6372725134855,396.332993858894,53.0262406841596));
#40366=CARTESIAN_POINT('Origin',(74.9879498948689,423.667006141107,53.0228109606356));
#40367=CARTESIAN_POINT('',(80.6319421555458,405.667006141107,53.0182025218874));
#40368=CARTESIAN_POINT('',(80.6278395430646,404.332993858894,53.0174600182511));
#40369=CARTESIAN_POINT('',(80.6314498948689,423.667006141107,53.0228109606222));
#40370=CARTESIAN_POINT('Ctrl Pts',(80.6319421555458,405.667006141107,53.0182025218874));
#40371=CARTESIAN_POINT('Ctrl Pts',(80.6183780990486,405.504685265015,54.4565202766007));
#40372=CARTESIAN_POINT('Ctrl Pts',(79.3242260166029,405.130208379371,57.7945566874126));
#40373=CARTESIAN_POINT('Ctrl Pts',(73.704367667017,404.543575484175,59.575416161524));
#40374=CARTESIAN_POINT('Ctrl Pts',(68.7776943304863,403.907107455519,55.477194252816));
#40375=CARTESIAN_POINT('Ctrl Pts',(69.4407233960758,403.376717431636,50.194338734914));
#40376=CARTESIAN_POINT('Ctrl Pts',(72.4450042051697,402.952405412533,47.7356388492427));
#40377=CARTESIAN_POINT('Ctrl Pts',(76.2412371124112,402.528093393428,46.9235284074953));
#40378=CARTESIAN_POINT('Ctrl Pts',(79.9095618030171,402.09962696962,49.1692426271042));
#40379=CARTESIAN_POINT('Ctrl Pts',(80.6210813572206,401.777238550587,52.0409558189692));
#40380=CARTESIAN_POINT('Ctrl Pts',(80.6220844309609,401.667006141107,53.022623341048));
#40381=CARTESIAN_POINT('Ctrl Pts',(80.6278395430645,404.332993858894,53.0174600182511));
#40382=CARTESIAN_POINT('Ctrl Pts',(80.6153316186647,404.182651075727,54.3503900415285));
#40383=CARTESIAN_POINT('Ctrl Pts',(79.8054162775193,403.926230287784,56.6359043562006));
#40384=CARTESIAN_POINT('Ctrl Pts',(77.0681164794659,403.563731495065,58.5085806146201));
#40385=CARTESIAN_POINT('Ctrl Pts',(73.2162245052195,403.13941947596,58.9921464057559));
#40386=CARTESIAN_POINT('Ctrl Pts',(68.9304046244017,402.609029452079,55.8330454857165));
#40387=CARTESIAN_POINT('Ctrl Pts',(69.3542790093376,401.972561423423,49.4386835020307));
#40388=CARTESIAN_POINT('Ctrl Pts',(74.9554640876222,401.336093394765,46.3505401944445));
#40389=CARTESIAN_POINT('Ctrl Pts',(79.7906837745455,400.789570873256,48.9553092231759));
#40390=CARTESIAN_POINT('Ctrl Pts',(80.619012038738,400.455204361299,51.9384533329752));
#40391=CARTESIAN_POINT('Ctrl Pts',(80.6229913075356,400.332993858894,53.0262785622937));
#40392=CARTESIAN_POINT('Origin',(74.9879498948689,423.667006141107,53.0228109606356));
#40393=CARTESIAN_POINT('',(80.6394151663028,409.667006141107,53.0244911165473));
#40394=CARTESIAN_POINT('',(80.6387414332306,408.332993858894,53.0233301036444));
#40395=CARTESIAN_POINT('',(80.6314498948689,423.667006141107,53.0228109606222));
#40396=CARTESIAN_POINT('Ctrl Pts',(80.6394151663029,409.667006141107,53.0244911165473));
#40397=CARTESIAN_POINT('Ctrl Pts',(80.6397780627352,409.656443998548,53.1177179807749));
#40398=CARTESIAN_POINT('Ctrl Pts',(80.5952691262063,409.433725846437,55.0831851225367));
#40399=CARTESIAN_POINT('Ctrl Pts',(78.3155544127733,408.998851684773,58.8116972627153));
#40400=CARTESIAN_POINT('Ctrl Pts',(71.90864214512,408.362383656117,58.9480975871434));
#40401=CARTESIAN_POINT('Ctrl Pts',(68.9450950083279,407.831993632236,54.524794049794));
#40402=CARTESIAN_POINT('Ctrl Pts',(69.6010890929968,407.407681613131,50.6984892817582));
#40403=CARTESIAN_POINT('Ctrl Pts',(71.9347077043872,406.983369594027,47.5960537873647));
#40404=CARTESIAN_POINT('Ctrl Pts',(77.1859865465286,406.452979570146,46.7172645440322));
#40405=CARTESIAN_POINT('Ctrl Pts',(80.386744270138,405.97883241758,50.2593803039047));
#40406=CARTESIAN_POINT('Ctrl Pts',(80.6361065402022,405.716841274567,52.5766157156117));
#40407=CARTESIAN_POINT('Ctrl Pts',(80.6319421555458,405.667006141107,53.0182025218874));
#40408=CARTESIAN_POINT('Ctrl Pts',(80.6387414332307,408.332993858894,53.0233301036444));
#40409=CARTESIAN_POINT('Ctrl Pts',(80.6399063121554,408.228331804484,53.9476020009326));
#40410=CARTESIAN_POINT('Ctrl Pts',(80.1469930043062,408.017591745297,55.8101772106293));
#40411=CARTESIAN_POINT('Ctrl Pts',(77.5645627245594,407.594695676559,58.6914128709184));
#40412=CARTESIAN_POINT('Ctrl Pts',(72.2572669003642,407.064305652677,59.1166316929431));
#40413=CARTESIAN_POINT('Ctrl Pts',(68.3843315795067,406.427837624022,54.0109585396062));
#40414=CARTESIAN_POINT('Ctrl Pts',(70.5882295550609,405.791369595364,48.0065658313019));
#40415=CARTESIAN_POINT('Ctrl Pts',(76.8287342059321,405.154901566707,46.6044208685245));
#40416=CARTESIAN_POINT('Ctrl Pts',(80.3093621919521,404.668776321217,50.0457497443635));
#40417=CARTESIAN_POINT('Ctrl Pts',(80.6329821588008,404.394807085279,52.4694276913957));
#40418=CARTESIAN_POINT('Ctrl Pts',(80.6278395430645,404.332993858894,53.0174600182511));
#40419=CARTESIAN_POINT('Origin',(74.9879498948689,423.667006141107,53.0228109606356));
#40420=CARTESIAN_POINT('',(80.6269259201534,413.667006141107,53.0266694084182));
#40421=CARTESIAN_POINT('',(80.6310716108719,412.332993858894,53.0264521482468));
#40422=CARTESIAN_POINT('',(80.6314498948689,423.667006141107,53.0228109606222));
#40423=CARTESIAN_POINT('Ctrl Pts',(80.6269259201534,413.667006141107,53.0266694084182));
#40424=CARTESIAN_POINT('Ctrl Pts',(80.6312435980057,413.596046722529,53.6570115578714));
#40425=CARTESIAN_POINT('Ctrl Pts',(80.2411937413767,413.312931294398,56.1667899653849));
#40426=CARTESIAN_POINT('Ctrl Pts',(76.5500783965337,412.817659856716,59.5150838971706));
#40427=CARTESIAN_POINT('Ctrl Pts',(71.4097383128725,412.287269832834,58.1195031021403));
#40428=CARTESIAN_POINT('Ctrl Pts',(69.397075484847,411.86295781373,54.8001736486049));
#40429=CARTESIAN_POINT('Ctrl Pts',(69.1240494715453,411.438645794625,50.9277902465141));
#40430=CARTESIAN_POINT('Ctrl Pts',(72.5128743250655,410.908255770745,46.8207854764477));
#40431=CARTESIAN_POINT('Ctrl Pts',(78.7687719438231,410.282349884646,47.5804943468211));
#40432=CARTESIAN_POINT('Ctrl Pts',(80.632488759591,409.868600008101,51.2451206940265));
#40433=CARTESIAN_POINT('Ctrl Pts',(80.6394151663029,409.667006141107,53.0244911165473));
#40434=CARTESIAN_POINT('Ctrl Pts',(80.6310716108719,412.332993858894,53.0264521482468));
#40435=CARTESIAN_POINT('Ctrl Pts',(80.6342885006541,412.27401253324,53.5496918395882));
#40436=CARTESIAN_POINT('Ctrl Pts',(80.3195049291274,412.002875198035,55.9505212394806));
#40437=CARTESIAN_POINT('Ctrl Pts',(76.922041457819,411.519581853277,59.4142434298776));
#40438=CARTESIAN_POINT('Ctrl Pts',(70.6502604163708,410.88311382462,58.0990212603595));
#40439=CARTESIAN_POINT('Ctrl Pts',(68.3768445575805,410.246645795963,52.120585584734));
#40440=CARTESIAN_POINT('Ctrl Pts',(72.1690405094426,409.610177767306,46.9698855255472));
#40441=CARTESIAN_POINT('Ctrl Pts',(78.5640475947216,408.973709738649,47.3834241974277));
#40442=CARTESIAN_POINT('Ctrl Pts',(80.6295583507564,408.547981769178,51.1247901462488));
#40443=CARTESIAN_POINT('Ctrl Pts',(80.6387256738349,408.33440980926,53.0108258284451));
#40444=CARTESIAN_POINT('Ctrl Pts',(80.6387414332307,408.332993858894,53.0233301036444));
#40445=CARTESIAN_POINT('Origin',(74.9879498948689,509.5,53.0228109606356));
#40446=CARTESIAN_POINT('',(69.9879498948689,509.,53.0228109606356));
#40447=CARTESIAN_POINT('Origin',(74.9879498948689,509.,53.0228109606356));
#40448=CARTESIAN_POINT('',(70.9879498948689,510.,53.0228109606356));
#40449=CARTESIAN_POINT('',(70.4879498948689,509.5,53.0228109606356));
#40450=CARTESIAN_POINT('Origin',(74.9879498948689,510.,53.0228109606356));
#40451=CARTESIAN_POINT('Origin',(74.9879498948689,416.,53.0228109606356));
#40452=CARTESIAN_POINT('',(69.9879498948689,455.,53.0228109606356));
#40453=CARTESIAN_POINT('',(69.9879498948689,416.,53.0228109606356));
#40454=CARTESIAN_POINT('Origin',(74.9879498948689,455.,53.0228109606356));
#40455=CARTESIAN_POINT('Origin',(74.9879498948689,510.,53.0228109606356));
#40456=CARTESIAN_POINT('Origin',(74.9879498948689,0.5,53.0228109606356));
#40457=CARTESIAN_POINT('',(78.9879498948689,0.,53.0228109606356));
#40458=CARTESIAN_POINT('Origin',(74.9879498948689,0.,53.0228109606356));
#40459=CARTESIAN_POINT('',(79.9879498948689,1.,53.0228109606356));
#40460=CARTESIAN_POINT('',(79.4879498948689,0.5,53.0228109606356));
#40461=CARTESIAN_POINT('Origin',(74.9879498948689,1.,53.0228109606356));
#40462=CARTESIAN_POINT('Origin',(74.9879498948689,0.,53.0228109606356));
#40463=CARTESIAN_POINT('',(79.9879498948689,15.,53.0228109606356));
#40464=CARTESIAN_POINT('',(79.9879498948689,0.,53.0228109606356));
#40465=CARTESIAN_POINT('Origin',(74.9879498948689,15.,53.0228109606356));
#40466=CARTESIAN_POINT('Origin',(74.9879498948689,0.,53.0228109606356));
#40467=CARTESIAN_POINT('Origin',(74.9879498948689,15.,53.0228109606356));
#40468=CARTESIAN_POINT('',(78.3434537325938,15.,60.2023805156308));
#40469=CARTESIAN_POINT('Ctrl Pts',(72.1688064861966,15.,57.9117293166054));
#40470=CARTESIAN_POINT('Ctrl Pts',(72.2546784237327,15.,58.0248630587345));
#40471=CARTESIAN_POINT('Ctrl Pts',(72.3449777763099,15.,58.13427856792));
#40472=CARTESIAN_POINT('Ctrl Pts',(72.4393010647226,15.,58.2398866170317));
#40473=CARTESIAN_POINT('Ctrl Pts',(72.5351751631816,15.,58.3472310138289));
#40474=CARTESIAN_POINT('Ctrl Pts',(72.635206430336,15.,58.4506423776243));
#40475=CARTESIAN_POINT('Ctrl Pts',(72.7390204213387,15.,58.5500517066503));
#40476=CARTESIAN_POINT('Ctrl Pts',(72.8444033767096,15.,58.65096343139));
#40477=CARTESIAN_POINT('Ctrl Pts',(72.9536841924254,15.,58.7477519171545));
#40478=CARTESIAN_POINT('Ctrl Pts',(73.0665233585081,15.,58.8403600304194));
#40479=CARTESIAN_POINT('Ctrl Pts',(73.180863358548,15.,58.9341998915422));
#40480=CARTESIAN_POINT('Ctrl Pts',(73.2988570389478,15.0000000000001,59.0237481324304));
#40481=CARTESIAN_POINT('Ctrl Pts',(73.4202044759237,15.0000000000001,59.1089501698777));
#40482=CARTESIAN_POINT('Ctrl Pts',(73.4609348987315,15.0000000000001,59.1375483429896));
#40483=CARTESIAN_POINT('Ctrl Pts',(73.5020435972152,14.9999999999999,59.1656568588392));
#40484=CARTESIAN_POINT('Ctrl Pts',(73.5435205270524,14.9999999999999,59.193273565218));
#40485=CARTESIAN_POINT('Ctrl Pts',(73.5707922927962,14.9999999999999,59.2114320053422));
#40486=CARTESIAN_POINT('Ctrl Pts',(73.5982267011967,15.,59.2293799234602));
#40487=CARTESIAN_POINT('Ctrl Pts',(73.6257970261555,15.,59.2471015554436));
#40488=CARTESIAN_POINT('Ctrl Pts',(73.7583003035948,15.,59.3322719088175));
#40489=CARTESIAN_POINT('Ctrl Pts',(73.8940373217576,15.,59.4122821412029));
#40490=CARTESIAN_POINT('Ctrl Pts',(74.032592582409,15.,59.4870928430669));
#40491=CARTESIAN_POINT('Ctrl Pts',(74.1743088382327,15.,59.5636102738297));
#40492=CARTESIAN_POINT('Ctrl Pts',(74.3189734092911,15.,59.6346888756922));
#40493=CARTESIAN_POINT('Ctrl Pts',(74.4661965872584,15.,59.7002916495573));
#40494=CARTESIAN_POINT('Ctrl Pts',(74.5848379276424,15.,59.7531583321798));
#40495=CARTESIAN_POINT('Ctrl Pts',(74.7051419796555,14.9999999999999,59.8024691803922));
#40496=CARTESIAN_POINT('Ctrl Pts',(74.8269292956354,14.9999999999999,59.8482028687199));
#40497=CARTESIAN_POINT('Ctrl Pts',(74.9660800226104,14.9999999999998,59.9004568816017));
#40498=CARTESIAN_POINT('Ctrl Pts',(75.1071665460714,14.9999999999999,59.9480416246017));
#40499=CARTESIAN_POINT('Ctrl Pts',(75.2499003342714,14.9999999999999,59.9909802687671));
#40500=CARTESIAN_POINT('Ctrl Pts',(75.3123463666089,14.9999999999999,60.0097659255895));
#40501=CARTESIAN_POINT('Ctrl Pts',(75.3751081297216,14.9999999999998,60.0276621259232));
#40502=CARTESIAN_POINT('Ctrl Pts',(75.4381633889478,14.9999999999998,60.0446699346699));
#40503=CARTESIAN_POINT('Ctrl Pts',(75.4670091976466,14.9999999999998,60.0524504751596));
#40504=CARTESIAN_POINT('Ctrl Pts',(75.4959164438666,14.9999999999999,60.0600450869122));
#40505=CARTESIAN_POINT('Ctrl Pts',(75.5248830744914,14.9999999999999,60.0674538280609));
#40506=CARTESIAN_POINT('Ctrl Pts',(75.5520898605735,14.9999999999999,60.0744124570496));
#40507=CARTESIAN_POINT('Ctrl Pts',(75.5793414200024,15.,60.0812051333796));
#40508=CARTESIAN_POINT('Ctrl Pts',(75.6066283015114,15.,60.0878303861922));
#40509=CARTESIAN_POINT('Ctrl Pts',(75.7740637033796,15.,60.1284836893846));
#40510=CARTESIAN_POINT('Ctrl Pts',(75.94290994267,14.9999999999998,60.1628557189233));
#40511=CARTESIAN_POINT('Ctrl Pts',(76.1126821629086,14.9999999999998,60.1910302695823));
#40512=CARTESIAN_POINT('Ctrl Pts',(76.2856185048526,14.9999999999998,60.2197299220934));
#40513=CARTESIAN_POINT('Ctrl Pts',(76.4595159481927,14.9999999999998,60.2419994636294));
#40514=CARTESIAN_POINT('Ctrl Pts',(76.6339143325404,14.9999999999998,60.257913982013));
#40515=CARTESIAN_POINT('Ctrl Pts',(76.8129175877103,14.9999999999999,60.2742487124395));
#40516=CARTESIAN_POINT('Ctrl Pts',(76.9924489312741,14.9999999999999,60.283888978601));
#40517=CARTESIAN_POINT('Ctrl Pts',(77.1720606699146,14.9999999999999,60.286893235395));
#40518=CARTESIAN_POINT('Ctrl Pts',(77.3538461982158,14.9999999999999,60.2899338518525));
#40519=CARTESIAN_POINT('Ctrl Pts',(77.5357146523819,14.9999999999999,60.2861774033693));
#40520=CARTESIAN_POINT('Ctrl Pts',(77.717245145824,14.9999999999999,60.2756529017544));
#40521=CARTESIAN_POINT('Ctrl Pts',(77.9003905459956,14.9999999999999,60.2650347735088));
#40522=CARTESIAN_POINT('Ctrl Pts',(78.0831926380365,15.,60.2475281592605));
#40523=CARTESIAN_POINT('Ctrl Pts',(78.2652533350261,15.,60.2231228362824));
#40524=CARTESIAN_POINT('Ctrl Pts',(78.2930224296742,15.,60.2194003759442));
#40525=CARTESIAN_POINT('Ctrl Pts',(78.3207743284586,14.9999999999999,60.2155173378091));
#40526=CARTESIAN_POINT('Ctrl Pts',(78.3485076714003,14.9999999999999,60.2114735929952));
#40527=CARTESIAN_POINT('Ctrl Pts',(78.3434537325882,14.9999999999999,45.8432414056378));
#40528=CARTESIAN_POINT('Ctrl Pts',(78.1604444691944,14.9999999999999,45.8163432874972));
#40529=CARTESIAN_POINT('Ctrl Pts',(77.9768364993718,14.9999999999998,45.7963747706827));
#40530=CARTESIAN_POINT('Ctrl Pts',(77.7929605518461,14.9999999999999,45.7833395953758));
#40531=CARTESIAN_POINT('Ctrl Pts',(77.6105716158271,14.9999999999999,45.7704098360079));
#40532=CARTESIAN_POINT('Ctrl Pts',(77.4279184304687,15.,45.7643022285713));
#40533=CARTESIAN_POINT('Ctrl Pts',(77.2453576416075,15.,45.7650583218053));
#40534=CARTESIAN_POINT('Ctrl Pts',(77.0651782861446,14.9999999999999,45.7658045521018));
#40535=CARTESIAN_POINT('Ctrl Pts',(76.8850884586316,15.,45.7732371101817));
#40536=CARTESIAN_POINT('Ctrl Pts',(76.7054719634877,15.,45.787425385552));
#40537=CARTESIAN_POINT('Ctrl Pts',(76.5221532410464,15.,45.8019061074504));
#40538=CARTESIAN_POINT('Ctrl Pts',(76.3393268374206,14.9999999999999,45.8234243776713));
#40539=CARTESIAN_POINT('Ctrl Pts',(76.1574531402198,14.9999999999998,45.8520775781582));
#40540=CARTESIAN_POINT('Ctrl Pts',(76.0789744509187,14.9999999999998,45.8644414639377));
#40541=CARTESIAN_POINT('Ctrl Pts',(76.0006738665816,15.,45.8781340766259));
#40542=CARTESIAN_POINT('Ctrl Pts',(75.922591806848,15.,45.8931641940993));
#40543=CARTESIAN_POINT('Ctrl Pts',(75.8968634177424,15.,45.8981166852602));
#40544=CARTESIAN_POINT('Ctrl Pts',(75.8711585155862,14.9999999999999,45.9032145034763));
#40545=CARTESIAN_POINT('Ctrl Pts',(75.845493153525,14.9999999999999,45.9084548388638));
#40546=CARTESIAN_POINT('Ctrl Pts',(75.6809018784442,14.9999999999999,45.9420609684487));
#40547=CARTESIAN_POINT('Ctrl Pts',(75.5177825848442,14.9999999999999,45.9815544092212));
#40548=CARTESIAN_POINT('Ctrl Pts',(75.3564446018102,14.9999999999998,46.0269586008827));
#40549=CARTESIAN_POINT('Ctrl Pts',(75.1977486437348,14.9999999999998,46.0716192664052));
#40550=CARTESIAN_POINT('Ctrl Pts',(75.0407758107613,14.9999999999999,46.1219992700254));
#40551=CARTESIAN_POINT('Ctrl Pts',(74.8858656690889,14.9999999999999,46.1781423428412));
#40552=CARTESIAN_POINT('Ctrl Pts',(74.7791862064282,14.9999999999999,46.2168054850696));
#40553=CARTESIAN_POINT('Ctrl Pts',(74.6734859004813,14.9999999999999,46.2582021789035));
#40554=CARTESIAN_POINT('Ctrl Pts',(74.5688895733295,14.9999999999999,46.3023505313413));
#40555=CARTESIAN_POINT('Ctrl Pts',(74.4230808149576,14.9999999999999,46.3638939586146));
#40556=CARTESIAN_POINT('Ctrl Pts',(74.2794151390612,14.9999999999999,46.4307849909926));
#40557=CARTESIAN_POINT('Ctrl Pts',(74.1383311642972,14.9999999999999,46.5029908494939));
#40558=CARTESIAN_POINT('Ctrl Pts',(74.0399765949272,14.9999999999999,46.5533280768848));
#40559=CARTESIAN_POINT('Ctrl Pts',(73.9428777407458,14.9999999999999,46.6062483716059));
#40560=CARTESIAN_POINT('Ctrl Pts',(73.8471982719262,14.9999999999999,46.6617392239536));
#40561=CARTESIAN_POINT('Ctrl Pts',(73.8193292090864,14.9999999999999,46.6779023367947));
#40562=CARTESIAN_POINT('Ctrl Pts',(73.7915764524053,14.9999999999998,46.6942861391598));
#40563=CARTESIAN_POINT('Ctrl Pts',(73.7639697491469,14.9999999999998,46.7108746871263));
#40564=CARTESIAN_POINT('Ctrl Pts',(73.635325383924,14.9999999999998,46.788175594922));
#40565=CARTESIAN_POINT('Ctrl Pts',(73.50975027916,14.9999999999999,46.8699766963246));
#40566=CARTESIAN_POINT('Ctrl Pts',(73.3875696928616,14.9999999999999,46.9562183983009));
#40567=CARTESIAN_POINT('Ctrl Pts',(73.2682057974333,14.9999999999999,47.0404719266896));
#40568=CARTESIAN_POINT('Ctrl Pts',(73.1520816382575,14.9999999999998,47.128964325939));
#40569=CARTESIAN_POINT('Ctrl Pts',(73.0395496569516,14.9999999999998,47.2216433484764));
#40570=CARTESIAN_POINT('Ctrl Pts',(72.9285853368353,14.9999999999998,47.3130312775395));
#40571=CARTESIAN_POINT('Ctrl Pts',(72.8211137584,14.9999999999998,47.4084906138113));
#40572=CARTESIAN_POINT('Ctrl Pts',(72.7175222237852,14.9999999999998,47.5079652205717));
#40573=CARTESIAN_POINT('Ctrl Pts',(72.6162286608911,14.9999999999998,47.6052331814503));
#40574=CARTESIAN_POINT('Ctrl Pts',(72.5186450261201,14.9999999999999,47.7063408125022));
#40575=CARTESIAN_POINT('Ctrl Pts',(72.4251803497841,14.9999999999999,47.8112211767485));
#40576=CARTESIAN_POINT('Ctrl Pts',(72.3343088870862,14.9999999999999,47.9131915946753));
#40577=CARTESIAN_POINT('Ctrl Pts',(72.2473312334373,14.9999999999999,48.0187287888016));
#40578=CARTESIAN_POINT('Ctrl Pts',(72.1646654645466,14.9999999999999,48.1277497923169));
#40579=CARTESIAN_POINT('Origin',(74.9879498948689,15.,53.0228109606356));
#40580=CARTESIAN_POINT('Ctrl Pts',(68.1225865616467,416.611326082532,56.981650601597));
#40581=CARTESIAN_POINT('Ctrl Pts',(67.4629372253086,416.505248077756,55.8376961156356));
#40582=CARTESIAN_POINT('Ctrl Pts',(66.7429036265161,416.293092068203,53.2244189993033));
#40583=CARTESIAN_POINT('Ctrl Pts',(67.9167913369144,415.868780049099,47.8794315286107));
#40584=CARTESIAN_POINT('Ctrl Pts',(74.0953234943061,415.338390025218,43.6918638654563));
#40585=CARTESIAN_POINT('Ctrl Pts',(82.3660788114064,414.701921996561,47.2361689914527));
#40586=CARTESIAN_POINT('Ctrl Pts',(83.8426349834315,414.065453967903,56.0973433337628));
#40587=CARTESIAN_POINT('Ctrl Pts',(77.1816007100824,413.428985939248,62.1397176713732));
#40588=CARTESIAN_POINT('Ctrl Pts',(69.9631732868513,412.898595915366,60.1799448706925));
#40589=CARTESIAN_POINT('Ctrl Pts',(67.1368504531333,412.474283896262,55.518708772654));
#40590=CARTESIAN_POINT('Ctrl Pts',(66.7534481043442,412.049971877156,50.0808353852934));
#40591=CARTESIAN_POINT('Ctrl Pts',(71.5122745354891,411.519581853277,44.3134901557799));
#40592=CARTESIAN_POINT('Ctrl Pts',(80.445492513773,410.883113824618,45.3983296708595));
#40593=CARTESIAN_POINT('Ctrl Pts',(84.3461800842815,410.246645795963,53.4889644224392));
#40594=CARTESIAN_POINT('Ctrl Pts',(79.6608064208477,409.610177767304,61.1519726411528));
#40595=CARTESIAN_POINT('Ctrl Pts',(70.6637691707098,408.973709738649,61.3435155792337));
#40596=CARTESIAN_POINT('Ctrl Pts',(66.5021476487722,408.443319714767,55.1320013533967));
#40597=CARTESIAN_POINT('Ctrl Pts',(67.4233407241729,408.019007695663,49.7588348278931));
#40598=CARTESIAN_POINT('Ctrl Pts',(70.7003722640477,407.594695676558,45.4021764965285));
#40599=CARTESIAN_POINT('Ctrl Pts',(78.0745877019812,407.064305652678,44.168118774657));
#40600=CARTESIAN_POINT('Ctrl Pts',(84.1080553689783,406.427837624021,50.8450505375157));
#40601=CARTESIAN_POINT('Ctrl Pts',(81.7476715690704,405.791369595364,59.5111857266153));
#40602=CARTESIAN_POINT('Ctrl Pts',(73.1854533668698,405.154901566707,62.2244404843412));
#40603=CARTESIAN_POINT('Ctrl Pts',(66.2670718320099,404.518433538049,56.4694287670495));
#40604=CARTESIAN_POINT('Ctrl Pts',(67.19814392288,403.988043514169,49.0508711380302));
#40605=CARTESIAN_POINT('Ctrl Pts',(71.4169665351032,403.563731495064,45.598191667147));
#40606=CARTESIAN_POINT('Ctrl Pts',(76.7479040366348,403.13941947596,44.4577690126192));
#40607=CARTESIAN_POINT('Ctrl Pts',(83.1246198509995,402.609029452079,48.3615350602155));
#40608=CARTESIAN_POINT('Ctrl Pts',(83.3016244349796,401.972561423422,57.358914436859));
#40609=CARTESIAN_POINT('Ctrl Pts',(75.8369141305076,401.336093394765,62.3540542041882));
#40610=CARTESIAN_POINT('Ctrl Pts',(67.5933056949457,400.699625366108,58.7880702754657));
#40611=CARTESIAN_POINT('Ctrl Pts',(66.1436664996217,400.063157337451,49.9064762517133));
#40612=CARTESIAN_POINT('Ctrl Pts',(71.7111780792753,399.53276731357,44.9160145050502));
#40613=CARTESIAN_POINT('Ctrl Pts',(77.1603959625132,399.108455294466,45.0756497094295));
#40614=CARTESIAN_POINT('Ctrl Pts',(81.9330467436625,398.684143275361,47.7102774725632));
#40615=CARTESIAN_POINT('Ctrl Pts',(84.1876426409602,398.15375325148,54.83900042918));
#40616=CARTESIAN_POINT('Ctrl Pts',(78.4214489426319,397.517285222823,61.7480652304801));
#40617=CARTESIAN_POINT('Ctrl Pts',(69.5101601487526,396.880817194167,60.6245647221929));
#40618=CARTESIAN_POINT('Ctrl Pts',(65.6245720453742,396.244349165508,52.5266929985891));
#40619=CARTESIAN_POINT('Ctrl Pts',(70.3540062684141,395.607881136854,44.8705439585235));
#40620=CARTESIAN_POINT('Ctrl Pts',(77.829847457575,395.077491112971,44.7535304268656));
#40621=CARTESIAN_POINT('Ctrl Pts',(81.8393155107531,394.653179093867,48.4472581999877));
#40622=CARTESIAN_POINT('Ctrl Pts',(83.7150557611386,394.228867074762,53.5659550502071));
#40623=CARTESIAN_POINT('Ctrl Pts',(80.7427680213086,393.698477050882,60.4265234846684));
#40624=CARTESIAN_POINT('Ctrl Pts',(71.8588410072801,393.062009022225,61.8617959337022));
#40625=CARTESIAN_POINT('Ctrl Pts',(65.8675517102712,392.425540993567,55.1701762552898));
#40626=CARTESIAN_POINT('Ctrl Pts',(68.2439423679512,391.789072964911,46.508416110662));
#40627=CARTESIAN_POINT('Ctrl Pts',(76.8350025796891,391.152604936254,43.8292650078264));
#40628=CARTESIAN_POINT('Ctrl Pts',(82.5559722100773,390.622214912373,48.6430369322593));
#40629=CARTESIAN_POINT('Ctrl Pts',(83.1610301794806,390.197902893269,54.0609114033989));
#40630=CARTESIAN_POINT('Ctrl Pts',(81.2207373946848,389.773590874163,59.1554891916591));
#40631=CARTESIAN_POINT('Ctrl Pts',(74.4780025100577,389.243200850283,62.3861887951374));
#40632=CARTESIAN_POINT('Ctrl Pts',(66.8295127442103,388.606732821626,57.6443779073797));
#40633=CARTESIAN_POINT('Ctrl Pts',(66.6939859425028,387.97026479297,48.6635675961109));
#40634=CARTESIAN_POINT('Ctrl Pts',(74.1679115467585,387.333796764312,43.682226669912));
#40635=CARTESIAN_POINT('Ctrl Pts',(82.4109334435622,386.697328735656,47.29287151569));
#40636=CARTESIAN_POINT('Ctrl Pts',(83.5737265630747,386.166938711774,54.6786555508142));
#40637=CARTESIAN_POINT('Ctrl Pts',(80.4778928884972,385.742626692671,59.1658899764619));
#40638=CARTESIAN_POINT('Ctrl Pts',(75.6723206511343,385.318314673565,61.7399790197646));
#40639=CARTESIAN_POINT('Ctrl Pts',(68.4631138765931,384.787924649685,59.7577501393902));
#40640=CARTESIAN_POINT('Ctrl Pts',(65.7978612288556,384.151456621028,51.1623679770162));
#40641=CARTESIAN_POINT('Ctrl Pts',(71.5845057620196,383.51498859237,44.2930109177437));
#40642=CARTESIAN_POINT('Ctrl Pts',(80.4937037924029,382.878520563714,45.4329722400649));
#40643=CARTESIAN_POINT('Ctrl Pts',(84.3495636598611,382.242052535057,53.5641782315556));
#40644=CARTESIAN_POINT('Ctrl Pts',(80.3844055763066,381.711662511175,59.9029016854306));
#40645=CARTESIAN_POINT('Ctrl Pts',(75.1046549021694,381.287350492072,61.2607277973877));
#40646=CARTESIAN_POINT('Ctrl Pts',(69.788558668218,380.863038472966,60.0530110413841));
#40647=CARTESIAN_POINT('Ctrl Pts',(65.6454289172183,380.332648449086,53.8291561652914));
#40648=CARTESIAN_POINT('Ctrl Pts',(69.2694010835046,379.696180420429,45.5919848102989));
#40649=CARTESIAN_POINT('Ctrl Pts',(78.1427309546104,379.059712391772,44.2001017837785));
#40650=CARTESIAN_POINT('Ctrl Pts',(84.1216479173398,378.423244363115,50.9027783621136));
#40651=CARTESIAN_POINT('Ctrl Pts',(81.7009543132028,377.786776334458,59.5702121615964));
#40652=CARTESIAN_POINT('Ctrl Pts',(74.5507931646769,377.256386310578,61.755867487212));
#40653=CARTESIAN_POINT('Ctrl Pts',(69.6742308536814,376.832074291472,59.3189434099489));
#40654=CARTESIAN_POINT('Ctrl Pts',(66.4525254996838,376.407762272368,54.9212083629745));
#40655=CARTESIAN_POINT('Ctrl Pts',(67.4056279554398,375.877372248488,47.505448836054));
#40656=CARTESIAN_POINT('Ctrl Pts',(75.543059676302,375.24090421983,43.6627452068579));
#40657=CARTESIAN_POINT('Ctrl Pts',(83.1550969766561,374.604436191174,48.4303661543525));
#40658=CARTESIAN_POINT('Ctrl Pts',(83.2740323816697,373.967968162516,57.4114115127954));
#40659=CARTESIAN_POINT('Ctrl Pts',(75.7629377951823,373.33150013386,62.3679853603609));
#40660=CARTESIAN_POINT('Ctrl Pts',(68.9313898304873,372.801110109979,59.3295900506045));
#40661=CARTESIAN_POINT('Ctrl Pts',(66.8475568448849,372.376798090874,54.2920212898348));
#40662=CARTESIAN_POINT('Ctrl Pts',(67.2988947945623,371.952486071769,48.859181057825));
#40663=CARTESIAN_POINT('Ctrl Pts',(72.8812042835999,371.422096047889,43.8852777193108));
#40664=CARTESIAN_POINT('Ctrl Pts',(81.5447115814599,370.785628019232,46.3199866328066));
#40665=CARTESIAN_POINT('Ctrl Pts',(84.1655183393139,370.149159990575,54.9109524282782));
#40666=CARTESIAN_POINT('Ctrl Pts',(78.3661932179409,369.512691961918,61.769607507635));
#40667=CARTESIAN_POINT('Ctrl Pts',(69.4451731646705,368.876223933261,60.5865743708756));
#40668=CARTESIAN_POINT('Ctrl Pts',(66.2797325110554,368.34583390938,53.8129579718812));
#40669=CARTESIAN_POINT('Ctrl Pts',(68.0097178803784,367.921521890275,48.6431794898481));
#40670=CARTESIAN_POINT('Ctrl Pts',(71.9129411847918,367.497209871171,44.8373541171795));
#40671=CARTESIAN_POINT('Ctrl Pts',(79.3890969473516,366.96681984729,44.7425455404127));
#40672=CARTESIAN_POINT('Ctrl Pts',(84.3335160685705,366.330351818633,52.2616469326837));
#40673=CARTESIAN_POINT('Ctrl Pts',(80.6788833058256,365.693883789976,60.4663395369466));
#40674=CARTESIAN_POINT('Ctrl Pts',(71.8029972093442,365.05741576132,61.8418275824281));
#40675=CARTESIAN_POINT('Ctrl Pts',(65.8433980359348,364.420947732661,55.0988798675317));
#40676=CARTESIAN_POINT('Ctrl Pts',(67.89514712053,363.890557708782,47.9091497372594));
#40677=CARTESIAN_POINT('Ctrl Pts',(72.591248992436,363.466245689677,45.1403799490598));
#40678=CARTESIAN_POINT('Ctrl Pts',(78.0337578782412,363.041933670573,44.8264437146201));
#40679=CARTESIAN_POINT('Ctrl Pts',(83.7404046046765,362.511543646691,49.6571865966155));
#40680=CARTESIAN_POINT('Ctrl Pts',(82.5429443961398,361.875075618035,58.5762815755079));
#40681=CARTESIAN_POINT('Ctrl Pts',(74.4036612243952,361.238607589377,62.3743588273717));
#40682=CARTESIAN_POINT('Ctrl Pts',(66.8004446252625,360.602139560721,57.5926835239192));
#40683=CARTESIAN_POINT('Ctrl Pts',(66.7225010042729,359.965671532063,48.5939007737091));
#40684=CARTESIAN_POINT('Ctrl Pts',(72.9860720763478,359.435281508183,44.5110621683577));
#40685=CARTESIAN_POINT('Ctrl Pts',(78.3471760447884,359.010969489078,45.500012708544));
#40686=CARTESIAN_POINT('Ctrl Pts',(82.6621127768296,358.586657469973,48.8317960042954));
#40687=CARTESIAN_POINT('Ctrl Pts',(83.8029638126729,358.056267446093,56.2210011419468));
#40688=CARTESIAN_POINT('Ctrl Pts',(77.050386020973,357.419799417436,62.1696866572998));
#40689=CARTESIAN_POINT('Ctrl Pts',(68.4147436383932,356.783331388779,59.7000708974758));
#40690=CARTESIAN_POINT('Ctrl Pts',(65.8098123187626,356.146863360122,51.1042780788362));
#40691=CARTESIAN_POINT('Ctrl Pts',(71.6517170309307,355.510395331465,44.2591107669676));
#40692=CARTESIAN_POINT('Ctrl Pts',(79.0579276024554,354.980005307585,45.2837758939829));
#40693=CARTESIAN_POINT('Ctrl Pts',(82.4570647662865,354.555693288479,49.5458558407725));
#40694=CARTESIAN_POINT('Ctrl Pts',(83.530087844715,354.131381269375,54.8907674775094));
#40695=CARTESIAN_POINT('Ctrl Pts',(79.5461202331947,353.600991245494,61.2176858207979));
#40696=CARTESIAN_POINT('Ctrl Pts',(70.5472231890065,352.964523216837,61.2810749494122));
#40697=CARTESIAN_POINT('Ctrl Pts',(65.6467313954362,352.328055188181,53.7538907785469));
#40698=CARTESIAN_POINT('Ctrl Pts',(69.3165152858901,351.691587159523,45.5559637504295));
#40699=CARTESIAN_POINT('Ctrl Pts',(78.2157045584089,351.055119130867,44.2185795552879));
#40700=CARTESIAN_POINT('Ctrl Pts',(83.1354728280878,350.524729106985,49.8486571590997));
#40701=CARTESIAN_POINT('Ctrl Pts',(82.9070482515139,350.100417087882,55.2954251130503));
#40702=CARTESIAN_POINT('Ctrl Pts',(80.2123707723944,349.676105068776,60.0344305166016));
#40703=CARTESIAN_POINT('Ctrl Pts',(73.0557494183956,349.145715044896,62.1988390842647));
#40704=CARTESIAN_POINT('Ctrl Pts',(66.2200396000194,348.509247016238,56.3458708225633));
#40705=CARTESIAN_POINT('Ctrl Pts',(67.4559649289566,347.872778987582,47.4494777364714));
#40706=CARTESIAN_POINT('Ctrl Pts',(75.6022507863105,347.236310958925,43.6664434924748));
#40707=CARTESIAN_POINT('Ctrl Pts',(83.1980754689443,346.599842930268,48.4921676437515));
#40708=CARTESIAN_POINT('Ctrl Pts',(83.2206893294649,346.069452906387,55.9688903392643));
#40709=CARTESIAN_POINT('Ctrl Pts',(79.4766322461752,345.645140887283,59.9314015996187));
#40710=CARTESIAN_POINT('Ctrl Pts',(74.3346602262409,345.220828868178,61.7423634097004));
#40711=CARTESIAN_POINT('Ctrl Pts',(67.5121669129356,344.690438844297,58.6836907168177));
#40712=CARTESIAN_POINT('Ctrl Pts',(66.1891777776275,344.05397081564,49.7823500345728));
#40713=CARTESIAN_POINT('Ctrl Pts',(72.9559103728996,343.417502786983,43.8760270375587));
#40714=CARTESIAN_POINT('Ctrl Pts',(81.5869756465227,342.781034758326,46.361592084672));
#40715=CARTESIAN_POINT('Ctrl Pts',(84.15744203475,342.144566729669,54.9857945834842));
#40716=CARTESIAN_POINT('Ctrl Pts',(79.2718205765323,341.614176705788,60.645529260948));
#40717=CARTESIAN_POINT('Ctrl Pts',(73.8467384815149,341.189864686684,61.182132646781));
#40718=CARTESIAN_POINT('Ctrl Pts',(68.777065024432,340.765552667579,59.1776701328107));
#40719=CARTESIAN_POINT('Ctrl Pts',(65.6317570526712,340.235162643698,52.3946817489889));
#40720=CARTESIAN_POINT('Ctrl Pts',(70.4697601757384,339.598694615042,44.8066719984206));
#40721=CARTESIAN_POINT('Ctrl Pts',(79.4515657791064,338.962226586384,44.7845481587893));
#40722=CARTESIAN_POINT('Ctrl Pts',(84.3381434764118,338.325758557728,52.3207726624231));
#40723=CARTESIAN_POINT('Ctrl Pts',(80.6237096357617,337.689290529071,60.5175493116288));
#40724=CARTESIAN_POINT('Ctrl Pts',(73.2238328504367,337.15890050519,61.5869964652049));
#40725=CARTESIAN_POINT('Ctrl Pts',(68.7760442604858,336.734588486085,58.434753519227));
#40726=CARTESIAN_POINT('Ctrl Pts',(66.2628357971074,336.31027646698,53.5970637657427));
#40727=CARTESIAN_POINT('Ctrl Pts',(68.3359304749261,335.7798864431,46.4134593703794));
#40728=CARTESIAN_POINT('Ctrl Pts',(76.9642790972773,335.143418414443,43.8569448985446));
#40729=CARTESIAN_POINT('Ctrl Pts',(83.7600261255697,334.506950385786,49.7298610130848));
#40730=CARTESIAN_POINT('Ctrl Pts',(82.5076676927869,333.870482357129,58.6239556672253));
#40731=CARTESIAN_POINT('Ctrl Pts',(74.3284255748771,333.234014328472,62.3768431648914));
#40732=CARTESIAN_POINT('Ctrl Pts',(68.0402716754738,332.703624304591,58.3319681124699));
#40733=CARTESIAN_POINT('Ctrl Pts',(66.7492161935976,332.279312285487,53.0354943162464));
#40734=CARTESIAN_POINT('Ctrl Pts',(68.0239579766349,331.855000266382,47.7350705296098));
#40735=CARTESIAN_POINT('Ctrl Pts',(74.2996281013125,331.324610242501,43.6708537368546));
#40736=CARTESIAN_POINT('Ctrl Pts',(82.49038640365,330.688142213844,47.3985399664363));
#40737=CARTESIAN_POINT('Ctrl Pts',(83.7701233751467,330.051674185187,56.2887365134628));
#40738=CARTESIAN_POINT('Ctrl Pts',(76.9924909750265,329.41520615653,62.1825485574472));
#40739=CARTESIAN_POINT('Ctrl Pts',(68.3563118700172,328.778738127874,59.6526124594933));
#40740=CARTESIAN_POINT('Ctrl Pts',(66.261109058149,328.248348103992,52.4754250696154));
#40741=CARTESIAN_POINT('Ctrl Pts',(68.7594106029481,327.824036084888,47.6300202028764));
#40742=CARTESIAN_POINT('Ctrl Pts',(73.1974725113032,327.399724065783,44.4640976787181));
#40743=CARTESIAN_POINT('Ctrl Pts',(80.6006069959407,326.869334041903,45.5107559107372));
#40744=CARTESIAN_POINT('Ctrl Pts',(84.3402606976814,326.232866013246,53.6960571504341));
#40745=CARTESIAN_POINT('Ctrl Pts',(79.4769098228901,325.596397984588,61.2472914620972));
#40746=CARTESIAN_POINT('Ctrl Pts',(70.4950786748861,324.959929955932,61.2528222598463));
#40747=CARTESIAN_POINT('Ctrl Pts',(65.6337353794111,324.323461927275,53.6797444471556));
#40748=CARTESIAN_POINT('Ctrl Pts',(68.7581439587704,323.793071903394,46.8871039678202));
#40749=CARTESIAN_POINT('Ctrl Pts',(73.8216217453728,323.368759884289,44.867041682654));
#40750=CARTESIAN_POINT('Ctrl Pts',(79.2483303007407,322.944447865185,45.3869389671831));
#40751=CARTESIAN_POINT('Ctrl Pts',(84.1513546426586,322.414057841304,51.0316042322666));
#40752=CARTESIAN_POINT('Ctrl Pts',(81.6074539287359,321.777589812647,59.6636801906463));
#40753=CARTESIAN_POINT('Ctrl Pts',(72.984082497274,321.14112178399,62.1758080767258));
#40754=CARTESIAN_POINT('Ctrl Pts',(66.1991967015628,320.504653755333,56.290347508501));
#40755=CARTESIAN_POINT('Ctrl Pts',(67.4947727809053,319.868185726676,47.3849756007047));
#40756=CARTESIAN_POINT('Ctrl Pts',(74.3078162547182,319.337795702796,44.3053112884437));
#40757=CARTESIAN_POINT('Ctrl Pts',(79.4553397631149,318.913483683691,46.1004326386231));
#40758=CARTESIAN_POINT('Ctrl Pts',(83.2115794746481,318.489171664586,50.0513973513058));
#40759=CARTESIAN_POINT('Ctrl Pts',(83.2119861784514,317.958781640706,57.5281542342649));
#40760=CARTESIAN_POINT('Ctrl Pts',(75.6310556643944,317.322313612048,62.3772426779387));
#40761=CARTESIAN_POINT('Ctrl Pts',(67.473160646069,316.685845583392,58.6193083742348));
#40762=CARTESIAN_POINT('Ctrl Pts',(66.2098496237681,316.049377554734,49.7267628094426));
#40763=CARTESIAN_POINT('Ctrl Pts',(73.0275060429953,315.412909526078,43.8527754803025));
#40764=CARTESIAN_POINT('Ctrl Pts',(80.1907575810404,314.882519502196,45.9951389076834));
#40765=CARTESIAN_POINT('Ctrl Pts',(82.9000134492689,314.458207483093,50.7258250705812));
#40766=CARTESIAN_POINT('Ctrl Pts',(83.1452072706115,314.033895463987,56.1718638990638));
#40767=CARTESIAN_POINT('Ctrl Pts',(78.2427970493154,313.503505440107,61.8170625381211));
#40768=CARTESIAN_POINT('Ctrl Pts',(69.3395322193748,312.86703741145,60.5070848430938));
#40769=CARTESIAN_POINT('Ctrl Pts',(65.6445247142307,312.230569382793,52.3204957549632));
#40770=CARTESIAN_POINT('Ctrl Pts',(70.5218174540695,311.594101354136,44.7782588924076));
#40771=CARTESIAN_POINT('Ctrl Pts',(79.5208670156516,310.957633325478,44.8139405643491));
#40772=CARTESIAN_POINT('Ctrl Pts',(83.5242960099995,310.427243301599,51.1285624801488));
#40773=CARTESIAN_POINT('Ctrl Pts',(82.4677347346415,310.002931282493,56.4767525667836));
#40774=CARTESIAN_POINT('Ctrl Pts',(79.0817364147207,309.578619263389,60.7492780855906));
#40775=CARTESIAN_POINT('Ctrl Pts',(71.6787158414133,309.048229239508,61.7967417095284));
#40776=CARTESIAN_POINT('Ctrl Pts',(65.8157628902134,308.411761210851,54.9695937775186));
#40777=CARTESIAN_POINT('Ctrl Pts',(68.3942158441679,307.775293182194,46.3658212488418));
#40778=CARTESIAN_POINT('Ctrl Pts',(77.022213469953,307.138825153537,43.8696284817613));
#40779=CARTESIAN_POINT('Ctrl Pts',(83.7930749612714,306.50235712488,49.7974949494634));
#40780=CARTESIAN_POINT('Ctrl Pts',(82.674980327966,305.971967100999,57.1901776860114));
#40781=CARTESIAN_POINT('Ctrl Pts',(78.3703224436088,305.547655081895,60.5352306646661));
#40782=CARTESIAN_POINT('Ctrl Pts',(73.0122888161883,305.12334306279,61.5406830895957));
#40783=CARTESIAN_POINT('Ctrl Pts',(66.736176576404,304.59295303891,57.4771490604643));
#40784=CARTESIAN_POINT('Ctrl Pts',(66.7864130236384,303.956485010252,48.4781689797607));
#40785=CARTESIAN_POINT('Ctrl Pts',(74.3748710433667,303.320016981596,43.6731064157774));
#40786=CARTESIAN_POINT('Ctrl Pts',(82.5258097259484,302.683548952939,47.4461052169655));
#40787=CARTESIAN_POINT('Ctrl Pts',(83.7507257081707,302.047080924282,56.3614709991433));
#40788=CARTESIAN_POINT('Ctrl Pts',(78.0589796480722,301.516690900401,61.2097614648264));
#40789=CARTESIAN_POINT('Ctrl Pts',(72.6155299655976,301.092378881296,60.9125839324752));
#40790=CARTESIAN_POINT('Ctrl Pts',(67.9109254487115,300.668066862192,58.1582863321683));
#40791=CARTESIAN_POINT('Ctrl Pts',(65.8370492680559,300.137676838311,50.9749075143978));
#40792=CARTESIAN_POINT('Ctrl Pts',(71.7758589926117,299.501208809654,44.2136424516264));
#40793=CARTESIAN_POINT('Ctrl Pts',(80.6559380768304,298.864740780997,45.5617955657014));
#40794=CARTESIAN_POINT('Ctrl Pts',(84.3358153569538,298.22827275234,53.7551968474773));
#40795=CARTESIAN_POINT('Ctrl Pts',(79.4145706112079,297.591804723683,61.2894862198068));
#40796=CARTESIAN_POINT('Ctrl Pts',(71.9381583745758,297.061414699802,61.2176968040063));
#40797=CARTESIAN_POINT('Ctrl Pts',(68.0232356244143,296.637102680698,57.4239073011965));
#40798=CARTESIAN_POINT('Ctrl Pts',(66.2773409644892,296.212790661593,52.2594798626694));
#40799=CARTESIAN_POINT('Ctrl Pts',(69.4219109861495,295.682400637713,45.4761493362127));
#40800=CARTESIAN_POINT('Ctrl Pts',(78.3392462538169,295.045932609055,44.2656544301752));
#40801=CARTESIAN_POINT('Ctrl Pts',(84.1596613442124,294.409464580399,51.1064211661828));
#40802=CARTESIAN_POINT('Ctrl Pts',(81.5653181651201,293.772996551741,59.7054155742559));
#40803=CARTESIAN_POINT('Ctrl Pts',(72.9093482796908,293.136528523085,62.1667874551533));
#40804=CARTESIAN_POINT('Ctrl Pts',(67.3117508498048,292.606138499203,57.2100953459727));
#40805=CARTESIAN_POINT('Ctrl Pts',(66.8436875947261,292.1818264801,51.7786705125969));
#40806=CARTESIAN_POINT('Ctrl Pts',(68.9120002794622,291.757514460994,46.7347096117251));
#40807=CARTESIAN_POINT('Ctrl Pts',(75.7341607948001,291.227124437114,43.6752947076548));
#40808=CARTESIAN_POINT('Ctrl Pts',(83.2604808230956,290.590656408457,48.6087187746907));
#40809=CARTESIAN_POINT('Ctrl Pts',(83.1691981735905,289.9541883798,57.5900877593652));
#40810=CARTESIAN_POINT('Ctrl Pts',(75.571876221788,289.317720351143,62.3811231925081));
#40811=CARTESIAN_POINT('Ctrl Pts',(67.422651578918,288.681252322486,58.5634925249907));
#40812=CARTESIAN_POINT('Ctrl Pts',(66.4467208862754,288.150862298605,51.1507027036456));
#40813=CARTESIAN_POINT('Ctrl Pts',(69.6548705620827,287.7265502795,46.7430690313694));
#40814=CARTESIAN_POINT('Ctrl Pts',(74.5239065903062,287.302238260396,44.2911418123788));
#40815=CARTESIAN_POINT('Ctrl Pts',(81.6807633712101,286.771848236515,46.4547717876539));
#40816=CARTESIAN_POINT('Ctrl Pts',(84.1281320986843,286.135380207858,55.1147113085348));
#40817=CARTESIAN_POINT('Ctrl Pts',(78.1698806835492,285.498912179201,61.835764904141));
#40818=CARTESIAN_POINT('Ctrl Pts',(69.2923073332586,284.862444150544,60.4712090162484));
#40819=CARTESIAN_POINT('Ctrl Pts',(65.6429905038059,284.225976121887,52.2452347352405));
#40820=CARTESIAN_POINT('Ctrl Pts',(69.7669376769983,283.695586098006,46.0086528697471));
#40821=CARTESIAN_POINT('Ctrl Pts',(75.0792902129726,283.271274078902,44.7845738425221));
#40822=CARTESIAN_POINT('Ctrl Pts',(80.3631965402376,282.846962059797,46.1261374288099));
#40823=CARTESIAN_POINT('Ctrl Pts',(84.3478524431245,282.316572035916,52.4526223128409));
#40824=CARTESIAN_POINT('Ctrl Pts',(80.5170464309942,281.68010400726,60.5956617632522));
#40825=CARTESIAN_POINT('Ctrl Pts',(71.6114005142047,281.043635978602,61.7630486595907));
#40826=CARTESIAN_POINT('Ctrl Pts',(65.8036330010486,280.407167949946,54.9115409514946));
#40827=CARTESIAN_POINT('Ctrl Pts',(68.442408261578,279.770699921289,46.3079933507691));
#40828=CARTESIAN_POINT('Ctrl Pts',(75.6454776805482,279.240309897407,44.303577077192));
#40829=CARTESIAN_POINT('Ctrl Pts',(80.4589526316782,278.815997878304,46.8628578015768));
#40830=CARTESIAN_POINT('Ctrl Pts',(83.5685876035802,278.391685859198,51.3405390399957));
#40831=CARTESIAN_POINT('Ctrl Pts',(82.4285404572061,277.861295835319,58.7298682488162));
#40832=CARTESIAN_POINT('Ctrl Pts',(74.1966746279617,277.22482780666,62.3658758344585));
#40833=CARTESIAN_POINT('Ctrl Pts',(66.7074471491151,276.588359778005,57.407570364738));
#40834=CARTESIAN_POINT('Ctrl Pts',(66.8153218403697,275.951891749346,48.4263853420385));
#40835=CARTESIAN_POINT('Ctrl Pts',(74.4491755527711,275.315423720691,43.6610476109663));
#40836=CARTESIAN_POINT('Ctrl Pts',(81.2018256402978,274.785033696809,46.8709713558098));
#40837=CARTESIAN_POINT('Ctrl Pts',(83.1577951796486,274.360721677705,51.9595509309462));
#40838=CARTESIAN_POINT('Ctrl Pts',(82.5694214441079,273.9364096586,57.3792626648571));
#40839=CARTESIAN_POINT('Ctrl Pts',(76.8633002952122,273.406019634719,62.210626352928));
#40840=CARTESIAN_POINT('Ctrl Pts',(68.2640318319858,272.769551606063,59.5579393961078));
#40841=CARTESIAN_POINT('Ctrl Pts',(65.8609833098742,272.133083577405,50.9035370966215));
#40842=CARTESIAN_POINT('Ctrl Pts',(71.8316410442895,271.496615548749,44.1935022547268));
#40843=CARTESIAN_POINT('Ctrl Pts',(80.7199450811446,270.860147520091,45.6014147313923));
#40844=CARTESIAN_POINT('Ctrl Pts',(83.7133420812205,270.329757496211,52.4527991208584));
#40845=CARTESIAN_POINT('Ctrl Pts',(81.8533709346943,269.905445477106,57.5772470194573));
#40846=CARTESIAN_POINT('Ctrl Pts',(77.8552946903246,269.481133458002,61.2833022370128));
#40847=CARTESIAN_POINT('Ctrl Pts',(70.3791286576398,268.950743434121,61.189307003014));
#40848=CARTESIAN_POINT('Ctrl Pts',(65.6261439501125,268.314275405464,53.5477559455689));
#40849=CARTESIAN_POINT('Ctrl Pts',(69.4867806917746,267.677807376807,45.4379590732729));
#40850=CARTESIAN_POINT('Ctrl Pts',(78.394568044232,267.04133934815,44.2870264756042));
#40851=CARTESIAN_POINT('Ctrl Pts',(84.1820070775441,266.404871319493,51.1783047045848));
#40852=CARTESIAN_POINT('Ctrl Pts',(81.9493708504318,265.874481295612,58.3139356598449));
#40853=CARTESIAN_POINT('Ctrl Pts',(77.1848545790382,265.450169276508,60.9632456890776));
#40854=CARTESIAN_POINT('Ctrl Pts',(71.7361540343936,265.025857257403,61.1396580076683));
#40855=CARTESIAN_POINT('Ctrl Pts',(66.1533034599807,264.495467233522,56.1663620064171));
#40856=CARTESIAN_POINT('Ctrl Pts',(67.5755898002831,263.858999204865,47.2803467149763));
#40857=CARTESIAN_POINT('Ctrl Pts',(75.8081796701991,263.222531176208,43.6889980275431));
#40858=CARTESIAN_POINT('Ctrl Pts',(83.2882343864571,262.586063147551,48.6611306487392));
#40859=CARTESIAN_POINT('Ctrl Pts',(83.1389331100811,261.949595118894,57.6590123618092));
#40860=CARTESIAN_POINT('Ctrl Pts',(76.7742670496182,261.419205095014,61.5823935045322));
#40861=CARTESIAN_POINT('Ctrl Pts',(71.4398434719161,260.994893075909,60.4583899346883));
#40862=CARTESIAN_POINT('Ctrl Pts',(67.2104103072712,260.570581056805,57.0187163982657));
#40863=CARTESIAN_POINT('Ctrl Pts',(66.2565010855456,260.040191032923,49.6030606046766));
#40864=CARTESIAN_POINT('Ctrl Pts',(73.1571307501172,259.403723004267,43.8267749100486));
#40865=CARTESIAN_POINT('Ctrl Pts',(81.7276617814507,258.767254975609,46.5136539921665));
#40866=CARTESIAN_POINT('Ctrl Pts',(84.1147180442186,258.130786946953,55.1724809196061));
#40867=CARTESIAN_POINT('Ctrl Pts',(78.1018348621412,257.494318918295,61.867957156008));
#40868=CARTESIAN_POINT('Ctrl Pts',(70.7238585278493,256.963928894415,60.6566112669601));
#40869=CARTESIAN_POINT('Ctrl Pts',(67.4334230143906,256.53961687531,56.3100617086169));
#40870=CARTESIAN_POINT('Ctrl Pts',(66.4957015356938,256.115304856205,50.9397602869315));
#40871=CARTESIAN_POINT('Ctrl Pts',(70.6381541596617,255.584914832325,44.7154547103664));
#40872=CARTESIAN_POINT('Ctrl Pts',(79.6357826280725,254.948446803668,44.8793087245797));
#40873=CARTESIAN_POINT('Ctrl Pts',(84.3446499226267,254.311978775011,52.5278308147126));
#40874=CARTESIAN_POINT('Ctrl Pts',(80.4690377153397,253.675510746354,60.6304817006697));
#40875=CARTESIAN_POINT('Ctrl Pts',(71.5389167422275,253.039042717697,61.7427341895921));
#40876=CARTESIAN_POINT('Ctrl Pts',(66.762877011925,252.508652693816,55.9902270712261));
#40877=CARTESIAN_POINT('Ctrl Pts',(67.1287601229746,252.084340674712,50.5509634739719));
#40878=CARTESIAN_POINT('Ctrl Pts',(69.9422387447338,251.660028655607,45.8815098682203));
#40879=CARTESIAN_POINT('Ctrl Pts',(77.1512298269574,251.129638631726,43.8984966991504));
#40880=CARTESIAN_POINT('Ctrl Pts',(83.8369722296532,250.493170603069,49.9222011007897));
#40881=CARTESIAN_POINT('Ctrl Pts',(82.3768062577141,249.856702574412,58.7845504899393));
#40882=CARTESIAN_POINT('Ctrl Pts',(74.1375957721407,249.220234545756,62.3606841473118));
#40883=CARTESIAN_POINT('Ctrl Pts',(66.6660428528195,248.583766517098,57.3447033691071));
#40884=CARTESIAN_POINT('Ctrl Pts',(66.8322241000219,248.053376493218,49.8697935070852));
#40885=CARTESIAN_POINT('Ctrl Pts',(70.6751412031906,247.629064474113,46.0030833977625));
#40886=CARTESIAN_POINT('Ctrl Pts',(75.8612007292659,247.204752455009,44.3225342246141));
#40887=CARTESIAN_POINT('Ctrl Pts',(82.6042870466499,246.674362431127,47.5525002567253));
#40888=CARTESIAN_POINT('Ctrl Pts',(83.7020947420946,246.037894402471,56.4844084771085));
#40889=CARTESIAN_POINT('Ctrl Pts',(76.7883844442563,245.401426373813,62.2179877500005));
#40890=CARTESIAN_POINT('Ctrl Pts',(68.2228317834295,244.764958345157,59.5152800381715));
#40891=CARTESIAN_POINT('Ctrl Pts',(65.8709468103568,244.128490316499,50.8289227310511));
#40892=CARTESIAN_POINT('Ctrl Pts',(70.8979193573472,243.598100292619,45.2943549372585));
#40893=CARTESIAN_POINT('Ctrl Pts',(76.3348210323808,243.173788273514,44.8949064332121));
#40894=CARTESIAN_POINT('Ctrl Pts',(81.3522652511927,242.74947625441,47.0267395510882));
#40895=CARTESIAN_POINT('Ctrl Pts',(84.3252993449719,242.219086230529,53.8869845853058));
#40896=CARTESIAN_POINT('Ctrl Pts',(79.297240837648,241.582618201872,61.3504150191248));
#40897=CARTESIAN_POINT('Ctrl Pts',(70.3177403128524,240.946150173215,61.1457404330823));
#40898=CARTESIAN_POINT('Ctrl Pts',(65.6230109474603,240.309682144558,53.4885322246883));
#40899=CARTESIAN_POINT('Ctrl Pts',(69.5432298218416,239.673214115901,45.3881587659845));
#40900=CARTESIAN_POINT('Ctrl Pts',(76.967750906386,239.142824092021,44.5059001205523));
#40901=CARTESIAN_POINT('Ctrl Pts',(81.3345269806457,238.718512072916,47.769445071773));
#40902=CARTESIAN_POINT('Ctrl Pts',(83.724782060455,238.294200053811,52.6690511360203));
#40903=CARTESIAN_POINT('Ctrl Pts',(81.4709617211638,237.76381002993,59.7980193313823));
#40904=CARTESIAN_POINT('Ctrl Pts',(72.7808118995323,237.127342001274,62.1358521464321));
#40905=CARTESIAN_POINT('Ctrl Pts',(66.1355232304304,236.490873972616,56.0932153159349));
#40906=CARTESIAN_POINT('Ctrl Pts',(67.612059031172,235.85440594396,47.2335785632174));
#40907=CARTESIAN_POINT('Ctrl Pts',(75.8834540617522,235.217937915302,43.6884141888023));
#40908=CARTESIAN_POINT('Ctrl Pts',(82.0674696356908,234.687547891422,47.8907760287162));
#40909=CARTESIAN_POINT('Ctrl Pts',(83.2243770613147,234.263235872317,53.2181603906615));
#40910=CARTESIAN_POINT('Ctrl Pts',(81.8162055485238,233.838923853213,58.4847068797696));
#40911=CARTESIAN_POINT('Ctrl Pts',(75.4399144954396,233.308533829332,62.3891666450382));
#40912=CARTESIAN_POINT('Ctrl Pts',(67.345892088715,232.672065800675,58.4558515708228));
#40913=CARTESIAN_POINT('Ctrl Pts',(66.291041376437,232.035597772018,49.5361760534184));
#40914=CARTESIAN_POINT('Ctrl Pts',(73.2153321012232,231.399129743361,43.8153789656575));
#40915=CARTESIAN_POINT('Ctrl Pts',(81.7848765901179,230.762661714704,46.5625727059977));
#40916=CARTESIAN_POINT('Ctrl Pts',(83.698186774302,230.232271690823,53.7903758156054));
#40917=CARTESIAN_POINT('Ctrl Pts',(81.0783348798918,229.807959671719,58.5711534701399));
#40918=CARTESIAN_POINT('Ctrl Pts',(76.5617481587882,229.383647652614,61.6240051409511));
#40919=CARTESIAN_POINT('Ctrl Pts',(69.1874022588527,228.853257628733,60.3907508304615));
#40920=CARTESIAN_POINT('Ctrl Pts',(65.6556204535641,228.216789600076,52.1136327645463));
#40921=CARTESIAN_POINT('Ctrl Pts',(70.7080900492044,227.580321571419,44.687606077119));
#40922=CARTESIAN_POINT('Ctrl Pts',(79.687197132215,226.943853542762,44.9088690599485));
#40923=CARTESIAN_POINT('Ctrl Pts',(84.3557695970477,226.307385514105,52.6022816558166));
#40924=CARTESIAN_POINT('Ctrl Pts',(81.0608424149524,225.776995490225,59.3138648216729));
#40925=CARTESIAN_POINT('Ctrl Pts',(75.9479723037787,225.35268347112,61.2054297859663));
#40926=CARTESIAN_POINT('Ctrl Pts',(70.5361213944014,224.928371452016,60.5486734034489));
#40927=CARTESIAN_POINT('Ctrl Pts',(65.7771886512274,224.397981428134,54.7820060528674));
#40928=CARTESIAN_POINT('Ctrl Pts',(68.5382388443865,223.761513399478,46.216916024055));
#40929=CARTESIAN_POINT('Ctrl Pts',(77.2222924846526,223.125045370821,43.9233299437037));
#40930=CARTESIAN_POINT('Ctrl Pts',(83.8564062843967,222.488577342164,49.9782330272043));
#40931=CARTESIAN_POINT('Ctrl Pts',(82.3363825504368,221.852109313506,58.848052098875));
#40932=CARTESIAN_POINT('Ctrl Pts',(75.4477482643877,221.321719289626,61.7547047329954));
#40933=CARTESIAN_POINT('Ctrl Pts',(70.3471947930426,220.897407270521,59.8301800696257));
#40934=CARTESIAN_POINT('Ctrl Pts',(66.6919112490471,220.473095251417,55.7856301591708));
#40935=CARTESIAN_POINT('Ctrl Pts',(66.880301523413,219.942705227536,48.3112457941265));
#40936=CARTESIAN_POINT('Ctrl Pts',(74.5812401565408,219.306237198879,43.6551244884603));
#40937=CARTESIAN_POINT('Ctrl Pts',(82.6416720877777,218.669769170222,47.6178447743592));
#40938=CARTESIAN_POINT('Ctrl Pts',(83.6799939691614,218.033301141565,56.5394601953136));
#40939=CARTESIAN_POINT('Ctrl Pts',(76.7162878641993,217.396833112908,62.2394157987944));
#40940=CARTESIAN_POINT('Ctrl Pts',(69.6092409969674,216.866443089027,59.9168855034723));
#40941=CARTESIAN_POINT('Ctrl Pts',(67.0205576898783,216.442131069923,55.1192648449001));
#40942=CARTESIAN_POINT('Ctrl Pts',(66.9124473478813,216.017819050818,49.6688377131259));
#40943=CARTESIAN_POINT('Ctrl Pts',(71.9569601804353,215.487429026937,44.1490780730461));
#40944=CARTESIAN_POINT('Ctrl Pts',(80.8222636492987,214.85096099828,45.6837141077411));
#40945=CARTESIAN_POINT('Ctrl Pts',(84.3130014825699,214.214492969623,53.9605188524692));
#40946=CARTESIAN_POINT('Ctrl Pts',(79.2400908333381,213.578024940966,61.3780748791543));
#40947=CARTESIAN_POINT('Ctrl Pts',(70.2576310661073,212.94155691231,61.1135443626181));
#40948=CARTESIAN_POINT('Ctrl Pts',(65.6207844274967,212.305088883652,53.420014571099));
#40949=CARTESIAN_POINT('Ctrl Pts',(69.5979250829234,211.668620854996,45.3496325751228));
#40950=CARTESIAN_POINT('Ctrl Pts',(77.0293989008466,211.138230831115,44.5201429154035));
#40951=CARTESIAN_POINT('Ctrl Pts',(81.3721622592396,210.71391881201,47.8154805578659));
#40952=CARTESIAN_POINT('Ctrl Pts',(83.7271839203301,210.289606792905,52.7320157427041));
#40953=CARTESIAN_POINT('Ctrl Pts',(81.4218657451715,209.759216769025,59.8446643532429));
#40954=CARTESIAN_POINT('Ctrl Pts',(72.7151407986123,209.122748740368,62.1196670571768));
#40955=CARTESIAN_POINT('Ctrl Pts',(66.1135889180742,208.486280711711,56.0292773473689));
#40956=CARTESIAN_POINT('Ctrl Pts',(67.6540268194141,207.849812683054,47.1805053390905));
#40957=CARTESIAN_POINT('Ctrl Pts',(75.9507747452419,207.213344654397,43.6951222468685));
#40958=CARTESIAN_POINT('Ctrl Pts',(82.1043148718093,206.682954630516,47.9419865539333));
#40959=CARTESIAN_POINT('Ctrl Pts',(83.2227524914535,206.258642611411,53.2775820273672));
#40960=CARTESIAN_POINT('Ctrl Pts',(81.7766207124032,205.834330592307,58.5338300971972));
#40961=CARTESIAN_POINT('Ctrl Pts',(75.3723240203356,205.303940568426,62.3921841170279));
#40962=CARTESIAN_POINT('Ctrl Pts',(67.3068916918394,204.667472539769,58.4005724286968));
#40963=CARTESIAN_POINT('Ctrl Pts',(66.3164237824365,204.031004511112,49.4735185709573));
#40964=CARTESIAN_POINT('Ctrl Pts',(73.2818100437565,203.394536482455,43.802829109735));
#40965=CARTESIAN_POINT('Ctrl Pts',(81.8313103627761,202.758068453799,46.6117808120413));
#40966=CARTESIAN_POINT('Ctrl Pts',(83.6924220806197,202.227678429917,53.853200311008));
#40967=CARTESIAN_POINT('Ctrl Pts',(81.0381449774921,201.803366410813,58.6149512779444));
#40968=CARTESIAN_POINT('Ctrl Pts',(76.499649456248,201.379054391708,61.635136237765));
#40969=CARTESIAN_POINT('Ctrl Pts',(69.1343934412748,200.848664367828,60.3487080192437));
#40970=CARTESIAN_POINT('Ctrl Pts',(65.6624230963692,200.21219633917,52.0463235332207));
#40971=CARTESIAN_POINT('Ctrl Pts',(70.7683400725564,199.575728310514,44.6569437792745));
#40972=CARTESIAN_POINT('Ctrl Pts',(79.7456170301404,198.939260281857,44.9429853917731));
#40973=CARTESIAN_POINT('Ctrl Pts',(84.3585598878715,198.3027922532,52.6698815596127));
#40974=CARTESIAN_POINT('Ctrl Pts',(81.0152943056921,197.772402229319,59.3575170829689));
#40975=CARTESIAN_POINT('Ctrl Pts',(75.8889095924911,197.348090210215,61.2121433810362));
#40976=CARTESIAN_POINT('Ctrl Pts',(70.4819380791528,196.92377819111,60.5163575054332));
#40977=CARTESIAN_POINT('Ctrl Pts',(65.7647357358894,196.393388167229,54.7155044901546));
#40978=CARTESIAN_POINT('Ctrl Pts',(68.5875114199334,195.756920138572,46.1705584030409));
#40979=CARTESIAN_POINT('Ctrl Pts',(77.2878870962725,195.120452109915,43.9396876198568));
#40980=CARTESIAN_POINT('Ctrl Pts',(83.8781423559844,194.483984081258,50.042298288482));
#40981=CARTESIAN_POINT('Ctrl Pts',(82.2941616241956,193.847516052601,58.9009195827315));
#40982=CARTESIAN_POINT('Ctrl Pts',(75.3847363513986,193.31712602872,61.7577948078464));
#40983=CARTESIAN_POINT('Ctrl Pts',(70.2981992521546,192.892814009616,59.796519898665));
#40984=CARTESIAN_POINT('Ctrl Pts',(66.6721959932454,192.468501990511,55.7257018853234));
#40985=CARTESIAN_POINT('Ctrl Pts',(66.9145010625479,191.938111966631,48.2528723070669));
#40986=CARTESIAN_POINT('Ctrl Pts',(74.648847973789,191.301643937973,43.6524327574035));
#40987=CARTESIAN_POINT('Ctrl Pts',(82.680452897193,190.665175909317,47.6732092639168));
#40988=CARTESIAN_POINT('Ctrl Pts',(83.6544270164244,190.028707880659,56.6020779367127));
#40989=CARTESIAN_POINT('Ctrl Pts',(76.6496815131711,189.392239852003,62.2516537285915));
#40990=CARTESIAN_POINT('Ctrl Pts',(69.5597509643709,188.861849828122,59.8778848970763));
#40991=CARTESIAN_POINT('Ctrl Pts',(67.0054911824049,188.437537809017,55.0617437137643));
#40992=CARTESIAN_POINT('Ctrl Pts',(66.9372166834158,188.013225789912,49.6106156172916));
#40993=CARTESIAN_POINT('Ctrl Pts',(72.0202984177305,187.482835766032,44.1275349380969));
#40994=CARTESIAN_POINT('Ctrl Pts',(80.8763462373005,186.846367737374,45.7258412951564));
#40995=CARTESIAN_POINT('Ctrl Pts',(84.3036521127895,186.209899708718,54.0280636360005));
#40996=CARTESIAN_POINT('Ctrl Pts',(79.1840926941306,185.573431680061,61.4079981018203));
#40997=CARTESIAN_POINT('Ctrl Pts',(70.1909442437265,184.936963651404,61.0802067924056));
#40998=CARTESIAN_POINT('Ctrl Pts',(66.394611359777,184.406573627523,54.6389530102197));
#40999=CARTESIAN_POINT('Ctrl Pts',(67.6242295079782,183.982261608419,49.3278798473855));
#41000=CARTESIAN_POINT('Ctrl Pts',(71.1471386294461,183.557949589314,45.167522861111));
#41001=CARTESIAN_POINT('Ctrl Pts',(78.5802604721558,183.027559565433,44.3609292064653));
#41002=CARTESIAN_POINT('Ctrl Pts',(84.2184995867349,182.391091536776,51.3748030205826));
#41003=CARTESIAN_POINT('Ctrl Pts',(81.3621086629095,181.754623508119,59.8903389550533));
#41004=CARTESIAN_POINT('Ctrl Pts',(72.6576265185261,181.118155479462,62.1051328414189));
#41005=CARTESIAN_POINT('Ctrl Pts',(66.0827647583405,180.481687450805,55.9605938816611));
#41006=CARTESIAN_POINT('Ctrl Pts',(67.4402524491558,179.951297426925,48.6081030913529));
#41007=CARTESIAN_POINT('Ctrl Pts',(71.8512292228023,179.52698540782,45.4045514944974));
#41008=CARTESIAN_POINT('Ctrl Pts',(77.2390781242549,179.102673388715,44.5735622367552));
#41009=CARTESIAN_POINT('Ctrl Pts',(83.3799716108488,178.572283364835,48.8386907035881));
#41010=CARTESIAN_POINT('Ctrl Pts',(83.0376354525052,177.935815336178,57.83129723052));
#41011=CARTESIAN_POINT('Ctrl Pts',(75.2971941772932,177.299347307521,62.3874897446671));
#41012=CARTESIAN_POINT('Ctrl Pts',(67.2730309492928,176.662879278864,58.351882497749));
#41013=CARTESIAN_POINT('Ctrl Pts',(66.3381724278209,176.026411250207,49.4014520199251));
#41014=CARTESIAN_POINT('Ctrl Pts',(72.1843046459954,175.496021226326,44.7404830498607));
#41015=CARTESIAN_POINT('Ctrl Pts',(77.6152384240311,175.071709207222,45.2142100070392));
#41016=CARTESIAN_POINT('Ctrl Pts',(82.2279530476807,174.647397188116,48.1197775474917));
#41017=CARTESIAN_POINT('Ctrl Pts',(84.0675483467432,174.117007164236,55.3666929456424));
#41018=CARTESIAN_POINT('Ctrl Pts',(77.9123834182491,173.480539135579,61.9316080933473));
#41019=CARTESIAN_POINT('Ctrl Pts',(69.0807483806694,172.844071106922,60.2958990960111));
#41020=CARTESIAN_POINT('Ctrl Pts',(65.668785894465,172.207603078265,51.9873593113253));
#41021=CARTESIAN_POINT('Ctrl Pts',(70.8320161622452,171.571135049608,44.6167949234776));
#41022=CARTESIAN_POINT('Ctrl Pts',(78.3021576349833,171.040745025728,44.9312468745954));
#41023=CARTESIAN_POINT('Ctrl Pts',(82.0918625454198,170.616433006623,48.850123706441));
#41024=CARTESIAN_POINT('Ctrl Pts',(83.6691886717045,170.192120987518,54.0685047985716));
#41025=CARTESIAN_POINT('Ctrl Pts',(80.3060744937362,169.661730963637,60.7461807923759));
#41026=CARTESIAN_POINT('Ctrl Pts',(71.3541437074611,169.025262934981,61.6665619043428));
#41027=CARTESIAN_POINT('Ctrl Pts',(65.7588621303524,168.388794906323,54.6404573339678));
#41028=CARTESIAN_POINT('Ctrl Pts',(68.6309797965831,167.752326877667,46.1302128326447));
#41029=CARTESIAN_POINT('Ctrl Pts',(77.3622890976487,167.11585884901,43.9511295201827));
#41030=CARTESIAN_POINT('Ctrl Pts',(82.7960315486792,166.585468825129,49.0869192966586));
#41031=CARTESIAN_POINT('Ctrl Pts',(83.0875324231865,166.161156806024,54.5306759197567));
#41032=CARTESIAN_POINT('Ctrl Pts',(80.8565720249266,165.73684478692,59.5048366160715));
#41033=CARTESIAN_POINT('Ctrl Pts',(73.9386918548011,165.206454763039,62.3411771464144));
#41034=CARTESIAN_POINT('Ctrl Pts',(66.5764879777522,164.569986734382,57.166032678258));
#41035=CARTESIAN_POINT('Ctrl Pts',(66.9592770116748,163.933518705725,48.1923604134332));
#41036=CARTESIAN_POINT('Ctrl Pts',(74.7081221966236,163.297050677068,43.6504753795876));
#41037=CARTESIAN_POINT('Ctrl Pts',(82.7291234421973,162.660582648411,47.7306353289073));
#41038=CARTESIAN_POINT('Ctrl Pts',(83.463904735118,162.13019262453,55.1711991586084));
#41039=CARTESIAN_POINT('Ctrl Pts',(80.1143646250949,161.705880605426,59.4723664400229));
#41040=CARTESIAN_POINT('Ctrl Pts',(75.1682999312516,161.281568586321,61.7649420605167));
#41041=CARTESIAN_POINT('Ctrl Pts',(68.0854511270769,160.75117856244,59.3701254768339));
#41042=CARTESIAN_POINT('Ctrl Pts',(65.9204924507741,160.114710533783,50.6353032048341));
#41043=CARTESIAN_POINT('Ctrl Pts',(72.0937834729716,159.478242505126,44.1112094504318));
#41044=CARTESIAN_POINT('Ctrl Pts',(80.9223816280249,158.841774476469,45.7632312352661));
#41045=CARTESIAN_POINT('Ctrl Pts',(84.3027423805713,158.205306447812,54.1033347943454));
#41046=CARTESIAN_POINT('Ctrl Pts',(79.9785158501795,157.674916423932,60.2027576003278));
#41047=CARTESIAN_POINT('Ctrl Pts',(74.6292268764211,157.250604404827,61.2537411428208));
#41048=CARTESIAN_POINT('Ctrl Pts',(69.3916553792759,156.826292385722,59.7413576783326));
#41049=CARTESIAN_POINT('Ctrl Pts',(65.6144707901074,156.295902361841,53.288856594905));
#41050=CARTESIAN_POINT('Ctrl Pts',(69.7075983555732,155.659434333185,45.274464981916));
#41051=CARTESIAN_POINT('Ctrl Pts',(78.64644657324,155.022966304528,44.3967896988572));
#41052=CARTESIAN_POINT('Ctrl Pts',(84.2287385638327,154.386498275871,51.4332190129864));
#41053=CARTESIAN_POINT('Ctrl Pts',(81.3120644269999,153.750030247214,59.9465719466464));
#41054=CARTESIAN_POINT('Ctrl Pts',(74.0477236227788,153.219640223333,61.7161047472509));
#41055=CARTESIAN_POINT('Ctrl Pts',(69.3198652774232,152.795328204229,59.0019171344252));
#41056=CARTESIAN_POINT('Ctrl Pts',(66.3572243229997,152.371016185123,54.4256503691965));
#41057=CARTESIAN_POINT('Ctrl Pts',(67.7365440944563,151.840626161243,47.0772239648329));
#41058=CARTESIAN_POINT('Ctrl Pts',(76.0821040501351,151.204158132586,43.710356693956));
#41059=CARTESIAN_POINT('Ctrl Pts',(83.406427223103,150.567690103929,48.9091653477627));
#41060=CARTESIAN_POINT('Ctrl Pts',(83.0070608638056,149.931222075272,57.8821151343176));
#41061=CARTESIAN_POINT('Ctrl Pts',(75.2225373742539,149.294754046615,62.3971301103889));
#41062=CARTESIAN_POINT('Ctrl Pts',(68.5776471717109,148.764364022734,58.9696926057169));
#41063=CARTESIAN_POINT('Ctrl Pts',(66.7878946983978,148.34005200363,53.8202999215615));
#41064=CARTESIAN_POINT('Ctrl Pts',(67.5518938036794,147.915739984525,48.4225444344639));
#41065=CARTESIAN_POINT('Ctrl Pts',(73.4118440549937,147.385349960644,43.7789599672223));
#41066=CARTESIAN_POINT('Ctrl Pts',(81.9204685029185,146.748881931987,46.7093995584277));
#41067=CARTESIAN_POINT('Ctrl Pts',(84.0413100822046,146.112413903331,55.4372487984491));
#41068=CARTESIAN_POINT('Ctrl Pts',(77.8559769716525,145.475945874673,61.9499268706774));
#41069=CARTESIAN_POINT('Ctrl Pts',(69.0180612333034,144.839477846017,60.2542230063861));
#41070=CARTESIAN_POINT('Ctrl Pts',(66.2486524828672,144.309087822136,53.3092774468237));
#41071=CARTESIAN_POINT('Ctrl Pts',(68.2739939265614,143.884775803031,48.2479089591696));
#41072=CARTESIAN_POINT('Ctrl Pts',(72.3902695459265,143.460463783926,44.6735930866159));
#41073=CARTESIAN_POINT('Ctrl Pts',(79.8594440960063,142.930073760046,45.0102311603966));
#41074=CARTESIAN_POINT('Ctrl Pts',(84.3618626866762,142.293605731389,52.8020469325975));
#41075=CARTESIAN_POINT('Ctrl Pts',(80.2399992388539,141.657137702732,60.7822451180113));
#41076=CARTESIAN_POINT('Ctrl Pts',(71.2995448559428,141.020669674075,61.6434052587863));
#41077=CARTESIAN_POINT('Ctrl Pts',(65.7388616677646,140.384201645418,54.5678862902412));
#41078=CARTESIAN_POINT('Ctrl Pts',(68.2019590988151,139.853811621537,47.5084922158581));
#41079=CARTESIAN_POINT('Ctrl Pts',(73.049966590537,139.429499602433,45.0152448772302));
#41080=CARTESIAN_POINT('Ctrl Pts',(78.5015222053076,139.005187583328,45.0158020357968));
#41081=CARTESIAN_POINT('Ctrl Pts',(83.919986575027,138.474797559447,50.1677082389766));
#41082=CARTESIAN_POINT('Ctrl Pts',(82.2099907202014,137.83832953079,59.0028698317267));
#41083=CARTESIAN_POINT('Ctrl Pts',(73.8651568290306,137.201861502133,62.3250782372519));
#41084=CARTESIAN_POINT('Ctrl Pts',(66.5504504432737,136.565393473476,57.1127474868928));
#41085=CARTESIAN_POINT('Ctrl Pts',(66.9917635648296,135.928925444819,48.124454605468));
#41086=CARTESIAN_POINT('Ctrl Pts',(73.480436591811,135.398535420938,44.4097519254127));
#41087=CARTESIAN_POINT('Ctrl Pts',(78.7755611796576,134.974223401834,45.7063299333033));
#41088=CARTESIAN_POINT('Ctrl Pts',(82.8911061103094,134.549911382729,49.2814871123865));
#41089=CARTESIAN_POINT('Ctrl Pts',(83.6037845027795,134.019521358848,56.7242005397054));
#41090=CARTESIAN_POINT('Ctrl Pts',(76.5192810884573,133.383053330192,62.2734326997418));
#41091=CARTESIAN_POINT('Ctrl Pts',(68.0404888765095,132.746585301534,59.3097518823143));
#41092=CARTESIAN_POINT('Ctrl Pts',(65.935774761008,132.110117272878,50.577999489296));
#41093=CARTESIAN_POINT('Ctrl Pts',(72.1628384614155,131.473649244221,44.08124307824));
#41094=CARTESIAN_POINT('Ctrl Pts',(79.4976034645514,130.94325922034,45.531455476841));
#41095=CARTESIAN_POINT('Ctrl Pts',(82.6452064879334,130.518947201235,49.9825288461035));
#41096=CARTESIAN_POINT('Ctrl Pts',(83.4081022570692,130.094635182131,55.3804403845415));
#41097=CARTESIAN_POINT('Ctrl Pts',(79.0657785435674,129.56424515825,61.4669926450126));
#41098=CARTESIAN_POINT('Ctrl Pts',(70.0782111864052,128.927777129593,61.0111426762753));
#41099=CARTESIAN_POINT('Ctrl Pts',(65.6201130519864,128.291309100936,53.2137916911737));
#41100=CARTESIAN_POINT('Ctrl Pts',(69.7567120988123,127.654841072279,45.241221861641));
#41101=CARTESIAN_POINT('Ctrl Pts',(78.7182326925333,127.018373043622,44.4194464410791));
#41102=CARTESIAN_POINT('Ctrl Pts',(83.3050165716072,126.487983019741,50.323962280583));
#41103=CARTESIAN_POINT('Ctrl Pts',(82.7627561352269,126.063671000637,55.7484818492179));
#41104=CARTESIAN_POINT('Ctrl Pts',(79.7991798376885,125.639358981532,60.3241429446261));
#41105=CARTESIAN_POINT('Ctrl Pts',(72.5296152817953,125.108968957651,62.0720916910074));
#41106=CARTESIAN_POINT('Ctrl Pts',(66.0429388543689,124.472500928994,55.8345284553034));
#41107=CARTESIAN_POINT('Ctrl Pts',(67.7900261310386,123.836032900337,47.0242499461599));
#41108=CARTESIAN_POINT('Ctrl Pts',(76.1409832360778,123.19956487168,43.7174634712323));
#41109=CARTESIAN_POINT('Ctrl Pts',(83.4457689004487,122.563096843024,48.9733432825609));
#41110=CARTESIAN_POINT('Ctrl Pts',(83.0370236359612,122.032706819143,56.438919011267));
#41111=CARTESIAN_POINT('Ctrl Pts',(79.0706101813766,121.608394800038,60.1788419033402));
#41112=CARTESIAN_POINT('Ctrl Pts',(73.8327296571528,121.184082780934,61.6901547582187));
#41113=CARTESIAN_POINT('Ctrl Pts',(67.1980487999333,120.653692757053,58.2429959897354));
#41114=CARTESIAN_POINT('Ctrl Pts',(66.3907685778263,120.017224728396,49.2801579996498));
#41115=CARTESIAN_POINT('Ctrl Pts',(73.48695938946,119.380756699739,43.774034379002));
#41116=CARTESIAN_POINT('Ctrl Pts',(81.9602620234156,118.744288671082,46.7533738753299));
#41117=CARTESIAN_POINT('Ctrl Pts',(84.0289296905471,118.107820642425,55.5115004031035));
#41118=CARTESIAN_POINT('Ctrl Pts',(78.8249425935863,117.577430618544,60.8799649831249));
#41119=CARTESIAN_POINT('Ctrl Pts',(73.3779393972438,117.153118599439,61.1027094789036));
#41120=CARTESIAN_POINT('Ctrl Pts',(68.4323434172374,116.728806580335,58.8091229133018));
#41121=CARTESIAN_POINT('Ctrl Pts',(65.6835744766738,116.198416556454,51.8559824024478));
#41122=CARTESIAN_POINT('Ctrl Pts',(70.9512619784509,115.561948527797,44.5597070117332));
#41123=CARTESIAN_POINT('Ctrl Pts',(79.9193858227639,114.92548049914,45.055767566542));
#41124=CARTESIAN_POINT('Ctrl Pts',(84.3630715091719,114.289012470483,52.8613411445304));
#41125=CARTESIAN_POINT('Ctrl Pts',(80.1819632346659,113.652544441826,60.8301867190402));
#41126=CARTESIAN_POINT('Ctrl Pts',(72.7327151200314,113.122154417945,61.4709645111751));
#41127=CARTESIAN_POINT('Ctrl Pts',(68.4741821526868,112.697842398841,58.0673846461795));
#41128=CARTESIAN_POINT('Ctrl Pts',(66.2442385369553,112.273530379736,53.0927680376334));
#41129=CARTESIAN_POINT('Ctrl Pts',(68.7282926279591,111.743140355855,46.0407208933463));
#41130=CARTESIAN_POINT('Ctrl Pts',(77.4897535082816,111.106672327198,43.9862210914205));
#41131=CARTESIAN_POINT('Ctrl Pts',(83.9353829353853,110.470204298542,50.2413935630175));
#41132=CARTESIAN_POINT('Ctrl Pts',(82.1720225153696,109.833736269885,59.0484294656406));
#41133=CARTESIAN_POINT('Ctrl Pts',(73.7899031570053,109.197268241228,62.3232182001498));
#41134=CARTESIAN_POINT('Ctrl Pts',(67.7455644465447,108.666878217347,57.922324744781));
#41135=CARTESIAN_POINT('Ctrl Pts',(66.7622050692158,108.242566198242,52.5601924015445));
#41136=CARTESIAN_POINT('Ctrl Pts',(68.3405978179793,107.818254179138,47.34213382943));
#41137=CARTESIAN_POINT('Ctrl Pts',(74.8402754823346,107.287864155257,43.6467199267987));
#41138=CARTESIAN_POINT('Ctrl Pts',(82.802348221357,106.6513961266,47.8407113302285));
#41139=CARTESIAN_POINT('Ctrl Pts',(83.5670911998759,106.014928097943,56.7899285886139));
#41140=CARTESIAN_POINT('Ctrl Pts',(76.4607404746586,105.378460069286,62.2829332974389));
#41141=CARTESIAN_POINT('Ctrl Pts',(67.9848922283654,104.741992040629,59.2590016349609));
#41142=CARTESIAN_POINT('Ctrl Pts',(66.3072204096844,104.211602016748,51.972897674607));
#41143=CARTESIAN_POINT('Ctrl Pts',(69.0808858451976,103.787289997644,47.2796856632862));
#41144=CARTESIAN_POINT('Ctrl Pts',(73.6941942806995,103.362977978539,44.3750610386075));
#41145=CARTESIAN_POINT('Ctrl Pts',(81.0246195689312,102.832587954658,45.847052460437));
#41146=CARTESIAN_POINT('Ctrl Pts',(84.2858470046237,102.196119926001,54.2344574110884));
#41147=CARTESIAN_POINT('Ctrl Pts',(78.9949754871697,101.559651897344,61.4925563320708));
#41148=CARTESIAN_POINT('Ctrl Pts',(70.0277833696733,100.923183868687,60.9799288953412));
#41149=CARTESIAN_POINT('Ctrl Pts',(65.6114160752346,100.28671584003,53.1390191194198));
#41150=CARTESIAN_POINT('Ctrl Pts',(69.1224790880608,99.7563258161497,46.5379335895811));
#41151=CARTESIAN_POINT('Ctrl Pts',(74.2940588091507,99.3320137970449,44.8133402694683));
#41152=CARTESIAN_POINT('Ctrl Pts',(79.6817377409247,98.9077017779405,45.645430805096));
#41153=CARTESIAN_POINT('Ctrl Pts',(84.2509640357489,98.3773117540596,51.5635440786798));
#41154=CARTESIAN_POINT('Ctrl Pts',(81.2133277182638,97.7408437254026,60.0344904128399));
#41155=CARTESIAN_POINT('Ctrl Pts',(72.4593963387556,97.1043756967459,62.0449646762496));
#41156=CARTESIAN_POINT('Ctrl Pts',(66.0253337278694,96.4679076680886,55.7778952111669));
#41157=CARTESIAN_POINT('Ctrl Pts',(67.8324903896393,95.8314396394319,46.9620940000828));
#41158=CARTESIAN_POINT('Ctrl Pts',(74.8118490485081,95.3010496155511,44.2805932331342));
#41159=CARTESIAN_POINT('Ctrl Pts',(79.8472420235469,94.8767375964464,46.3696783243398));
#41160=CARTESIAN_POINT('Ctrl Pts',(83.3693006798349,94.4524255773417,50.5307553187046));
#41161=CARTESIAN_POINT('Ctrl Pts',(82.9383832695932,93.9220355534611,57.995084078736));
#41162=CARTESIAN_POINT('Ctrl Pts',(75.0903408348937,93.285567524804,62.3987639191292));
#41163=CARTESIAN_POINT('Ctrl Pts',(67.162821618513,92.6490994961473,58.1764706518527));
#41164=CARTESIAN_POINT('Ctrl Pts',(66.414612745349,92.0126314674902,49.2258558772637));
#41165=CARTESIAN_POINT('Ctrl Pts',(73.5597771752602,91.3761634388332,43.7549517963041));
#41166=CARTESIAN_POINT('Ctrl Pts',(80.5875093419881,90.8457734149524,46.3069851513022));
#41167=CARTESIAN_POINT('Ctrl Pts',(83.0193467550868,90.4214613958478,51.186086065161));
#41168=CARTESIAN_POINT('Ctrl Pts',(82.9499580277891,89.9971493767431,56.6372000922097));
#41169=CARTESIAN_POINT('Ctrl Pts',(77.7300486906101,89.4667593528625,61.9901843219554));
#41170=CARTESIAN_POINT('Ctrl Pts',(68.9171818569722,88.8302913242055,60.168771582871));
#41171=CARTESIAN_POINT('Ctrl Pts',(65.700600559468,88.1938232955485,51.7826565039134));
#41172=CARTESIAN_POINT('Ctrl Pts',(71.0048716735689,87.5573552668916,44.5343443342367));
#41173=CARTESIAN_POINT('Ctrl Pts',(79.9868760409975,86.9208872382345,45.0891089122556));
#41174=CARTESIAN_POINT('Ctrl Pts',(83.6193563062945,86.3904972143539,51.6241667371345));
#41175=CARTESIAN_POINT('Ctrl Pts',(82.2560251437057,85.9661851952492,56.902498582754));
#41176=CARTESIAN_POINT('Ctrl Pts',(78.6291898710409,85.5418731761446,60.9725753432482));
#41177=CARTESIAN_POINT('Ctrl Pts',(71.1780714024604,85.0114831522638,61.5912248558673));
#41178=CARTESIAN_POINT('Ctrl Pts',(65.7187308749215,84.3750151236068,54.4372212775972));
#41179=CARTESIAN_POINT('Ctrl Pts',(68.7892291056127,83.7385470949501,45.996524506815));
#41180=CARTESIAN_POINT('Ctrl Pts',(77.5468597008283,83.1020790662928,44.0022257030456));
#41181=CARTESIAN_POINT('Ctrl Pts',(83.9644750271765,82.4656110376362,50.3108214038772));
#41182=CARTESIAN_POINT('Ctrl Pts',(82.4217691187119,81.9352210137552,57.6266912860082));
#41183=CARTESIAN_POINT('Ctrl Pts',(77.9313087594824,81.5109089946506,60.717843934059));
#41184=CARTESIAN_POINT('Ctrl Pts',(72.5241951379537,81.0865969755461,61.4125245910826));
#41185=CARTESIAN_POINT('Ctrl Pts',(66.4929544430065,80.5562069516651,56.9936978993126));
#41186=CARTESIAN_POINT('Ctrl Pts',(67.062245548944,79.9197389230083,48.0126025412713));
#41187=CARTESIAN_POINT('Ctrl Pts',(74.9152631630308,79.2832708943513,43.6533095121423));
#41188=CARTESIAN_POINT('Ctrl Pts',(82.8349685791922,78.6468028656944,47.8902408878197));
#41189=CARTESIAN_POINT('Ctrl Pts',(83.5435298885395,78.0103348370374,56.8614229205523));
#41190=CARTESIAN_POINT('Ctrl Pts',(77.5815717462269,77.4799448131566,61.3732904675436));
#41191=CARTESIAN_POINT('Ctrl Pts',(72.164331182832,77.0556327940521,60.7625830010131));
#41192=CARTESIAN_POINT('Ctrl Pts',(67.6264530835239,76.6313207749473,57.7414704100648));
#41193=CARTESIAN_POINT('Ctrl Pts',(65.9704295539125,76.1009307510667,50.4504156357781));
#41194=CARTESIAN_POINT('Ctrl Pts',(72.2893966827277,75.4644627224096,44.0430120572231));
#41195=CARTESIAN_POINT('Ctrl Pts',(81.0769140980902,74.8279946937527,45.9011990864744));
#41196=CARTESIAN_POINT('Ctrl Pts',(84.2779973823023,74.1915266650957,54.2932421731437));
#41197=CARTESIAN_POINT('Ctrl Pts',(78.9303059381265,73.5550586364389,61.5310845596158));
#41198=CARTESIAN_POINT('Ctrl Pts',(71.4704861415877,73.024668612558,61.0281111453561));
#41199=CARTESIAN_POINT('Ctrl Pts',(67.7809414994357,72.6003565934535,57.0147934075068));
#41200=CARTESIAN_POINT('Ctrl Pts',(66.3358828547326,72.1760445743488,51.7582484923816));
#41201=CARTESIAN_POINT('Ctrl Pts',(69.8665366556498,71.645654550468,45.167620495722));
#41202=CARTESIAN_POINT('Ctrl Pts',(78.8388529626364,71.009186521811,44.4735698629039));
#41203=CARTESIAN_POINT('Ctrl Pts',(84.2549408213817,70.3727184931542,51.6387156162939));
#41204=CARTESIAN_POINT('Ctrl Pts',(81.1688544716568,69.7362504644971,60.0737255394068));
#41205=CARTESIAN_POINT('Ctrl Pts',(72.385306968269,69.0997824358402,62.0316477669905));
#41206=CARTESIAN_POINT('Ctrl Pts',(67.0829761186137,68.5693924119593,56.7602929873277));
#41207=CARTESIAN_POINT('Ctrl Pts',(66.9290235122682,68.1450803928548,51.3109115979991));
#41208=CARTESIAN_POINT('Ctrl Pts',(69.2848705936376,67.7207683737502,46.3946687784702));
#41209=CARTESIAN_POINT('Ctrl Pts',(76.2721629512954,67.1903783498693,43.7339096460225));
#41210=CARTESIAN_POINT('Ctrl Pts',(83.5013466579915,66.5539103212124,49.0933003882955));
#41211=CARTESIAN_POINT('Ctrl Pts',(82.8920936660021,65.9174422925556,58.0544460824981));
#41212=CARTESIAN_POINT('Ctrl Pts',(75.0310360867532,65.2809742638985,62.3992239935898));
#41213=CARTESIAN_POINT('Ctrl Pts',(67.1156166044769,64.6445062352416,58.11783396077));
#41214=CARTESIAN_POINT('Ctrl Pts',(66.568944468159,64.1141162113608,50.6610891463319));
#41215=CARTESIAN_POINT('Ctrl Pts',(70.0260214775475,63.6898041922562,46.4458694032433));
#41216=CARTESIAN_POINT('Ctrl Pts',(75.028396930057,63.2654921731517,44.2789132976665));
#41217=CARTESIAN_POINT('Ctrl Pts',(82.0485181524915,62.7351021492707,46.8518088794201));
#41218=CARTESIAN_POINT('Ctrl Pts',(83.9922315445127,62.0986341206139,55.6385115853959));
#41219=CARTESIAN_POINT('Ctrl Pts',(77.6561748449408,61.4621660919568,62.0046491004664));
#41220=CARTESIAN_POINT('Ctrl Pts',(68.8721052431446,60.8256980632999,60.13023116634));
#41221=CARTESIAN_POINT('Ctrl Pts',(65.7034106049201,60.189230034643,51.7074323154109));
#41222=CARTESIAN_POINT('Ctrl Pts',(70.1802693794732,59.6588400107622,45.719141310041));
#41223=CARTESIAN_POINT('Ctrl Pts',(75.5543902423377,59.2345279916576,44.8035628684599));
#41224=CARTESIAN_POINT('Ctrl Pts',(80.7521040083146,58.8102159725529,46.4477132686177));
#41225=CARTESIAN_POINT('Ctrl Pts',(84.3651580886292,58.2798259486721,52.993531312606));
#41226=CARTESIAN_POINT('Ctrl Pts',(80.0709714679809,57.6433579200152,60.902015836241));
#41227=CARTESIAN_POINT('Ctrl Pts',(71.112811884322,57.0068898913583,61.5537045922262));
#41228=CARTESIAN_POINT('Ctrl Pts',(65.7099701712437,56.3704218627013,54.3785653751525));
#41229=CARTESIAN_POINT('Ctrl Pts',(68.8406772736282,55.7339538340444,45.9415730655311));
#41230=CARTESIAN_POINT('Ctrl Pts',(76.1473828139961,55.2035638101635,44.3560296890693));
#41231=CARTESIAN_POINT('Ctrl Pts',(80.805200283045,54.779251791059,47.1887307598465));
#41232=CARTESIAN_POINT('Ctrl Pts',(83.6513455125856,54.3549397719544,51.8383453958925));
#41233=CARTESIAN_POINT('Ctrl Pts',(82.0869171103928,53.8245497480736,59.1496009260114));
#41234=CARTESIAN_POINT('Ctrl Pts',(73.6590043141352,53.1880817194166,62.3046686102621));
#41235=CARTESIAN_POINT('Ctrl Pts',(66.4682867565965,52.5516136907597,56.9225777183616));
#41236=CARTESIAN_POINT('Ctrl Pts',(67.0940935459028,51.9151456621027,47.9625728509838));
#41237=CARTESIAN_POINT('Ctrl Pts',(74.9901395829951,51.2786776334457,43.6455573108627));
#41238=CARTESIAN_POINT('Ctrl Pts',(81.5463680720391,50.748287609565,47.2396860859249));
#41239=CARTESIAN_POINT('Ctrl Pts',(83.2055272982663,50.3239755904603,52.4326283726629));
#41240=CARTESIAN_POINT('Ctrl Pts',(82.3054779870697,49.8996635713557,57.8093718265372));
#41241=CARTESIAN_POINT('Ctrl Pts',(76.3301451774869,49.369273547475,62.303511506943));
#41242=CARTESIAN_POINT('Ctrl Pts',(67.8982274249162,48.7328055188179,59.1591627337605));
#41243=CARTESIAN_POINT('Ctrl Pts',(65.9984409942062,48.096337490161,50.380544797054));
#41244=CARTESIAN_POINT('Ctrl Pts',(72.3462476957355,47.4598694615041,44.0261233882245));
#41245=CARTESIAN_POINT('Ctrl Pts',(81.1385289337613,46.8234014328471,45.9444447442511));
#41246=CARTESIAN_POINT('Ctrl Pts',(83.7316942230129,46.2930114089664,52.9571038287145));
#41247=CARTESIAN_POINT('Ctrl Pts',(81.5791985335305,45.8686993898618,57.9657185312172));
#41248=CARTESIAN_POINT('Ctrl Pts',(77.3739835375813,45.4443873707569,61.4349584723578));
#41249=CARTESIAN_POINT('Ctrl Pts',(69.9156905569373,44.9139973468764,60.9098304240122));
#41250=CARTESIAN_POINT('Ctrl Pts',(65.6114515168285,44.2775293182193,53.0068124891259));
#41251=CARTESIAN_POINT('Ctrl Pts',(69.9335014708324,43.6410612895624,45.1332360745562));
#41252=CARTESIAN_POINT('Ctrl Pts',(78.8928496988574,43.0045932609056,44.4980977510727));
#41253=CARTESIAN_POINT('Ctrl Pts',(84.2731024819777,42.3681252322484,51.7117685353029));
#41254=CARTESIAN_POINT('Ctrl Pts',(81.6325400570954,41.8377352083678,58.7067184087889));
#41255=CARTESIAN_POINT('Ctrl Pts',(76.7231235643936,41.413423189263,61.0767582043516));
#41256=CARTESIAN_POINT('Ctrl Pts',(71.2733201606874,40.9891111701586,60.9385489705161));
#41257=CARTESIAN_POINT('Ctrl Pts',(65.9866694623412,40.4587211462777,55.6514686754988));
#41258=CARTESIAN_POINT('Ctrl Pts',(67.9192087097107,39.8222531176208,46.8623015789586));
#41259=CARTESIAN_POINT('Ctrl Pts',(76.3452680327245,39.1857850889638,43.7518601880908));
#41260=CARTESIAN_POINT('Ctrl Pts',(83.5260304351007,38.5493170603069,49.1472260405232));
#41261=CARTESIAN_POINT('Ctrl Pts',(82.8579028431224,37.9128490316499,58.1215099514755));
#41262=CARTESIAN_POINT('Ctrl Pts',(76.2775020620698,37.3824590077692,61.6711886993321));
#41263=CARTESIAN_POINT('Ctrl Pts',(71.0168044487598,36.9581469886645,60.2413217290587));
#41264=CARTESIAN_POINT('Ctrl Pts',(66.9928447242639,36.5338349695599,56.5633865655431));
#41265=CARTESIAN_POINT('Ctrl Pts',(66.4683227187594,36.0034449456791,49.1050509390183));
#41266=CARTESIAN_POINT('Ctrl Pts',(73.6906859447653,35.3669769170221,43.7364723910789));
#41267=CARTESIAN_POINT('Ctrl Pts',(82.0919416290415,34.7305088883652,46.9132985255213));
#41268=CARTESIAN_POINT('Ctrl Pts',(83.9755071830147,34.0940408597083,55.6954111508481));
#41269=CARTESIAN_POINT('Ctrl Pts',(77.5863852200769,33.4575728310513,62.0328622739661));
#41270=CARTESIAN_POINT('Ctrl Pts',(70.2905767805001,32.9271828071705,60.3979087989981));
#41271=CARTESIAN_POINT('Ctrl Pts',(67.2563673100594,32.5028707880659,55.8687773349566));
#41272=CARTESIAN_POINT('Ctrl Pts',(66.6300125136881,32.0785587689612,50.4533236506808));
#41273=CARTESIAN_POINT('Ctrl Pts',(71.1246377186793,31.5481687450805,44.4783560439785));
#41274=CARTESIAN_POINT('Ctrl Pts',(80.0978292805397,30.9117007164235,45.1609975264086));
#41275=CARTESIAN_POINT('Ctrl Pts',(84.3576222297789,30.2752326877666,53.0684298181443));
#41276=CARTESIAN_POINT('Ctrl Pts',(80.0210339933028,29.6387646591097,60.9340082261254));
#41277=CARTESIAN_POINT('Ctrl Pts',(71.0416207354475,29.0022966304526,61.5292424780427));
#41278=CARTESIAN_POINT('Ctrl Pts',(66.6053888241581,28.471906606572,55.5107924815076));
#41279=CARTESIAN_POINT('Ctrl Pts',(67.2844459508887,28.0475945874673,50.1016945997134));
#41280=CARTESIAN_POINT('Ctrl Pts',(70.3626132162843,27.6232825683627,45.6023228604246));
#41281=CARTESIAN_POINT('Ctrl Pts',(77.6739958051555,27.0928925444818,44.0384887347478));
#41282=CARTESIAN_POINT('Ctrl Pts',(84.0011051141402,26.456424515825,50.4378520405945));
#41283=CARTESIAN_POINT('Ctrl Pts',(82.0321144470125,25.8199564871679,59.2012080002241));
#41284=CARTESIAN_POINT('Ctrl Pts',(73.6003234993231,25.183488458511,62.2960766909906));
#41285=CARTESIAN_POINT('Ctrl Pts',(66.4305778201804,24.5470204298541,56.8574282604532));
#41286=CARTESIAN_POINT('Ctrl Pts',(67.0277000252806,24.0166304059734,49.404549832749));
#41287=CARTESIAN_POINT('Ctrl Pts',(71.087281001366,23.5923183868687,45.7659773340634));
#41288=CARTESIAN_POINT('Ctrl Pts',(76.3616547019156,23.1680063677641,44.3873920955271));
#41289=CARTESIAN_POINT('Ctrl Pts',(82.9071737981875,22.6376163438832,48.0010028147332));
#41290=CARTESIAN_POINT('Ctrl Pts',(83.4878939142026,22.0011483152263,56.9813219696603));
#41291=CARTESIAN_POINT('Ctrl Pts',(76.2549182840066,21.3646802865694,62.3065904942583));
#41292=CARTESIAN_POINT('Ctrl Pts',(67.8595780289596,20.7282122579124,59.1140998978481));
#41293=CARTESIAN_POINT('Ctrl Pts',(66.0126504674273,20.0917442292555,50.306823428731));
#41294=CARTESIAN_POINT('Ctrl Pts',(71.3506474699067,19.5613542053747,45.0709387852651));
#41295=CARTESIAN_POINT('Ctrl Pts',(76.8013676315427,19.13704218627,44.986593912523));
#41296=CARTESIAN_POINT('Ctrl Pts',(81.6878086862886,18.7127301671654,47.4027719979591));
#41297=CARTESIAN_POINT('Ctrl Pts',(84.2593913555,18.1823401432847,54.4265435254333));
#41298=CARTESIAN_POINT('Ctrl Pts',(78.8105057472924,17.5458721146277,61.5812140877453));
#41299=CARTESIAN_POINT('Ctrl Pts',(69.8553503280536,16.9094040859708,60.8700036609127));
#41300=CARTESIAN_POINT('Ctrl Pts',(65.6148282883278,16.2729360573138,52.9336653886293));
#41301=CARTESIAN_POINT('Ctrl Pts',(69.2571180034507,15.742546033433,46.4187817991452));
#41302=CARTESIAN_POINT('Ctrl Pts',(74.4817461662636,15.3182340143284,44.7908493746173));
#41303=CARTESIAN_POINT('Ctrl Pts',(77.1471440252829,15.1060780047761,45.284124068141));
#41304=CARTESIAN_POINT('Ctrl Pts',(78.3434537325882,14.9999999999999,45.8432414056378));
#41305=CARTESIAN_POINT('Ctrl Pts',(68.7814015540657,416.407550721688,56.6017518575033));
#41306=CARTESIAN_POINT('Ctrl Pts',(68.1850535830631,416.301472716912,55.5675736979236));
#41307=CARTESIAN_POINT('Ctrl Pts',(67.5341159529618,416.089316707359,53.2050722594426));
#41308=CARTESIAN_POINT('Ctrl Pts',(68.5953548805507,415.665004688255,48.3730012520256));
#41309=CARTESIAN_POINT('Ctrl Pts',(74.1809818384847,415.134614664374,44.5872815646217));
#41310=CARTESIAN_POINT('Ctrl Pts',(81.6580577336735,414.498146635717,47.7914675678002));
#41311=CARTESIAN_POINT('Ctrl Pts',(82.9929204080563,413.86167860706,55.8023046120247));
#41312=CARTESIAN_POINT('Ctrl Pts',(76.9710932722329,413.225210578403,61.2648397466391));
#41313=CARTESIAN_POINT('Ctrl Pts',(70.4453616288584,412.694820554522,59.4931309478417));
#41314=CARTESIAN_POINT('Ctrl Pts',(67.8902587970379,412.270508535417,55.2791970646377));
#41315=CARTESIAN_POINT('Ctrl Pts',(67.5436485600779,411.846196516313,50.3631536723669));
#41316=CARTESIAN_POINT('Ctrl Pts',(71.8458077986813,411.315806492433,45.1492552626692));
#41317=CARTESIAN_POINT('Ctrl Pts',(79.9217750170301,410.679338463775,46.1299912507797));
#41318=CARTESIAN_POINT('Ctrl Pts',(83.4481442408686,410.042870435119,53.4442313362922));
#41319=CARTESIAN_POINT('Ctrl Pts',(79.2123890848229,409.40640240646,60.3718808483404));
#41320=CARTESIAN_POINT('Ctrl Pts',(71.0787268288466,408.769934377806,60.5450429152035));
#41321=CARTESIAN_POINT('Ctrl Pts',(67.3164634352907,408.239544353923,54.9295989188625));
#41322=CARTESIAN_POINT('Ctrl Pts',(68.1492568471143,407.815232334819,50.0720529791814));
#41323=CARTESIAN_POINT('Ctrl Pts',(71.1118174108275,407.390920315714,46.1334689268072));
#41324=CARTESIAN_POINT('Ctrl Pts',(77.7783873168303,406.860530291834,45.0178340311155));
#41325=CARTESIAN_POINT('Ctrl Pts',(83.2328704840493,406.224062263176,51.0540330992533));
#41326=CARTESIAN_POINT('Ctrl Pts',(81.0989941768656,405.58759423452,58.8885473657906));
#41327=CARTESIAN_POINT('Ctrl Pts',(73.3584248002522,404.951126205863,61.3414323767353));
#41328=CARTESIAN_POINT('Ctrl Pts',(67.1039459981687,404.314658177206,56.1386839289719));
#41329=CARTESIAN_POINT('Ctrl Pts',(67.9456704139453,403.784268153325,49.432027003658));
#41330=CARTESIAN_POINT('Ctrl Pts',(71.7596457584586,403.359956134221,46.310674061179));
#41331=CARTESIAN_POINT('Ctrl Pts',(76.5790150618936,402.935644115116,45.2796888109111));
#41332=CARTESIAN_POINT('Ctrl Pts',(82.343807547953,402.405254091235,48.8088410945701));
#41333=CARTESIAN_POINT('Ctrl Pts',(82.5038263923615,401.768786062578,56.9428126458584));
#41334=CARTESIAN_POINT('Ctrl Pts',(75.7554457013352,401.132318033921,61.4586080859898));
#41335=CARTESIAN_POINT('Ctrl Pts',(68.3029116146995,400.495850005264,58.234823624498));
#41336=CARTESIAN_POINT('Ctrl Pts',(66.9923829061935,399.859381976607,50.205526415265));
#41337=CARTESIAN_POINT('Ctrl Pts',(72.0256241317357,399.328991952726,45.6939600829022));
#41338=CARTESIAN_POINT('Ctrl Pts',(76.951923377724,398.904679933622,45.8382763506332));
#41339=CARTESIAN_POINT('Ctrl Pts',(81.266580352052,398.480367914517,48.2200795820483));
#41340=CARTESIAN_POINT('Ctrl Pts',(83.3048203906889,397.949977890636,54.6647149918501));
#41341=CARTESIAN_POINT('Ctrl Pts',(78.0919630087754,397.313509861979,60.9107711141114));
#41342=CARTESIAN_POINT('Ctrl Pts',(70.035820603255,396.677041833323,59.8950841246337));
#41343=CARTESIAN_POINT('Ctrl Pts',(66.5231018692908,396.040573804665,52.5743015424564));
#41344=CARTESIAN_POINT('Ctrl Pts',(70.7986894391281,395.404105776009,45.6528529875597));
#41345=CARTESIAN_POINT('Ctrl Pts',(77.5571328712723,394.873715752128,45.5470683254055));
#41346=CARTESIAN_POINT('Ctrl Pts',(81.1818437693164,394.449403733023,48.8863380579642));
#41347=CARTESIAN_POINT('Ctrl Pts',(82.8775839616058,394.025091713919,53.5138337782664));
#41348=CARTESIAN_POINT('Ctrl Pts',(80.1905233291765,393.494701690038,59.7160473490804));
#41349=CARTESIAN_POINT('Ctrl Pts',(72.1591170084185,392.858233661381,61.0135879750886));
#41350=CARTESIAN_POINT('Ctrl Pts',(66.7427646843267,392.221765632724,54.9641104752807));
#41351=CARTESIAN_POINT('Ctrl Pts',(68.8911117968739,391.585297604067,47.1335514145627));
#41352=CARTESIAN_POINT('Ctrl Pts',(76.6577554419204,390.94882957541,44.7114973986289));
#41353=CARTESIAN_POINT('Ctrl Pts',(81.8297285544656,390.418439551529,49.0633294431198));
#41354=CARTESIAN_POINT('Ctrl Pts',(82.37672386321,389.994127532425,53.96129305807));
#41355=CARTESIAN_POINT('Ctrl Pts',(80.622625736186,389.569815513319,58.566984233337));
#41356=CARTESIAN_POINT('Ctrl Pts',(74.5269381549992,389.03942548944,61.4876589726595));
#41357=CARTESIAN_POINT('Ctrl Pts',(67.6124138739367,388.402957460782,57.2008824294));
#41358=CARTESIAN_POINT('Ctrl Pts',(67.4898925148396,387.766489432125,49.0818899404304));
#41359=CARTESIAN_POINT('Ctrl Pts',(74.2466041857144,387.130021403468,44.5785691750345));
#41360=CARTESIAN_POINT('Ctrl Pts',(81.6986080191094,386.493553374812,47.8427287961786));
#41361=CARTESIAN_POINT('Ctrl Pts',(82.749817016555,385.96316335093,54.5197571519698));
#41362=CARTESIAN_POINT('Ctrl Pts',(79.9510661822958,385.538851331826,58.5763869365196));
#41363=CARTESIAN_POINT('Ctrl Pts',(75.6066469653137,385.114539312722,60.9034608735224));
#41364=CARTESIAN_POINT('Ctrl Pts',(69.0892511374014,384.58414928884,59.1114509286099));
#41365=CARTESIAN_POINT('Ctrl Pts',(66.679761851001,383.947681260184,51.3409000765814));
#41366=CARTESIAN_POINT('Ctrl Pts',(71.9111075617697,383.311213231526,45.1307412562451));
#41367=CARTESIAN_POINT('Ctrl Pts',(79.9653598379443,382.67474520287,46.1613094447321));
#41368=CARTESIAN_POINT('Ctrl Pts',(83.4512031212773,382.038277174213,53.512227466944));
#41369=CARTESIAN_POINT('Ctrl Pts',(79.8665501131237,381.507887150332,59.2426734209241));
#41370=CARTESIAN_POINT('Ctrl Pts',(75.093455639325,381.083575131227,60.4701996264918));
#41371=CARTESIAN_POINT('Ctrl Pts',(70.2875034035968,380.659263112123,59.3783779610809));
#41372=CARTESIAN_POINT('Ctrl Pts',(66.5419572709727,380.128873088242,53.7517775497547));
#41373=CARTESIAN_POINT('Ctrl Pts',(69.8181652943605,379.492405059585,46.3050628276286));
#41374=CARTESIAN_POINT('Ctrl Pts',(77.8399913967625,378.855937030928,45.0467478820745));
#41375=CARTESIAN_POINT('Ctrl Pts',(83.2451586623123,378.219469002271,51.1062212379702));
#41376=CARTESIAN_POINT('Ctrl Pts',(81.056760009085,377.583000973614,58.9419094974527));
#41377=CARTESIAN_POINT('Ctrl Pts',(74.5927436622569,377.052610949733,60.9178246495513));
#41378=CARTESIAN_POINT('Ctrl Pts',(70.1841467313888,376.628298930629,58.7147530342143));
#41379=CARTESIAN_POINT('Ctrl Pts',(67.2716031340737,376.203986911524,54.7390340759755));
#41380=CARTESIAN_POINT('Ctrl Pts',(68.1332438336644,375.673596887643,48.0349067408809));
#41381=CARTESIAN_POINT('Ctrl Pts',(75.4897901509022,375.037128858987,44.5609571949648));
#41382=CARTESIAN_POINT('Ctrl Pts',(82.3713600232549,374.40066083033,48.8710670092633));
#41383=CARTESIAN_POINT('Ctrl Pts',(82.4788821316752,373.764192801672,56.990271989776));
#41384=CARTESIAN_POINT('Ctrl Pts',(75.6885682938352,373.127724773016,61.4712023785323));
#41385=CARTESIAN_POINT('Ctrl Pts',(69.5125903262564,372.597334749135,58.7243780003945));
#41386=CARTESIAN_POINT('Ctrl Pts',(67.6287264240034,372.17302273003,54.1702251440499));
#41387=CARTESIAN_POINT('Ctrl Pts',(68.0367530158591,371.748710710926,49.2587319147457));
#41388=CARTESIAN_POINT('Ctrl Pts',(73.0833721116578,371.218320687044,44.7621350101664));
#41389=CARTESIAN_POINT('Ctrl Pts',(80.9155106650358,370.581852658388,46.9632040336022));
#41390=CARTESIAN_POINT('Ctrl Pts',(83.2848191844876,369.945384629731,54.7297623227698));
#41391=CARTESIAN_POINT('Ctrl Pts',(78.0420097419556,369.308916601074,60.93024614814));
#41392=CARTESIAN_POINT('Ctrl Pts',(69.9770699095695,368.672448572417,59.8607394089223));
#41393=CARTESIAN_POINT('Ctrl Pts',(67.1153917312942,368.142058548536,53.7371337697309));
#41394=CARTESIAN_POINT('Ctrl Pts',(68.6793639935662,367.717746529432,49.0634583205791));
#41395=CARTESIAN_POINT('Ctrl Pts',(72.2080256168429,367.293434510327,45.6228481145867));
#41396=CARTESIAN_POINT('Ctrl Pts',(78.9667534352475,366.763044486446,45.5371375722202));
#41397=CARTESIAN_POINT('Ctrl Pts',(83.4366954912707,366.126576457789,52.3346898655854));
#41398=CARTESIAN_POINT('Ctrl Pts',(80.1327691280308,365.490108429132,59.7520425675722));
#41399=CARTESIAN_POINT('Ctrl Pts',(72.1086321011238,364.853640400476,60.995535829637));
#41400=CARTESIAN_POINT('Ctrl Pts',(66.7209288483918,364.217172371818,54.8996558418304));
#41401=CARTESIAN_POINT('Ctrl Pts',(68.5757876895998,363.686782347938,48.3998676376236));
#41402=CARTESIAN_POINT('Ctrl Pts',(72.8212415522201,363.262470328833,45.8967949376159));
#41403=CARTESIAN_POINT('Ctrl Pts',(77.7414756105612,362.838158309728,45.6129846976599));
#41404=CARTESIAN_POINT('Ctrl Pts',(82.900500275741,362.307768285847,49.9801591302214));
#41405=CARTESIAN_POINT('Ctrl Pts',(81.8179509175015,361.671300257191,58.0433586224958));
#41406=CARTESIAN_POINT('Ctrl Pts',(74.459730818579,361.034832228533,61.4769642339771));
#41407=CARTESIAN_POINT('Ctrl Pts',(67.5861351940375,360.398364199877,57.1541487498666));
#41408=CARTESIAN_POINT('Ctrl Pts',(67.5156712101143,359.761896171219,49.0189084957493));
#41409=CARTESIAN_POINT('Ctrl Pts',(73.1781765660606,359.231506147339,45.327867841106));
#41410=CARTESIAN_POINT('Ctrl Pts',(78.02481749753,358.807194128234,46.221916566047));
#41411=CARTESIAN_POINT('Ctrl Pts',(81.9256836447492,358.38288210913,49.2339747896943));
#41412=CARTESIAN_POINT('Ctrl Pts',(82.9570561679429,357.852492085249,55.9140959516758));
#41413=CARTESIAN_POINT('Ctrl Pts',(76.8524702261602,357.216024056593,61.2919328443892));
#41414=CARTESIAN_POINT('Ctrl Pts',(69.045522611019,356.579556027934,59.059306710478));
#41415=CARTESIAN_POINT('Ctrl Pts',(66.6905660886839,355.943087999279,51.2883846096399));
#41416=CARTESIAN_POINT('Ctrl Pts',(71.9718690931407,355.30661997062,45.1000942366571));
#41417=CARTESIAN_POINT('Ctrl Pts',(78.6673638110826,354.776229946742,46.0264303000629));
#41418=CARTESIAN_POINT('Ctrl Pts',(81.7403124811487,354.351917927635,49.879511912526));
#41419=CARTESIAN_POINT('Ctrl Pts',(82.710365963219,353.927605908532,54.7115143631759));
#41420=CARTESIAN_POINT('Ctrl Pts',(79.1087084297517,353.39721588465,60.4312880503046));
#41421=CARTESIAN_POINT('Ctrl Pts',(70.9733648495515,352.760747855993,60.4885942221618));
#41422=CARTESIAN_POINT('Ctrl Pts',(66.5431347605869,352.124279827337,53.6837347909748));
#41423=CARTESIAN_POINT('Ctrl Pts',(69.86075831682,351.487811798679,46.2724984259334));
#41424=CARTESIAN_POINT('Ctrl Pts',(77.9059622970041,350.851343770022,45.063452486993));
#41425=CARTESIAN_POINT('Ctrl Pts',(82.3536190500792,350.320953746142,50.1532557668041));
#41426=CARTESIAN_POINT('Ctrl Pts',(82.1471145858705,349.896641727037,55.077340183975));
#41427=CARTESIAN_POINT('Ctrl Pts',(79.7110241380284,349.472329707933,59.3615804633122));
#41428=CARTESIAN_POINT('Ctrl Pts',(73.241167520903,348.941939684051,61.3182877419281));
#41429=CARTESIAN_POINT('Ctrl Pts',(67.0614270800493,348.305471655395,56.0269828698838));
#41430=CARTESIAN_POINT('Ctrl Pts',(68.178750363224,347.669003626737,47.9843067480785));
#41431=CARTESIAN_POINT('Ctrl Pts',(75.5433011550229,347.032535598082,44.5643005851607));
#41432=CARTESIAN_POINT('Ctrl Pts',(82.4102142072295,346.396067569423,48.9269378951685));
#41433=CARTESIAN_POINT('Ctrl Pts',(82.4306579931864,345.865677545544,55.6861782424242));
#41434=CARTESIAN_POINT('Ctrl Pts',(79.0458886590258,345.441365526438,59.2684384222114));
#41435=CARTESIAN_POINT('Ctrl Pts',(74.3973513042222,345.017053507334,60.9056164522856));
#41436=CARTESIAN_POINT('Ctrl Pts',(68.2295590842627,344.486663483453,58.1404605522035));
#41437=CARTESIAN_POINT('Ctrl Pts',(67.0335268243352,343.850195454796,50.0933116161857));
#41438=CARTESIAN_POINT('Ctrl Pts',(73.1509092443753,343.213727426139,44.753772043679));
#41439=CARTESIAN_POINT('Ctrl Pts',(80.9537189797542,342.577259397483,47.0008169370583));
#41440=CARTESIAN_POINT('Ctrl Pts',(83.2775178994342,341.940791368825,54.7974224642177));
#41441=CARTESIAN_POINT('Ctrl Pts',(78.8607311565456,341.410401344945,59.9140368612769));
#41442=CARTESIAN_POINT('Ctrl Pts',(73.9562515767661,340.98608932584,60.3991466351328));
#41443=CARTESIAN_POINT('Ctrl Pts',(69.3730748596339,340.561777306736,58.5870366437974));
#41444=CARTESIAN_POINT('Ctrl Pts',(66.529597387875,340.031387282854,52.4549583755465));
#41445=CARTESIAN_POINT('Ctrl Pts',(70.9033353532007,339.394919254198,45.5951103177607));
#41446=CARTESIAN_POINT('Ctrl Pts',(79.0232276239048,338.75845122554,45.575109529237));
#41447=CARTESIAN_POINT('Ctrl Pts',(83.4408788431293,338.121983196884,52.3881417634678));
#41448=CARTESIAN_POINT('Ctrl Pts',(80.0828900417,337.485515168226,59.7983381424253));
#41449=CARTESIAN_POINT('Ctrl Pts',(73.3931213062477,336.955125144346,60.7651588530632));
#41450=CARTESIAN_POINT('Ctrl Pts',(69.3721520503855,336.530813125241,57.9154119020912));
#41451=CARTESIAN_POINT('Ctrl Pts',(67.1001164622618,336.106501106137,53.5419572347303));
#41452=CARTESIAN_POINT('Ctrl Pts',(68.9742725277789,335.576111082256,47.0477069267705));
#41453=CARTESIAN_POINT('Ctrl Pts',(76.7746263075684,334.939643053599,44.7365210676572));
#41454=CARTESIAN_POINT('Ctrl Pts',(82.9182388733991,334.303175024942,50.0458595537917));
#41455=CARTESIAN_POINT('Ctrl Pts',(81.7860594422747,333.666706996285,58.0864578061059));
#41456=CARTESIAN_POINT('Ctrl Pts',(74.3917149433775,333.030238967628,61.4792101691393));
#41457=CARTESIAN_POINT('Ctrl Pts',(68.7069857809447,332.499848943747,57.8224900034527));
#41458=CARTESIAN_POINT('Ctrl Pts',(67.5398227525649,332.075536924643,53.0342771942362));
#41459=CARTESIAN_POINT('Ctrl Pts',(68.6922375796396,331.651224905538,48.2424934441593));
#41460=CARTESIAN_POINT('Ctrl Pts',(74.3656809371467,331.120834881658,44.5682876130294));
#41461=CARTESIAN_POINT('Ctrl Pts',(81.7704365027121,330.484366853,47.9382570757208));
#41462=CARTESIAN_POINT('Ctrl Pts',(82.9273671692477,329.847898824343,55.9753312916411));
#41463=CARTESIAN_POINT('Ctrl Pts',(76.8001309130144,329.211430795687,61.3035604890083));
#41464=CARTESIAN_POINT('Ctrl Pts',(68.9926980804786,328.574962767029,59.0164024860079));
#41465=CARTESIAN_POINT('Ctrl Pts',(67.0985554248778,328.044572743149,52.5279533939223));
#41466=CARTESIAN_POINT('Ctrl Pts',(69.3571145943043,327.620260724044,48.1475239721236));
#41467=CARTESIAN_POINT('Ctrl Pts',(73.3692905618005,327.19594870494,45.2854101646361));
#41468=CARTESIAN_POINT('Ctrl Pts',(80.0620043807514,326.665558681058,46.2316288275121));
#41469=CARTESIAN_POINT('Ctrl Pts',(83.4427928913044,326.029090652402,53.6314510018721));
#41470=CARTESIAN_POINT('Ctrl Pts',(79.0461395988837,325.392622623745,60.4580526707575));
#41471=CARTESIAN_POINT('Ctrl Pts',(70.9262242348619,324.756154595088,60.4630527212918));
#41472=CARTESIAN_POINT('Ctrl Pts',(66.5313858701374,324.119686566431,53.6167037005958));
#41473=CARTESIAN_POINT('Ctrl Pts',(69.3559695000191,323.58929654255,47.4758995726207));
#41474=CARTESIAN_POINT('Ctrl Pts',(73.9335450964997,323.164984523445,45.6496867975949));
#41475=CARTESIAN_POINT('Ctrl Pts',(78.8394950580058,322.740672504341,46.1196936234625));
#41476=CARTESIAN_POINT('Ctrl Pts',(83.2720146665453,322.21028248046,51.2226847012778));
#41477=CARTESIAN_POINT('Ctrl Pts',(80.9722321220802,321.573814451804,59.0264081339356));
#41478=CARTESIAN_POINT('Ctrl Pts',(73.1763779112654,320.937346423146,61.2974668392768));
#41479=CARTESIAN_POINT('Ctrl Pts',(67.042584310839,320.300878394489,55.9767876921426));
#41480=CARTESIAN_POINT('Ctrl Pts',(68.2138341304525,319.664410365832,47.9259943756242));
#41481=CARTESIAN_POINT('Ctrl Pts',(74.3730833377875,319.134020341951,45.1418612569866));
#41482=CARTESIAN_POINT('Ctrl Pts',(79.0266394483123,318.709708322847,46.7647189116685));
#41483=CARTESIAN_POINT('Ctrl Pts',(82.4224223395787,318.285396303742,50.336540575266));
#41484=CARTESIAN_POINT('Ctrl Pts',(82.4227900152136,317.755006279862,57.0958118292673));
#41485=CARTESIAN_POINT('Ctrl Pts',(75.5693418552194,317.118538251204,61.4795713440574));
#41486=CARTESIAN_POINT('Ctrl Pts',(68.1942959424373,316.482070222548,58.0822564773221));
#41487=CARTESIAN_POINT('Ctrl Pts',(67.0522149557767,315.845602193891,50.0430586604197));
#41488=CARTESIAN_POINT('Ctrl Pts',(73.2156344403881,315.209134165234,44.7327517557342));
#41489=CARTESIAN_POINT('Ctrl Pts',(79.6914849948774,314.678744141353,46.6695293930162));
#41490=CARTESIAN_POINT('Ctrl Pts',(82.1407548583383,314.254432122248,50.9462487638779));
#41491=CARTESIAN_POINT('Ctrl Pts',(82.3624193546182,313.830120103144,55.8696740240246));
#41492=CARTESIAN_POINT('Ctrl Pts',(77.9304549343695,313.299730079263,60.9731472921046));
#41493=CARTESIAN_POINT('Ctrl Pts',(69.8815664959961,312.663262050606,59.7888778667402));
#41494=CARTESIAN_POINT('Ctrl Pts',(66.5411398372432,312.026794021949,52.3878914286447));
#41495=CARTESIAN_POINT('Ctrl Pts',(70.9503971034345,311.390325993292,45.5694237943499));
#41496=CARTESIAN_POINT('Ctrl Pts',(79.0858785651323,310.753857964635,45.6016813765094));
#41497=CARTESIAN_POINT('Ctrl Pts',(82.7051299253863,310.223467940754,51.310338627707));
#41498=CARTESIAN_POINT('Ctrl Pts',(81.7499585364533,309.79915592165,56.1453049211703));
#41499=CARTESIAN_POINT('Ctrl Pts',(78.6888878786527,309.374843902545,60.0078297261541));
#41500=CARTESIAN_POINT('Ctrl Pts',(71.9962770398569,308.844453878664,60.9547764938151));
#41501=CARTESIAN_POINT('Ctrl Pts',(66.6959456305342,308.207985850007,54.7827763223478));
#41502=CARTESIAN_POINT('Ctrl Pts',(69.0269647079598,307.57151782135,47.0046402615646));
#41503=CARTESIAN_POINT('Ctrl Pts',(76.8270011735663,306.935049792693,44.7479875070206));
#41504=CARTESIAN_POINT('Ctrl Pts',(82.9481162719336,306.298581764036,50.1070031925532));
#41505=CARTESIAN_POINT('Ctrl Pts',(81.9373163980776,305.768191740156,56.7902682355812));
#41506=CARTESIAN_POINT('Ctrl Pts',(78.0457427182703,305.343879721051,59.8143227548971));
#41507=CARTESIAN_POINT('Ctrl Pts',(73.2018774913111,304.919567701947,60.7232898083249));
#41508=CARTESIAN_POINT('Ctrl Pts',(67.5280344450094,304.389177678065,57.049701221359));
#41509=CARTESIAN_POINT('Ctrl Pts',(67.5734500950031,303.752709649409,48.9142825730056));
#41510=CARTESIAN_POINT('Ctrl Pts',(74.4337034050772,303.116241620751,44.5703241200507));
#41511=CARTESIAN_POINT('Ctrl Pts',(81.8024605270155,302.479773592095,47.9812578627763));
#41512=CARTESIAN_POINT('Ctrl Pts',(82.9098309440052,301.843305563437,56.0410860200523));
#41513=CARTESIAN_POINT('Ctrl Pts',(77.7642770452582,301.312915539558,60.424124132531));
#41514=CARTESIAN_POINT('Ctrl Pts',(72.8431924711145,300.888603520452,60.1554643936637));
#41515=CARTESIAN_POINT('Ctrl Pts',(68.5900518955643,300.464291501348,57.6654750993555));
#41516=CARTESIAN_POINT('Ctrl Pts',(66.7151893218969,299.933901477467,51.1714287220792));
#41517=CARTESIAN_POINT('Ctrl Pts',(72.0840981258804,299.29743344881,45.0589891583906));
#41518=CARTESIAN_POINT('Ctrl Pts',(80.1120257724278,298.660965420153,46.2777706077001));
#41519=CARTESIAN_POINT('Ctrl Pts',(83.4387741350087,298.024497391496,53.6849155267259));
#41520=CARTESIAN_POINT('Ctrl Pts',(78.9897825916792,297.388029362839,60.4961983290048));
#41521=CARTESIAN_POINT('Ctrl Pts',(72.230822911004,296.857639338958,60.4312979795421));
#41522=CARTESIAN_POINT('Ctrl Pts',(68.6915845458889,296.433327319854,57.0015686555198));
#41523=CARTESIAN_POINT('Ctrl Pts',(67.1132296826662,296.009015300749,52.3327307522611));
#41524=CARTESIAN_POINT('Ctrl Pts',(69.956040019597,295.478625276869,46.2003431741158));
#41525=CARTESIAN_POINT('Ctrl Pts',(78.0176486663101,294.842157248211,45.1060099559052));
#41526=CARTESIAN_POINT('Ctrl Pts',(83.2795242391994,294.205689219555,51.2903220417248));
#41527=CARTESIAN_POINT('Ctrl Pts',(80.9341397967266,293.569221190898,59.064138500607));
#41528=CARTESIAN_POINT('Ctrl Pts',(73.1088153495147,292.93275316224,61.2893118559007));
#41529=CARTESIAN_POINT('Ctrl Pts',(68.0483753764643,292.40236313836,56.8082745541695));
#41530=CARTESIAN_POINT('Ctrl Pts',(67.6252284753894,291.978051119255,51.8980608988107));
#41531=CARTESIAN_POINT('Ctrl Pts',(69.4950614381384,291.553739100151,47.3381293058391));
#41532=CARTESIAN_POINT('Ctrl Pts',(75.6625527961363,291.02334907627,44.5723024187452));
#41533=CARTESIAN_POINT('Ctrl Pts',(82.46663100973,290.386881047613,49.0323045295677));
#41534=CARTESIAN_POINT('Ctrl Pts',(82.3841080390843,289.750413018956,57.1518020804449));
#41535=CARTESIAN_POINT('Ctrl Pts',(75.5158413988719,289.113944990299,61.4830794761245));
#41536=CARTESIAN_POINT('Ctrl Pts',(68.1486338337177,288.477476961643,58.0317968367027));
#41537=CARTESIAN_POINT('Ctrl Pts',(67.2663555438189,287.947086937761,51.3303542278666));
#41538=CARTESIAN_POINT('Ctrl Pts',(70.1666442948999,287.522774918657,47.3456865376424));
#41539=CARTESIAN_POINT('Ctrl Pts',(74.5684371812347,287.098462899552,45.1290515142399));
#41540=CARTESIAN_POINT('Ctrl Pts',(81.0385066331955,286.568072875671,47.0850549158614));
#41541=CARTESIAN_POINT('Ctrl Pts',(83.2510206077065,285.931604847015,54.9139680637917));
#41542=CARTESIAN_POINT('Ctrl Pts',(77.8645357794759,285.295136818357,60.9900549389625));
#41543=CARTESIAN_POINT('Ctrl Pts',(69.8388734112542,284.658668789701,59.7564447611965));
#41544=CARTESIAN_POINT('Ctrl Pts',(66.5397528529418,284.022200761043,52.3198526178177));
#41545=CARTESIAN_POINT('Ctrl Pts',(70.2679572090717,283.491810737163,46.6817465262931));
#41546=CARTESIAN_POINT('Ctrl Pts',(75.0705250001109,283.067498718058,45.5751327483045));
#41547=CARTESIAN_POINT('Ctrl Pts',(79.8473763416493,282.643186698953,46.7879570150492));
#41548=CARTESIAN_POINT('Ctrl Pts',(83.4496561165695,282.112796675073,52.5073388385993));
#41549=CARTESIAN_POINT('Ctrl Pts',(79.9864624668663,281.476328646416,59.8689547556312));
#41550=CARTESIAN_POINT('Ctrl Pts',(71.9354214358458,280.839860617759,60.9243167012247));
#41551=CARTESIAN_POINT('Ctrl Pts',(66.6849797515537,280.203392589102,54.7302943700388));
#41552=CARTESIAN_POINT('Ctrl Pts',(69.0705324776169,279.566924560445,46.9523616526382));
#41553=CARTESIAN_POINT('Ctrl Pts',(75.5823799037634,279.036534536564,45.1402934643665));
#41554=CARTESIAN_POINT('Ctrl Pts',(79.9339434731479,278.61222251746,47.4539801204988));
#41555=CARTESIAN_POINT('Ctrl Pts',(82.7451712026369,278.187910498354,51.501973462158));
#41556=CARTESIAN_POINT('Ctrl Pts',(81.7145254259567,277.657520474474,58.1822067891732));
#41557=CARTESIAN_POINT('Ctrl Pts',(74.2726070999485,277.021052445817,61.4692952872608));
#41558=CARTESIAN_POINT('Ctrl Pts',(67.5020619551909,276.38458441716,56.9867994465287));
#41559=CARTESIAN_POINT('Ctrl Pts',(67.5995847596681,275.748116388503,48.8674682042408));
#41560=CARTESIAN_POINT('Ctrl Pts',(74.5008774943678,275.111648359846,44.5594225040166));
#41561=CARTESIAN_POINT('Ctrl Pts',(80.6055287943158,274.581258335966,47.4613150806631));
#41562=CARTESIAN_POINT('Ctrl Pts',(82.3737993009008,274.156946316861,52.061583644204));
#41563=CARTESIAN_POINT('Ctrl Pts',(81.84188717115,273.732634297756,56.9612082142489));
#41564=CARTESIAN_POINT('Ctrl Pts',(76.683337647963,273.202244273875,61.3289438790048));
#41565=CARTESIAN_POINT('Ctrl Pts',(68.9092734328478,272.565776245219,58.930814452869));
#41566=CARTESIAN_POINT('Ctrl Pts',(66.736826601721,271.929308216562,51.1069071626902));
#41567=CARTESIAN_POINT('Ctrl Pts',(72.1345272122206,271.292840187904,45.0407816579883));
#41568=CARTESIAN_POINT('Ctrl Pts',(80.169890527306,270.656372159248,46.3135878332638));
#41569=CARTESIAN_POINT('Ctrl Pts',(82.8760347300884,270.125982135366,52.5074986797403));
#41570=CARTESIAN_POINT('Ctrl Pts',(81.1945504046273,269.701670116263,57.1401935654835));
#41571=CARTESIAN_POINT('Ctrl Pts',(77.5801381329828,269.277358097157,60.4906077744654));
#41572=CARTESIAN_POINT('Ctrl Pts',(70.8214010299961,268.746968073278,60.4056325247524));
#41573=CARTESIAN_POINT('Ctrl Pts',(66.5245229306788,268.110500044619,53.4973810987512));
#41574=CARTESIAN_POINT('Ctrl Pts',(70.0146846891176,267.474032015963,46.1658177307299));
#41575=CARTESIAN_POINT('Ctrl Pts',(78.0676616590457,266.837563987306,45.1253310940095));
#41576=CARTESIAN_POINT('Ctrl Pts',(83.2997256280266,266.201095958649,51.3553074815834));
#41577=CARTESIAN_POINT('Ctrl Pts',(81.2813379625202,265.670705934768,57.8061879836611));
#41578=CARTESIAN_POINT('Ctrl Pts',(76.9740348929436,265.246393915664,60.2012645394267));
#41579=CARTESIAN_POINT('Ctrl Pts',(72.0482033406272,264.822081896559,60.3607479535025));
#41580=CARTESIAN_POINT('Ctrl Pts',(67.0010950831651,264.291691872678,55.8647001048012));
#41581=CARTESIAN_POINT('Ctrl Pts',(68.2868957752895,263.655223844021,47.8314059022108));
#41582=CARTESIAN_POINT('Ctrl Pts',(75.7294686614734,263.018755815364,44.5846907386619));
#41583=CARTESIAN_POINT('Ctrl Pts',(82.491721281617,262.382287786707,49.0796868477532));
#41584=CARTESIAN_POINT('Ctrl Pts',(82.3567472759911,261.74581975805,57.2141125301874));
#41585=CARTESIAN_POINT('Ctrl Pts',(76.6028482236023,261.21542973417,60.7609976023698));
#41586=CARTESIAN_POINT('Ctrl Pts',(71.7803273753439,260.791117715065,59.744855826201));
#41587=CARTESIAN_POINT('Ctrl Pts',(67.9567596897789,260.366805695961,56.6352607408135));
#41588=CARTESIAN_POINT('Ctrl Pts',(67.0943896432094,259.836415672079,49.9312271845779));
#41589=CARTESIAN_POINT('Ctrl Pts',(73.3328200825553,259.199947643423,44.7092462559759));
#41590=CARTESIAN_POINT('Ctrl Pts',(81.0809045713872,258.563479614766,47.1382866577201));
#41591=CARTESIAN_POINT('Ctrl Pts',(83.2388937946819,257.927011586109,54.9661939790624));
#41592=CARTESIAN_POINT('Ctrl Pts',(77.8030197810562,257.290543557452,61.0191579532844));
#41593=CARTESIAN_POINT('Ctrl Pts',(71.1330498823766,256.760153533571,59.9240554142214));
#41594=CARTESIAN_POINT('Ctrl Pts',(68.1583716191361,256.335841514467,55.9946100753261));
#41595=CARTESIAN_POINT('Ctrl Pts',(67.3106359050502,255.911529495361,51.1396542979552));
#41596=CARTESIAN_POINT('Ctrl Pts',(71.0555698892031,255.381139471481,45.5126464363393));
#41597=CARTESIAN_POINT('Ctrl Pts',(79.1897666288785,254.744671442824,45.6607766678622));
#41598=CARTESIAN_POINT('Ctrl Pts',(83.4467609168083,254.108203414167,52.5753301713011));
#41599=CARTESIAN_POINT('Ctrl Pts',(79.94306077055,253.47173538551,59.9004332971613));
#41600=CARTESIAN_POINT('Ctrl Pts',(71.8698933621133,252.835267356853,60.905951651344));
#41601=CARTESIAN_POINT('Ctrl Pts',(67.5521726494623,252.304877332973,55.7054674558198));
#41602=CARTESIAN_POINT('Ctrl Pts',(67.8829448323149,251.880565313867,50.7881672611792));
#41603=CARTESIAN_POINT('Ctrl Pts',(70.4264360103071,251.456253294763,46.5668044399285));
#41604=CARTESIAN_POINT('Ctrl Pts',(76.9436368441984,250.925863270882,44.7740854683437));
#41605=CARTESIAN_POINT('Ctrl Pts',(82.9878010642769,250.289395242225,50.2197422740896));
#41606=CARTESIAN_POINT('Ctrl Pts',(81.6677557512237,249.652927213568,58.2316416051388));
#41607=CARTESIAN_POINT('Ctrl Pts',(74.2191975778626,249.016459184912,61.4646018055494));
#41608=CARTESIAN_POINT('Ctrl Pts',(67.4646309039848,248.379991156254,56.9299653026552));
#41609=CARTESIAN_POINT('Ctrl Pts',(67.6148650422271,247.849601132374,50.1723638254997));
#41610=CARTESIAN_POINT('Ctrl Pts',(71.0890075766938,247.425289113269,46.6767115127872));
#41611=CARTESIAN_POINT('Ctrl Pts',(75.7774017059763,247.000977094165,45.1574314432569));
#41612=CARTESIAN_POINT('Ctrl Pts',(81.87340699568,246.470587070284,48.0774430062916));
#41613=CARTESIAN_POINT('Ctrl Pts',(82.8658667097527,245.834119041627,56.1522261539176));
#41614=CARTESIAN_POINT('Ctrl Pts',(76.6156108827676,245.19765101297,61.3355988606232));
#41615=CARTESIAN_POINT('Ctrl Pts',(68.8720270293296,244.561182984313,58.8922487784292));
#41616=CARTESIAN_POINT('Ctrl Pts',(66.7458339833244,243.924714955656,51.039452951696));
#41617=CARTESIAN_POINT('Ctrl Pts',(71.2904074612936,243.394324931775,46.0359941556539));
#41618=CARTESIAN_POINT('Ctrl Pts',(76.2055723888366,242.970012912671,45.6748775869161));
#41619=CARTESIAN_POINT('Ctrl Pts',(80.7415318974397,242.545700893566,47.6021354257825));
#41620=CARTESIAN_POINT('Ctrl Pts',(83.4292672620948,242.015310869685,53.8040566305332));
#41621=CARTESIAN_POINT('Ctrl Pts',(78.8837120348752,241.378842841028,60.5512802700413));
#41622=CARTESIAN_POINT('Ctrl Pts',(70.7659036424594,240.742374812371,60.3662466963265));
#41623=CARTESIAN_POINT('Ctrl Pts',(66.5216905776815,240.105906783714,53.4438406131678));
#41624=CARTESIAN_POINT('Ctrl Pts',(70.0657168395739,239.469438755057,46.1207963677559));
#41625=CARTESIAN_POINT('Ctrl Pts',(76.7777649544276,238.939048731177,45.3232011544806));
#41626=CARTESIAN_POINT('Ctrl Pts',(80.7254958293852,238.514736712072,48.273569331517));
#41627=CARTESIAN_POINT('Ctrl Pts',(82.8863769043757,238.090424692968,52.702998687643));
#41628=CARTESIAN_POINT('Ctrl Pts',(80.8488379995376,237.560034669086,59.1478558025543));
#41629=CARTESIAN_POINT('Ctrl Pts',(72.9926135961208,236.92356664043,61.261345165764));
#41630=CARTESIAN_POINT('Ctrl Pts',(66.9850210825831,236.287098611772,55.7985727276454));
#41631=CARTESIAN_POINT('Ctrl Pts',(68.3198653405516,235.650630583116,47.7891257226176));
#41632=CARTESIAN_POINT('Ctrl Pts',(75.7975195609413,235.014162554458,44.5841629263389));
#41633=CARTESIAN_POINT('Ctrl Pts',(81.3881037350091,234.483772530579,48.3832571095637));
#41634=CARTESIAN_POINT('Ctrl Pts',(82.433991842377,234.059460511473,53.1994142403088));
#41635=CARTESIAN_POINT('Ctrl Pts',(81.1609514886376,233.635148492369,57.9605716309985));
#41636=CARTESIAN_POINT('Ctrl Pts',(75.3965430028564,233.104758468487,61.4903510616958));
#41637=CARTESIAN_POINT('Ctrl Pts',(68.0792403488523,232.468290439831,57.9344853393984));
#41638=CARTESIAN_POINT('Ctrl Pts',(67.1256153736941,231.831822411174,49.8707610183333));
#41639=CARTESIAN_POINT('Ctrl Pts',(73.3854363071609,231.195354382517,44.698943890854));
#41640=CARTESIAN_POINT('Ctrl Pts',(81.1326289242826,230.55888635386,47.182511026836));
#41641=CARTESIAN_POINT('Ctrl Pts',(82.8623337589318,230.028496329979,53.7167186456097));
#41642=CARTESIAN_POINT('Ctrl Pts',(80.4938884721818,229.604184310875,58.0387226211197));
#41643=CARTESIAN_POINT('Ctrl Pts',(76.4107231014128,229.17987229177,60.7986160968965));
#41644=CARTESIAN_POINT('Ctrl Pts',(69.7440352528211,228.649482267889,59.6837075155094));
#41645=CARTESIAN_POINT('Ctrl Pts',(66.5511708056287,228.013014239233,52.2008794545322));
#41646=CARTESIAN_POINT('Ctrl Pts',(71.1187945807649,227.376546210575,45.4874702176766));
#41647=CARTESIAN_POINT('Ctrl Pts',(79.2362472869139,226.740078181919,45.687500330039));
#41648=CARTESIAN_POINT('Ctrl Pts',(83.4568135234188,226.103610153261,52.6426365499872));
#41649=CARTESIAN_POINT('Ctrl Pts',(80.4780746217014,225.573220129381,58.7101617981617));
#41650=CARTESIAN_POINT('Ctrl Pts',(75.8558464940669,225.148908110276,60.4202081308665));
#41651=CARTESIAN_POINT('Ctrl Pts',(70.9633284069712,224.724596091172,59.8264754996315));
#41652=CARTESIAN_POINT('Ctrl Pts',(66.6610730582673,224.194206067291,54.6131899181505));
#41653=CARTESIAN_POINT('Ctrl Pts',(69.157166952132,223.557738038634,46.8700243015665));
#41654=CARTESIAN_POINT('Ctrl Pts',(77.0078801768239,222.921270009977,44.7965356614796));
#41655=CARTESIAN_POINT('Ctrl Pts',(83.005370185439,222.28480198132,50.2703972566507));
#41656=CARTESIAN_POINT('Ctrl Pts',(81.6312111896099,221.648333952663,58.289049463463));
#41657=CARTESIAN_POINT('Ctrl Pts',(75.403625026532,221.117943928782,60.9167734757233));
#41658=CARTESIAN_POINT('Ctrl Pts',(70.7925316075469,220.693631909677,59.1769303273695));
#41659=CARTESIAN_POINT('Ctrl Pts',(67.4880169134195,220.269319890573,55.5205041023283));
#41660=CARTESIAN_POINT('Ctrl Pts',(67.658328852938,219.738929866692,48.7633776943335));
#41661=CARTESIAN_POINT('Ctrl Pts',(74.6202688954666,219.102461838035,44.5540677770521));
#41662=CARTESIAN_POINT('Ctrl Pts',(81.9072044880662,218.465993809378,48.1365169238422));
#41663=CARTESIAN_POINT('Ctrl Pts',(82.8458867743987,217.829525780721,56.2019949911516));
#41664=CARTESIAN_POINT('Ctrl Pts',(76.5504328451881,217.193057752064,61.3549706278894));
#41665=CARTESIAN_POINT('Ctrl Pts',(70.1253934407355,216.662667728183,59.2553153217915));
#41666=CARTESIAN_POINT('Ctrl Pts',(67.7851257368055,216.238355709079,54.9180846330423));
#41667=CARTESIAN_POINT('Ctrl Pts',(67.6873898951343,215.814043689974,49.9906921806011));
#41668=CARTESIAN_POINT('Ctrl Pts',(72.2478204552385,215.283653666094,45.0006205160765));
#41669=CARTESIAN_POINT('Ctrl Pts',(80.2623903861754,214.647185637436,46.3879895849169));
#41670=CARTESIAN_POINT('Ctrl Pts',(83.4181495289489,214.01071760878,53.8705343916804));
#41671=CARTESIAN_POINT('Ctrl Pts',(78.8320462675723,213.374249580122,60.576285830569));
#41672=CARTESIAN_POINT('Ctrl Pts',(70.7115626079727,212.737781551466,60.3371402298481));
#41673=CARTESIAN_POINT('Ctrl Pts',(66.51967771935,212.101313522809,53.3818980605949));
#41674=CARTESIAN_POINT('Ctrl Pts',(70.1151634260747,211.464845494152,46.0859672328122));
#41675=CARTESIAN_POINT('Ctrl Pts',(76.8334970750981,210.934455470271,45.3360771801855));
#41676=CARTESIAN_POINT('Ctrl Pts',(80.7595195459134,210.510143451166,48.3151871536133));
#41677=CARTESIAN_POINT('Ctrl Pts',(82.888548276625,210.085831432062,52.7599210756032));
#41678=CARTESIAN_POINT('Ctrl Pts',(80.8044533787177,209.555441408181,59.1900246680587));
#41679=CARTESIAN_POINT('Ctrl Pts',(72.9332444349171,208.918973379524,61.2467132323923));
#41680=CARTESIAN_POINT('Ctrl Pts',(66.9651916338919,208.282505350867,55.7407703836971));
#41681=CARTESIAN_POINT('Ctrl Pts',(68.3578058098086,207.64603732221,47.7411455189258));
#41682=CARTESIAN_POINT('Ctrl Pts',(75.858380007233,207.009569293553,44.5902272647635));
#41683=CARTESIAN_POINT('Ctrl Pts',(81.4214132232327,206.479179269672,48.4295533629287));
#41684=CARTESIAN_POINT('Ctrl Pts',(82.4325231697244,206.054867250568,53.2531336492902));
#41685=CARTESIAN_POINT('Ctrl Pts',(81.1251652983051,205.630555231463,58.0049808791072));
#41686=CARTESIAN_POINT('Ctrl Pts',(75.3354386547323,205.100165207582,61.4930789706004));
#41687=CARTESIAN_POINT('Ctrl Pts',(68.0439825137209,204.463697178926,57.8845109023309));
#41688=CARTESIAN_POINT('Ctrl Pts',(67.1485620295659,203.827229150268,49.8141162822962));
#41689=CARTESIAN_POINT('Ctrl Pts',(73.4455348837261,203.190761121612,44.6875983460268));
#41690=CARTESIAN_POINT('Ctrl Pts',(81.1746068125109,202.554293092954,47.2269970174668));
#41691=CARTESIAN_POINT('Ctrl Pts',(82.8571222576213,202.023903069074,53.773514367668));
#41692=CARTESIAN_POINT('Ctrl Pts',(80.457555279028,201.599591049969,58.0783174973361));
#41693=CARTESIAN_POINT('Ctrl Pts',(76.3545835235771,201.175279030865,60.8086790297828));
#41694=CARTESIAN_POINT('Ctrl Pts',(69.6961132750877,200.644889006984,59.6456992226426));
#41695=CARTESIAN_POINT('Ctrl Pts',(66.5573206522378,200.008420978327,52.1400293614303));
#41696=CARTESIAN_POINT('Ctrl Pts',(71.1732628826331,199.37195294967,45.4597503397074));
#41697=CARTESIAN_POINT('Ctrl Pts',(79.2890610861173,198.735484921013,45.7183427854784));
#41698=CARTESIAN_POINT('Ctrl Pts',(83.4593360519497,198.099016892356,52.7037494220058));
#41699=CARTESIAN_POINT('Ctrl Pts',(80.4368974067114,197.568626868475,58.7496250948249));
#41700=CARTESIAN_POINT('Ctrl Pts',(75.8024515672505,197.144314849371,60.4262774749522));
#41701=CARTESIAN_POINT('Ctrl Pts',(70.9143446388831,196.720002830266,59.7972607045105));
#41702=CARTESIAN_POINT('Ctrl Pts',(66.649815151398,196.189612806385,54.553069988049));
#41703=CARTESIAN_POINT('Ctrl Pts',(69.2017112256344,195.553144777728,46.8281152573069));
#41704=CARTESIAN_POINT('Ctrl Pts',(77.0671801888051,194.916676749071,44.8113236199402));
#41705=CARTESIAN_POINT('Ctrl Pts',(83.0250204169708,194.280208720415,50.328314678029));
#41706=CARTESIAN_POINT('Ctrl Pts',(81.5930418740195,193.643740691757,58.3368436701622));
#41707=CARTESIAN_POINT('Ctrl Pts',(75.3466598718807,193.113350667877,60.9195670203631));
#41708=CARTESIAN_POINT('Ctrl Pts',(70.7482377838634,192.689038648772,59.146500258619));
#41709=CARTESIAN_POINT('Ctrl Pts',(67.4701935758559,192.264726629667,55.4663266741922));
#41710=CARTESIAN_POINT('Ctrl Pts',(67.6892465309357,191.734336605787,48.7106058523097));
#41711=CARTESIAN_POINT('Ctrl Pts',(74.6813889215455,191.09786857713,44.5516343502816));
#41712=CARTESIAN_POINT('Ctrl Pts',(81.9422638078207,190.461400548472,48.1865685182189));
#41713=CARTESIAN_POINT('Ctrl Pts',(82.8227732812904,189.824932519816,56.2586037997643));
#41714=CARTESIAN_POINT('Ctrl Pts',(76.4902181824824,189.188464491159,61.3660341796913));
#41715=CARTESIAN_POINT('Ctrl Pts',(70.0806525778287,188.658074467278,59.2200572972461));
#41716=CARTESIAN_POINT('Ctrl Pts',(67.7715050437085,188.233762448174,54.8660833530394));
#41717=CARTESIAN_POINT('Ctrl Pts',(67.709782312098,187.809450429068,49.938057201976));
#41718=CARTESIAN_POINT('Ctrl Pts',(72.3050806194153,187.279060405188,44.9811447065694));
#41719=CARTESIAN_POINT('Ctrl Pts',(80.3112830930193,186.642592376531,46.4260741570604));
#41720=CARTESIAN_POINT('Ctrl Pts',(83.4096973447483,186.006124347874,53.9315974328931));
#41721=CARTESIAN_POINT('Ctrl Pts',(78.7814218299252,185.369656319217,60.6033375565992));
#41722=CARTESIAN_POINT('Ctrl Pts',(70.6512751961183,184.73318829056,60.307001804386));
#41723=CARTESIAN_POINT('Ctrl Pts',(67.2192465592645,184.202798266679,54.4838645523399));
#41724=CARTESIAN_POINT('Ctrl Pts',(68.3308679122969,183.778486247575,49.6824533630493));
#41725=CARTESIAN_POINT('Ctrl Pts',(71.5157111174391,183.35417422847,45.9213331576022));
#41726=CARTESIAN_POINT('Ctrl Pts',(78.2355346432551,182.823784204589,45.1921419602876));
#41727=CARTESIAN_POINT('Ctrl Pts',(83.3327162377549,182.187316175932,51.5329493976676));
#41728=CARTESIAN_POINT('Ctrl Pts',(80.7504307142551,181.550848147276,59.2313162371021));
#41729=CARTESIAN_POINT('Ctrl Pts',(72.8812493485224,180.914380118618,61.2335737511561));
#41730=CARTESIAN_POINT('Ctrl Pts',(66.9373254266475,180.277912089962,55.6786779306922));
#41731=CARTESIAN_POINT('Ctrl Pts',(68.1645456866902,179.747522066081,49.0317479285263));
#41732=CARTESIAN_POINT('Ctrl Pts',(72.1522356671046,179.323210046976,46.1356160148762));
#41733=CARTESIAN_POINT('Ctrl Pts',(77.023055030443,178.898898027871,45.3843702688699));
#41734=CARTESIAN_POINT('Ctrl Pts',(82.5746552051696,178.368508003991,49.2402078588529));
#41735=CARTESIAN_POINT('Ctrl Pts',(82.2651703589308,177.732039975334,57.3698645733266));
#41736=CARTESIAN_POINT('Ctrl Pts',(75.2675184325902,177.095571946677,61.4888350802814));
#41737=CARTESIAN_POINT('Ctrl Pts',(68.0133711206639,176.45910391802,57.840493361602));
#41738=CARTESIAN_POINT('Ctrl Pts',(67.1682236282861,175.822635889363,49.7489653920918));
#41739=CARTESIAN_POINT('Ctrl Pts',(72.4533484582045,175.292245865482,45.5352730026869));
#41740=CARTESIAN_POINT('Ctrl Pts',(77.3631181809475,174.867933846378,45.963540104857));
#41741=CARTESIAN_POINT('Ctrl Pts',(81.53318681453,174.443621827273,48.5902831513639));
#41742=CARTESIAN_POINT('Ctrl Pts',(83.1962506025606,173.913231803392,55.1417690024739));
#41743=CARTESIAN_POINT('Ctrl Pts',(77.6317485041141,173.276763774735,61.0767008101384));
#41744=CARTESIAN_POINT('Ctrl Pts',(69.6476161095727,172.640295746078,59.5979579569643));
#41745=CARTESIAN_POINT('Ctrl Pts',(66.5630728625792,172.003827717421,52.0867234727528));
#41746=CARTESIAN_POINT('Ctrl Pts',(71.2308284781632,171.367359688764,45.4234542542364));
#41747=CARTESIAN_POINT('Ctrl Pts',(77.984119150899,170.836969664883,45.7077307215896));
#41748=CARTESIAN_POINT('Ctrl Pts',(81.4101558487953,170.412657645779,49.2505437262273));
#41749=CARTESIAN_POINT('Ctrl Pts',(82.8361183764638,169.988345626674,53.968157774753));
#41750=CARTESIAN_POINT('Ctrl Pts',(79.7957358492659,169.457955602793,60.0050296558403));
#41751=CARTESIAN_POINT('Ctrl Pts',(71.7028515441215,168.821487574137,60.8370890219851));
#41752=CARTESIAN_POINT('Ctrl Pts',(66.6445051896481,168.18501954548,54.4852245179543));
#41753=CARTESIAN_POINT('Ctrl Pts',(69.2410082836161,167.548551516823,46.7916413343917));
#41754=CARTESIAN_POINT('Ctrl Pts',(77.1344424145289,166.912083488166,44.8216675309665));
#41755=CARTESIAN_POINT('Ctrl Pts',(82.0467512839816,166.381693464285,49.4646159036547));
#41756=CARTESIAN_POINT('Ctrl Pts',(82.3102791092707,165.95738144518,54.3859779637414));
#41757=CARTESIAN_POINT('Ctrl Pts',(80.2934064564848,165.533069426076,58.8828075295142));
#41758=CARTESIAN_POINT('Ctrl Pts',(74.039380907102,165.002679402195,61.446966738303));
#41759=CARTESIAN_POINT('Ctrl Pts',(67.3836699068338,164.366211373538,56.7684402345682));
#41760=CARTESIAN_POINT('Ctrl Pts',(67.7297256839352,163.729743344881,48.6559008097939));
#41761=CARTESIAN_POINT('Ctrl Pts',(74.7349750628069,163.093275316224,44.5498648066396));
#41762=CARTESIAN_POINT('Ctrl Pts',(81.9862638229229,162.456807287567,48.2384838548278));
#41763=CARTESIAN_POINT('Ctrl Pts',(82.6505339267891,161.926417263686,54.9650352185995));
#41764=CARTESIAN_POINT('Ctrl Pts',(79.6224228708578,161.502105244582,58.8534532612115));
#41765=CARTESIAN_POINT('Ctrl Pts',(75.1509931548911,161.077793225477,60.9260284073355));
#41766=CARTESIAN_POINT('Ctrl Pts',(68.7478297154571,160.547403201596,58.7610235601704));
#41767=CARTESIAN_POINT('Ctrl Pts',(66.7906251178065,159.910935172939,50.8644135705499));
#41768=CARTESIAN_POINT('Ctrl Pts',(72.3715138911219,159.274467144282,44.9663858477208));
#41769=CARTESIAN_POINT('Ctrl Pts',(80.3529008288988,158.637999115625,46.4598760783115));
#41770=CARTESIAN_POINT('Ctrl Pts',(83.4088749123851,158.001531086968,53.9996454094183));
#41771=CARTESIAN_POINT('Ctrl Pts',(79.4996104357941,157.471141063088,59.5137545190037));
#41772=CARTESIAN_POINT('Ctrl Pts',(74.6636507067732,157.046829043983,60.4638834262844));
#41773=CARTESIAN_POINT('Ctrl Pts',(69.9286878056629,156.622517024879,59.0966315232787));
#41774=CARTESIAN_POINT('Ctrl Pts',(66.5139699521479,156.092127000998,53.2633262851448));
#41775=CARTESIAN_POINT('Ctrl Pts',(70.2143122162198,155.455658972341,46.0180128830924));
#41776=CARTESIAN_POINT('Ctrl Pts',(78.2953693841028,154.819190943683,45.2245612029049));
#41777=CARTESIAN_POINT('Ctrl Pts',(83.3419726606467,154.182722915027,51.5857596661316));
#41778=CARTESIAN_POINT('Ctrl Pts',(80.7051888305738,153.54625488637,59.282152990196));
#41779=CARTESIAN_POINT('Ctrl Pts',(74.1379497527392,153.015864862489,60.8818776274124));
#41780=CARTESIAN_POINT('Ctrl Pts',(69.8637868359816,152.591552843385,58.4281492801464));
#41781=CARTESIAN_POINT('Ctrl Pts',(67.1854472627357,152.16724082428,54.2910308903069));
#41782=CARTESIAN_POINT('Ctrl Pts',(68.432404550129,151.636850800399,47.647775246892));
#41783=CARTESIAN_POINT('Ctrl Pts',(75.9771066703128,151.000382771742,44.6039997816288));
#41784=CARTESIAN_POINT('Ctrl Pts',(82.5985720801216,150.363914743085,49.3039196049969));
#41785=CARTESIAN_POINT('Ctrl Pts',(82.2375297733488,149.727446714428,57.4158058820656));
#41786=CARTESIAN_POINT('Ctrl Pts',(75.2000258565176,149.090978685771,61.497550335829));
#41787=CARTESIAN_POINT('Ctrl Pts',(69.1927935718333,148.56058866189,58.3990170863381));
#41788=CARTESIAN_POINT('Ctrl Pts',(67.5747895850749,148.136276642786,53.7437711701705));
#41789=CARTESIAN_POINT('Ctrl Pts',(68.2654736973507,147.711964623681,48.8639958783961));
#41790=CARTESIAN_POINT('Ctrl Pts',(73.5630905523075,147.1815745998,44.6660197376315));
#41791=CARTESIAN_POINT('Ctrl Pts',(81.2552091462713,146.545106571144,47.315248059547));
#41792=CARTESIAN_POINT('Ctrl Pts',(83.172530218171,145.908638542486,55.2055541642953));
#41793=CARTESIAN_POINT('Ctrl Pts',(77.5807549411311,145.27217051383,61.0932616783001));
#41794=CARTESIAN_POINT('Ctrl Pts',(69.5909445553386,144.635702485172,59.5602811942995));
#41795=CARTESIAN_POINT('Ctrl Pts',(67.0872942092809,144.105312461292,53.2817875083084));
#41796=CARTESIAN_POINT('Ctrl Pts',(68.9182795434562,143.681000442187,48.7061187979232));
#41797=CARTESIAN_POINT('Ctrl Pts',(72.6395485245209,143.256688423083,45.4748019438016));
#41798=CARTESIAN_POINT('Ctrl Pts',(79.3919650625709,142.726298399202,45.7791355058949));
#41799=CARTESIAN_POINT('Ctrl Pts',(83.4623219070964,142.089830370545,52.8232319222899));
#41800=CARTESIAN_POINT('Ctrl Pts',(79.7360013175807,141.453362341888,60.0376331714256));
#41801=CARTESIAN_POINT('Ctrl Pts',(71.6534921155156,140.816894313231,60.8161545378098));
#41802=CARTESIAN_POINT('Ctrl Pts',(66.6264240143533,140.180426284574,54.4196175472566));
#41803=CARTESIAN_POINT('Ctrl Pts',(68.8531573323029,139.650036260693,48.0376580714305));
#41804=CARTESIAN_POINT('Ctrl Pts',(73.2359396256076,139.225724241589,45.7836680957074));
#41805=CARTESIAN_POINT('Ctrl Pts',(78.164352269396,138.801412222484,45.784171788142));
#41806=CARTESIAN_POINT('Ctrl Pts',(83.0628491749938,138.271022198603,50.4416900206561));
#41807=CARTESIAN_POINT('Ctrl Pts',(81.5169481905285,137.634554169946,58.4290105545691));
#41808=CARTESIAN_POINT('Ctrl Pts',(73.9729024601451,136.998086141289,61.4324127149976));
#41809=CARTESIAN_POINT('Ctrl Pts',(67.3601309900174,136.361618112632,56.7202684044691));
#41810=CARTESIAN_POINT('Ctrl Pts',(67.7590947577619,135.725150083975,48.5945113888264));
#41811=CARTESIAN_POINT('Ctrl Pts',(73.6251008021535,135.194760060095,45.2362795463956));
#41812=CARTESIAN_POINT('Ctrl Pts',(78.4120938759237,134.77044804099,46.408435147345));
#41813=CARTESIAN_POINT('Ctrl Pts',(82.1327022867324,134.346136021885,49.640512574416));
#41814=CARTESIAN_POINT('Ctrl Pts',(82.7769905318885,133.815745998004,56.369007255807));
#41815=CARTESIAN_POINT('Ctrl Pts',(76.3723312622475,133.179277969348,61.385723194052));
#41816=CARTESIAN_POINT('Ctrl Pts',(68.7071821389033,132.542809940691,58.7064435452887));
#41817=CARTESIAN_POINT('Ctrl Pts',(66.804440904768,131.906341912034,50.8126088424777));
#41818=CARTESIAN_POINT('Ctrl Pts',(72.4339422147442,131.269873883377,44.9392951128856));
#41819=CARTESIAN_POINT('Ctrl Pts',(79.0648474342985,130.739483859496,46.2503420188497));
#41820=CARTESIAN_POINT('Ctrl Pts',(81.9103997196017,130.315171840391,50.2742808395536));
#41821=CARTESIAN_POINT('Ctrl Pts',(82.6000863742362,129.890859821287,55.1541972076467));
#41822=CARTESIAN_POINT('Ctrl Pts',(78.6744613590471,129.360469797406,60.6566708568771));
#41823=CARTESIAN_POINT('Ctrl Pts',(70.5493602448022,128.724001768749,60.2445652289898));
#41824=CARTESIAN_POINT('Ctrl Pts',(66.5190707704739,128.087533740092,53.1954647705981));
#41825=CARTESIAN_POINT('Ctrl Pts',(70.2587128993032,127.451065711435,45.987959843949));
#41826=CARTESIAN_POINT('Ctrl Pts',(78.3602667533996,126.814597682778,45.245043755542));
#41827=CARTESIAN_POINT('Ctrl Pts',(82.5068930122806,126.284207658897,50.5829495892478));
#41828=CARTESIAN_POINT('Ctrl Pts',(82.0166690505848,125.859895639793,55.4869206238833));
#41829=CARTESIAN_POINT('Ctrl Pts',(79.3374838917574,125.435583620688,59.6234914652784));
#41830=CARTESIAN_POINT('Ctrl Pts',(72.7655223446663,124.905193596807,61.203703300415));
#41831=CARTESIAN_POINT('Ctrl Pts',(66.9013213018522,124.268725568151,55.564710013072));
#41832=CARTESIAN_POINT('Ctrl Pts',(68.4807543357559,123.632257539493,47.599884728686));
#41833=CARTESIAN_POINT('Ctrl Pts',(76.0303356832701,122.995789510837,44.610424577313));
#41834=CARTESIAN_POINT('Ctrl Pts',(82.634138445717,122.359321482179,49.3619388875029));
#41835=CARTESIAN_POINT('Ctrl Pts',(82.2646172536146,121.828931458299,56.1111019547982));
#41836=CARTESIAN_POINT('Ctrl Pts',(78.6788293425275,121.404619439194,59.4921338236011));
#41837=CARTESIAN_POINT('Ctrl Pts',(73.9435870692403,120.98030742009,60.8584178549934));
#41838=CARTESIAN_POINT('Ctrl Pts',(67.9455844192023,120.449917396209,57.742055836471));
#41839=CARTESIAN_POINT('Ctrl Pts',(67.2157725389121,119.813449367552,49.6393110061912));
#41840=CARTESIAN_POINT('Ctrl Pts',(73.630997658148,119.176981338895,44.6615668194227));
#41841=CARTESIAN_POINT('Ctrl Pts',(81.2911839951798,118.540513310238,47.3550025066695));
#41842=CARTESIAN_POINT('Ctrl Pts',(83.1613378754544,117.904045281581,55.2726804256891));
#41843=CARTESIAN_POINT('Ctrl Pts',(78.4567365434457,117.3736552577,60.1259756286634));
#41844=CARTESIAN_POINT('Ctrl Pts',(73.5324394582474,116.949343238595,60.3273450848164));
#41845=CARTESIAN_POINT('Ctrl Pts',(69.0614334773316,116.525031219491,58.2538560060471));
#41846=CARTESIAN_POINT('Ctrl Pts',(66.5764423007162,115.99464119561,51.967953773869));
#41847=CARTESIAN_POINT('Ctrl Pts',(71.3386312100502,115.358173166953,45.3718446209629));
#41848=CARTESIAN_POINT('Ctrl Pts',(79.4461546526474,114.721705138296,45.8203021408262));
#41849=CARTESIAN_POINT('Ctrl Pts',(83.4634147283923,114.085237109639,52.8768361344529));
#41850=CARTESIAN_POINT('Ctrl Pts',(79.6835345728483,113.448769080982,60.0809741935798));
#41851=CARTESIAN_POINT('Ctrl Pts',(72.9491322867537,112.918379057102,60.6602615742436));
#41852=CARTESIAN_POINT('Ctrl Pts',(69.0992572779785,112.494067037997,57.5832965341482));
#41853=CARTESIAN_POINT('Ctrl Pts',(67.0833038350869,112.069755018892,53.0860548064605));
#41854=CARTESIAN_POINT('Ctrl Pts',(69.3289827669467,111.539364995011,46.7107372335584));
#41855=CARTESIAN_POINT('Ctrl Pts',(77.249675066892,110.902896966355,44.853391639753));
#41856=CARTESIAN_POINT('Ctrl Pts',(83.0767680675852,110.266428937698,50.5083043429388));
#41857=CARTESIAN_POINT('Ctrl Pts',(81.4826234960783,109.629960909041,58.4701981882822));
#41858=CARTESIAN_POINT('Ctrl Pts',(73.9048702919147,108.993492880384,61.4307311710459));
#41859=CARTESIAN_POINT('Ctrl Pts',(68.440559289883,108.463102856503,57.4521568920576));
#41860=CARTESIAN_POINT('Ctrl Pts',(67.5515651878163,108.038790837398,52.6045862708441));
#41861=CARTESIAN_POINT('Ctrl Pts',(68.9784919825808,107.614478818294,47.8872637926212));
#41862=CARTESIAN_POINT('Ctrl Pts',(74.8544466357378,107.084088794413,44.5464697351562));
#41863=CARTESIAN_POINT('Ctrl Pts',(82.0524617951992,106.447620765756,48.337996726937));
#41864=CARTESIAN_POINT('Ctrl Pts',(82.7438183970427,105.811152737099,56.4284279001484));
#41865=CARTESIAN_POINT('Ctrl Pts',(76.319408331325,105.174684708442,61.3943120940143));
#41866=CARTESIAN_POINT('Ctrl Pts',(68.6569206643761,104.538216679785,58.6605634005361));
#41867=CARTESIAN_POINT('Ctrl Pts',(67.1402418322057,104.007826655904,52.0736496057157));
#41868=CARTESIAN_POINT('Ctrl Pts',(69.6477403827077,103.5835146368,47.8308082864586));
#41869=CARTESIAN_POINT('Ctrl Pts',(73.8183458446825,103.159202617695,45.204917671504));
#41870=CARTESIAN_POINT('Ctrl Pts',(80.4453277976839,102.628812593814,46.5356536389092));
#41871=CARTESIAN_POINT('Ctrl Pts',(83.3936008529561,101.992344565157,54.1181852185861));
#41872=CARTESIAN_POINT('Ctrl Pts',(78.6104527158214,101.355876536501,60.6797813976882));
#41873=CARTESIAN_POINT('Ctrl Pts',(70.5037715895374,100.719408507843,60.2163467894311));
#41874=CARTESIAN_POINT('Ctrl Pts',(66.5112083742668,100.082940479187,53.1278675352251));
#41875=CARTESIAN_POINT('Ctrl Pts',(69.6853422487638,99.5525504553057,47.1602363328864));
#41876=CARTESIAN_POINT('Ctrl Pts',(74.3606460862077,99.1282384362012,45.6011386872139));
#41877=CARTESIAN_POINT('Ctrl Pts',(79.2313117905229,98.7039264170964,46.3533800301158));
#41878=CARTESIAN_POINT('Ctrl Pts',(83.3620653286017,98.1735363932159,51.7035784589593));
#41879=CARTESIAN_POINT('Ctrl Pts',(80.6159271082092,97.5370683645586,59.3616346117788));
#41880=CARTESIAN_POINT('Ctrl Pts',(72.7020417620283,96.9006003359019,61.1791794521838));
#41881=CARTESIAN_POINT('Ctrl Pts',(66.8854056010564,96.2641323072449,55.5135114165275));
#41882=CARTESIAN_POINT('Ctrl Pts',(68.5191436330107,95.6276642785879,47.5436934005256));
#41883=CARTESIAN_POINT('Ctrl Pts',(74.8287480634794,95.0972742547072,45.1195151992875));
#41884=CARTESIAN_POINT('Ctrl Pts',(79.3809339271596,94.6729622356025,47.008127203822));
#41885=CARTESIAN_POINT('Ctrl Pts',(82.5650082795865,94.2486502164979,50.7698983238375));
#41886=CARTESIAN_POINT('Ctrl Pts',(82.175442628398,93.7182601926172,57.5179340842469));
#41887=CARTESIAN_POINT('Ctrl Pts',(75.0805151806506,93.0817921639601,61.4990273607779));
#41888=CARTESIAN_POINT('Ctrl Pts',(67.913737713677,92.4453241353032,57.6819144127156));
#41889=CARTESIAN_POINT('Ctrl Pts',(67.2373285689711,91.8088561066465,49.5902198319534));
#41890=CARTESIAN_POINT('Ctrl Pts',(73.6968276930205,91.1723880779892,44.6443154422948));
#41891=CARTESIAN_POINT('Ctrl Pts',(80.0501636057682,90.6419980541087,46.9514502021527));
#41892=CARTESIAN_POINT('Ctrl Pts',(82.248636684147,90.2176860350039,51.3623421261072));
#41893=CARTESIAN_POINT('Ctrl Pts',(82.1859066479681,89.7933740158994,56.2903555578788));
#41894=CARTESIAN_POINT('Ctrl Pts',(77.4669110080675,89.2629839920186,61.1296559381968));
#41895=CARTESIAN_POINT('Ctrl Pts',(69.4997457803577,88.6265159633616,59.4830298726876));
#41896=CARTESIAN_POINT('Ctrl Pts',(66.5918345240826,87.9900479347046,51.9016643858503));
#41897=CARTESIAN_POINT('Ctrl Pts',(71.387096403826,87.3535799060477,45.3489158004046));
#41898=CARTESIAN_POINT('Ctrl Pts',(79.5071683647652,86.7171118773907,45.8504439794842));
#41899=CARTESIAN_POINT('Ctrl Pts',(82.7910680317342,86.18672185351,51.7583836370666));
#41900=CARTESIAN_POINT('Ctrl Pts',(81.5585650520041,85.7624098344053,56.530195436176));
#41901=CARTESIAN_POINT('Ctrl Pts',(78.2797686720669,85.3380978153008,60.2096988999699));
#41902=CARTESIAN_POINT('Ctrl Pts',(71.5436755152033,84.8077077914198,60.7689814782875));
#41903=CARTESIAN_POINT('Ctrl Pts',(66.608225015574,84.1712397627631,54.3014914295169));
#41904=CARTESIAN_POINT('Ctrl Pts',(69.3840716494891,83.534771734106,46.6707820270848));
#41905=CARTESIAN_POINT('Ctrl Pts',(77.3013012267029,82.8983037054491,44.8678604145149));
#41906=CARTESIAN_POINT('Ctrl Pts',(83.1030684198422,82.2618356767922,50.5710697392593));
#41907=CARTESIAN_POINT('Ctrl Pts',(81.7084038796298,81.7314456529114,57.1848930541526));
#41908=CARTESIAN_POINT('Ctrl Pts',(77.6488577290056,81.3071336338068,59.9794120632335));
#41909=CARTESIAN_POINT('Ctrl Pts',(72.7606223294546,80.882821614702,60.6074296742434));
#41910=CARTESIAN_POINT('Ctrl Pts',(67.308152429271,80.3524315908214,56.6126430706874));
#41911=CARTESIAN_POINT('Ctrl Pts',(67.8228131394891,79.7159635621643,48.4933928886451));
#41912=CARTESIAN_POINT('Ctrl Pts',(74.9222383377375,79.0794955335076,44.5524269697548));
#41913=CARTESIAN_POINT('Ctrl Pts',(82.0819518335224,78.4430275048504,48.3827733219354));
#41914=CARTESIAN_POINT('Ctrl Pts',(82.7225180796838,77.8065594761937,56.4930614826308));
#41915=CARTESIAN_POINT('Ctrl Pts',(77.3326822297666,77.2761694523128,60.5719605413598));
#41916=CARTESIAN_POINT('Ctrl Pts',(72.4352916914142,76.8518574332081,60.0198578733533));
#41917=CARTESIAN_POINT('Ctrl Pts',(68.3328781087648,76.4275454141036,57.2886577272533));
#41918=CARTESIAN_POINT('Ctrl Pts',(66.8357701494069,75.8971553902227,50.6972682092248));
#41919=CARTESIAN_POINT('Ctrl Pts',(72.548355637658,75.2606873615658,44.9047328226551));
#41920=CARTESIAN_POINT('Ctrl Pts',(80.4926040316474,74.6242193329087,46.5846042385617));
#41921=CARTESIAN_POINT('Ctrl Pts',(83.3865044972309,73.987751304252,54.1713288687746));
#41922=CARTESIAN_POINT('Ctrl Pts',(78.5519889954277,73.3512832755949,60.7146123738708));
#41923=CARTESIAN_POINT('Ctrl Pts',(71.808029508702,72.8208932517142,60.2599053673781));
#41924=CARTESIAN_POINT('Ctrl Pts',(68.4725414848908,72.3965812326095,56.6317142086632));
#41925=CARTESIAN_POINT('Ctrl Pts',(67.166153767543,71.9722692135049,51.8795986194627));
#41926=CARTESIAN_POINT('Ctrl Pts',(70.3579984560808,71.4418791896241,45.9214214229869));
#41927=CARTESIAN_POINT('Ctrl Pts',(78.4693120436398,70.8054111609672,45.2939733777076));
#41928=CARTESIAN_POINT('Ctrl Pts',(83.3656604933546,70.1689431323102,51.7715363745729));
#41929=CARTESIAN_POINT('Ctrl Pts',(80.5757216097465,69.5324751036534,59.3971046514366));
#41930=CARTESIAN_POINT('Ctrl Pts',(72.6350621664635,68.8960070749963,61.1671404621037));
#41931=CARTESIAN_POINT('Ctrl Pts',(67.8415543592253,68.3656170511155,56.401636194736));
#41932=CARTESIAN_POINT('Ctrl Pts',(67.7023753752291,67.9413050320109,51.4751891330521));
#41933=CARTESIAN_POINT('Ctrl Pts',(69.8321503171176,67.5169930129063,47.0307195203685));
#41934=CARTESIAN_POINT('Ctrl Pts',(76.1489271116202,66.9866029890255,44.6252925418915));
#41935=CARTESIAN_POINT('Ctrl Pts',(82.6843828424258,66.3501349603685,49.47038465205));
#41936=CARTESIAN_POINT('Ctrl Pts',(82.1335950744637,65.7136669317117,57.57159958279));
#41937=CARTESIAN_POINT('Ctrl Pts',(75.0269014433569,65.0771989030547,61.4994432855063));
#41938=CARTESIAN_POINT('Ctrl Pts',(67.8710625940478,64.4407308743976,57.6289046242914));
#41939=CARTESIAN_POINT('Ctrl Pts',(67.3768502886019,63.910340850517,50.8877250377879));
#41940=CARTESIAN_POINT('Ctrl Pts',(70.5021787723569,63.4860288314123,47.0770068233573));
#41941=CARTESIAN_POINT('Ctrl Pts',(75.0245155457956,63.0617168123077,45.1179964740309));
#41942=CARTESIAN_POINT('Ctrl Pts',(81.3709708767905,62.531326788427,47.4439914766132));
#41943=CARTESIAN_POINT('Ctrl Pts',(83.1281613622351,61.8948587597698,55.3875033424759));
#41944=CARTESIAN_POINT('Ctrl Pts',(77.4001262550961,61.258390731113,61.1427326455332));
#41945=CARTESIAN_POINT('Ctrl Pts',(69.4589948150873,60.621922702456,59.4481878772006));
#41946=CARTESIAN_POINT('Ctrl Pts',(66.5943749115452,59.9854546737991,51.8336588718405));
#41947=CARTESIAN_POINT('Ctrl Pts',(70.6416247147348,59.4550646499183,46.4200171168907));
#41948=CARTESIAN_POINT('Ctrl Pts',(75.5000334115163,59.0307526308137,45.5922995465797));
#41949=CARTESIAN_POINT('Ctrl Pts',(80.1989634148402,58.6064406117091,47.0786737474534));
#41950=CARTESIAN_POINT('Ctrl Pts',(83.4653010752091,58.0760505878282,52.9963410504375));
#41951=CARTESIAN_POINT('Ctrl Pts',(79.5831938141838,57.4395825591714,60.1459104346127));
#41952=CARTESIAN_POINT('Ctrl Pts',(71.4846784404145,56.8031145305144,60.7350617396308));
#41953=CARTESIAN_POINT('Ctrl Pts',(66.6003050078138,56.1666465018575,54.248464273294));
#41954=CARTESIAN_POINT('Ctrl Pts',(69.4305827409398,55.5301784732006,46.6211038439836));
#41955=CARTESIAN_POINT('Ctrl Pts',(76.0361211439636,54.9997884493197,45.1877126110912));
#41956=CARTESIAN_POINT('Ctrl Pts',(80.2469644571503,54.575476430215,47.7485816106596));
#41957=CARTESIAN_POINT('Ctrl Pts',(82.819987485169,54.1511644111105,51.9520092522931));
#41958=CARTESIAN_POINT('Ctrl Pts',(81.4056849883237,53.6207743872297,58.561661018292));
#41959=CARTESIAN_POINT('Ctrl Pts',(73.7865327827989,52.9843063585727,61.4139616395946));
#41960=CARTESIAN_POINT('Ctrl Pts',(67.2858519069638,52.3478383299158,56.5483477348614));
#41961=CARTESIAN_POINT('Ctrl Pts',(67.8516049343422,51.7113703012588,48.4481641547567));
#41962=CARTESIAN_POINT('Ctrl Pts',(74.9899294558238,51.0749022726019,44.5454186863394));
#41963=CARTESIAN_POINT('Ctrl Pts',(80.9170081952258,50.5445122487211,47.7946471543425));
#41964=CARTESIAN_POINT('Ctrl Pts',(82.4169509430253,50.1202002296165,52.4892635598102));
#41965=CARTESIAN_POINT('Ctrl Pts',(81.6032722944373,49.6958882105118,57.3500431781426));
#41966=CARTESIAN_POINT('Ctrl Pts',(76.2013452390112,49.1654981866312,61.4129155743917));
#41967=CARTESIAN_POINT('Ctrl Pts',(68.5785724013713,48.529030157974,58.5703052544606));
#41968=CARTESIAN_POINT('Ctrl Pts',(66.8610935518025,47.8925621293172,50.6341023260653));
#41969=CARTESIAN_POINT('Ctrl Pts',(72.5997511055059,47.2560941006602,44.8894648265617));
#41970=CARTESIAN_POINT('Ctrl Pts',(80.5483061755169,46.6196260720033,46.6236999502513));
#41971=CARTESIAN_POINT('Ctrl Pts',(82.8926257609871,46.0892360481225,52.9634092260413));
#41972=CARTESIAN_POINT('Ctrl Pts',(80.9466881752093,45.6649240290179,57.4913865176607));
#41973=CARTESIAN_POINT('Ctrl Pts',(77.1450146309224,45.2406120099132,60.6277107521473));
#41974=CARTESIAN_POINT('Ctrl Pts',(70.4024354435628,44.7102219860325,60.1529751177799));
#41975=CARTESIAN_POINT('Ctrl Pts',(66.5112404148095,44.0737539573755,53.0083477367719));
#41976=CARTESIAN_POINT('Ctrl Pts',(70.4185371839515,43.4372859287186,45.8903366046345));
#41977=CARTESIAN_POINT('Ctrl Pts',(78.5181271372242,42.8008179000617,45.3161475171128));
#41978=CARTESIAN_POINT('Ctrl Pts',(83.3820793220409,42.1643498714047,51.8375789787671));
#41979=CARTESIAN_POINT('Ctrl Pts',(80.9949109317497,41.6339598475238,58.161278457454));
#41980=CARTESIAN_POINT('Ctrl Pts',(76.5566125769281,41.2096478284193,60.3038841502383));
#41981=CARTESIAN_POINT('Ctrl Pts',(71.6297839982718,40.7853358093146,60.1789377709565));
#41982=CARTESIAN_POINT('Ctrl Pts',(66.8504516413873,40.2549457854338,55.399217042421));
#41983=CARTESIAN_POINT('Ctrl Pts',(68.5975402770678,39.6184777567769,47.4534772741982));
#41984=CARTESIAN_POINT('Ctrl Pts',(76.2150168726171,38.9820097281199,44.641520511437));
#41985=CARTESIAN_POINT('Ctrl Pts',(82.7066979113341,38.345541699463,49.5191354830133));
#41986=CARTESIAN_POINT('Ctrl Pts',(82.1026852762907,37.709073670806,57.6322278590409));
#41987=CARTESIAN_POINT('Ctrl Pts',(76.1537538698749,37.1786836469253,60.8412718198015));
#41988=CARTESIAN_POINT('Ctrl Pts',(71.3978840843149,36.7543716278207,59.5486179512189));
#41989=CARTESIAN_POINT('Ctrl Pts',(67.7600721668191,36.330059608716,56.2236253355719));
#41990=CARTESIAN_POINT('Ctrl Pts',(67.2858844181191,35.7996695848353,49.4810075947219));
#41991=CARTESIAN_POINT('Ctrl Pts',(73.8151741761902,35.1632015561782,44.6276093604353));
#41992=CARTESIAN_POINT('Ctrl Pts',(81.4102273433826,34.5267335275214,47.4995804443723));
#41993=CARTESIAN_POINT('Ctrl Pts',(83.1130419063421,33.8902654988644,55.4389427035715));
#41994=CARTESIAN_POINT('Ctrl Pts',(77.3370337923406,33.2537974702075,61.1682384223835));
#41995=CARTESIAN_POINT('Ctrl Pts',(70.7413467809401,32.7234074463267,59.6901785900305));
#41996=CARTESIAN_POINT('Ctrl Pts',(67.9983065599966,32.2990954272219,55.5956722967659));
#41997=CARTESIAN_POINT('Ctrl Pts',(67.4320581134842,31.8747834081174,50.6998971647794));
#41998=CARTESIAN_POINT('Ctrl Pts',(71.4953694423362,31.3443933842366,45.2983002665808));
#41999=CARTESIAN_POINT('Ctrl Pts',(79.607474293434,30.7079253555797,45.915434008014));
#42000=CARTESIAN_POINT('Ctrl Pts',(83.4584883735393,30.0714573269227,53.0640521347187));
#42001=CARTESIAN_POINT('Ctrl Pts',(79.5380484466973,29.4349892982659,60.1748327661367));
#42002=CARTESIAN_POINT('Ctrl Pts',(71.4203189468987,28.7985212696087,60.712947062398));
#42003=CARTESIAN_POINT('Ctrl Pts',(67.4097973660229,28.2681312457281,55.2720404377711));
#42004=CARTESIAN_POINT('Ctrl Pts',(68.0236907142191,27.8438192266234,50.3820111918258));
#42005=CARTESIAN_POINT('Ctrl Pts',(70.8064704458179,27.4195072075188,46.3144088162878));
#42006=CARTESIAN_POINT('Ctrl Pts',(77.416237077738,26.889117183638,44.9006435679068));
#42007=CARTESIAN_POINT('Ctrl Pts',(83.1361834050853,26.2526491549811,50.6859102435824));
#42008=CARTESIAN_POINT('Ctrl Pts',(81.3561413060791,25.6161811263241,58.6083157669602));
#42009=CARTESIAN_POINT('Ctrl Pts',(73.7334831048529,24.9797130976671,61.4061942193271));
#42010=CARTESIAN_POINT('Ctrl Pts',(67.2517616009762,24.3432450690103,56.4894501586866));
#42011=CARTESIAN_POINT('Ctrl Pts',(67.7915826783805,23.8128550451294,49.7517659321519));
#42012=CARTESIAN_POINT('Ctrl Pts',(71.4615975557508,23.3885430260248,46.4623586555792));
#42013=CARTESIAN_POINT('Ctrl Pts',(76.2298310418815,22.9642310069202,45.2160654137496));
#42014=CARTESIAN_POINT('Ctrl Pts',(82.1472280848147,22.4338409830394,48.4829062967456));
#42015=CARTESIAN_POINT('Ctrl Pts',(82.6722210527895,21.7973729543824,56.6014547617899));
#42016=CARTESIAN_POINT('Ctrl Pts',(76.1333372795995,21.1609049257255,61.4156990954795));
#42017=CARTESIAN_POINT('Ctrl Pts',(68.5436318843579,20.5244368970686,58.529566744947));
#42018=CARTESIAN_POINT('Ctrl Pts',(66.8739394534925,19.8879688684117,50.5674554183872));
#42019=CARTESIAN_POINT('Ctrl Pts',(71.69969081302,19.3575788445308,45.834017496858));
#42020=CARTESIAN_POINT('Ctrl Pts',(76.6273481755489,18.9332668254262,45.7577665390324));
#42021=CARTESIAN_POINT('Ctrl Pts',(81.0448758647264,18.5089548063216,47.9420829924205));
#42022=CARTESIAN_POINT('Ctrl Pts',(83.3696839446724,17.9785647824408,54.2918383373525));
#42023=CARTESIAN_POINT('Ctrl Pts',(78.4436850878909,17.3420967537838,60.7599313649476));
#42024=CARTESIAN_POINT('Ctrl Pts',(70.3478855924792,16.7056287251269,60.1169702163001));
#42025=CARTESIAN_POINT('Ctrl Pts',(66.5142931440722,16.06916069647,52.9422199889477));
#42026=CARTESIAN_POINT('Ctrl Pts',(69.8070609250172,15.5387706725891,47.0525186038545));
#42027=CARTESIAN_POINT('Ctrl Pts',(74.5303225619222,15.1144586534845,45.5808060668782));
#42028=CARTESIAN_POINT('Ctrl Pts',(76.9399431248174,14.9023026439322,46.0267450626822));
#42029=CARTESIAN_POINT('Ctrl Pts',(78.0214523863932,14.7962246391561,46.5322083011042));
#42030=CARTESIAN_POINT('Ctrl Pts',(69.4402165464847,416.203775360844,56.2218531134097));
#42031=CARTESIAN_POINT('Ctrl Pts',(68.9071699408176,416.097697356068,55.2974512802116));
#42032=CARTESIAN_POINT('Ctrl Pts',(68.3253282794076,415.885541346515,53.1857255195819));
#42033=CARTESIAN_POINT('Ctrl Pts',(69.2739184241871,415.461229327411,48.8665709754406));
#42034=CARTESIAN_POINT('Ctrl Pts',(74.2666401826634,414.93083930353,45.482699263787));
#42035=CARTESIAN_POINT('Ctrl Pts',(80.9500366559405,414.294371274873,48.3467661441477));
#42036=CARTESIAN_POINT('Ctrl Pts',(82.1432058326811,413.657903246216,55.5072658902866));
#42037=CARTESIAN_POINT('Ctrl Pts',(76.7605858343834,413.021435217559,60.3899618219047));
#42038=CARTESIAN_POINT('Ctrl Pts',(70.9275499708654,412.491045193678,58.8063170249911));
#42039=CARTESIAN_POINT('Ctrl Pts',(68.6436671409425,412.066733174574,55.0396853566212));
#42040=CARTESIAN_POINT('Ctrl Pts',(68.3338490158116,411.642421155469,50.6454719594405));
#42041=CARTESIAN_POINT('Ctrl Pts',(72.1793410618734,411.112031131589,45.9850203695584));
#42042=CARTESIAN_POINT('Ctrl Pts',(79.3980575202873,410.475563102931,46.8616528307));
#42043=CARTESIAN_POINT('Ctrl Pts',(82.5501083974558,409.839095074275,53.3994982501454));
#42044=CARTESIAN_POINT('Ctrl Pts',(78.763971748798,409.202627045617,59.5917890555278));
#42045=CARTESIAN_POINT('Ctrl Pts',(71.4936844869833,408.566159016961,59.7465702511734));
#42046=CARTESIAN_POINT('Ctrl Pts',(68.1307792218093,408.03576899308,54.7271964843283));
#42047=CARTESIAN_POINT('Ctrl Pts',(68.8751729700556,407.611456973975,50.3852711304698));
#42048=CARTESIAN_POINT('Ctrl Pts',(71.5232625576074,407.187144954871,46.8647613570859));
#42049=CARTESIAN_POINT('Ctrl Pts',(77.4821869316795,406.656754930989,45.8675492875739));
#42050=CARTESIAN_POINT('Ctrl Pts',(82.3576855991202,406.020286902333,51.2630156609909));
#42051=CARTESIAN_POINT('Ctrl Pts',(80.450316784661,405.383818873675,58.2659090049658));
#42052=CARTESIAN_POINT('Ctrl Pts',(73.5313962336346,404.747350845019,60.4584242691296));
#42053=CARTESIAN_POINT('Ctrl Pts',(67.9408201643275,404.110882816362,55.807939090894));
#42054=CARTESIAN_POINT('Ctrl Pts',(68.6931969050106,403.580492792481,49.8131828692861));
#42055=CARTESIAN_POINT('Ctrl Pts',(72.1023249818142,403.156180773377,47.0231564552108));
#42056=CARTESIAN_POINT('Ctrl Pts',(76.4101260871524,402.731868754271,46.1016086092032));
#42057=CARTESIAN_POINT('Ctrl Pts',(81.5629952449066,402.201478730392,49.2561471289245));
#42058=CARTESIAN_POINT('Ctrl Pts',(81.7060283497433,401.565010701734,56.526710854858));
#42059=CARTESIAN_POINT('Ctrl Pts',(75.6739772721628,400.928542673077,60.5631619677914));
#42060=CARTESIAN_POINT('Ctrl Pts',(69.0125175344533,400.29207464442,57.6815769735303));
#42061=CARTESIAN_POINT('Ctrl Pts',(67.8410993127655,399.655606615764,50.5045765788166));
#42062=CARTESIAN_POINT('Ctrl Pts',(72.3400701841959,399.125216591882,46.4719056607541));
#42063=CARTESIAN_POINT('Ctrl Pts',(76.7434507929351,398.700904572778,46.6009029918369));
#42064=CARTESIAN_POINT('Ctrl Pts',(80.6001139604411,398.276592553673,48.7298816915336));
#42065=CARTESIAN_POINT('Ctrl Pts',(82.4219981404177,397.746202529792,54.4904295545201));
#42066=CARTESIAN_POINT('Ctrl Pts',(77.7624770749188,397.109734501136,60.0734769977429));
#42067=CARTESIAN_POINT('Ctrl Pts',(70.5614810577574,396.473266472479,59.1656035270743));
#42068=CARTESIAN_POINT('Ctrl Pts',(67.4216316932075,395.836798443821,52.6219100863238));
#42069=CARTESIAN_POINT('Ctrl Pts',(71.2433726098421,395.200330415165,46.4351620165959));
#42070=CARTESIAN_POINT('Ctrl Pts',(77.2844182849696,394.669940391284,46.3406062239454));
#42071=CARTESIAN_POINT('Ctrl Pts',(80.5243720278798,394.24562837218,49.3254179159407));
#42072=CARTESIAN_POINT('Ctrl Pts',(82.040112162073,393.821316353075,53.4617125063257));
#42073=CARTESIAN_POINT('Ctrl Pts',(79.6382786370442,393.290926329193,59.0055712134925));
#42074=CARTESIAN_POINT('Ctrl Pts',(72.459393009557,392.654458300537,60.165380016475));
#42075=CARTESIAN_POINT('Ctrl Pts',(67.6179776583822,392.01799027188,54.7580446952715));
#42076=CARTESIAN_POINT('Ctrl Pts',(69.5382812257965,391.381522243223,47.7586867184634));
#42077=CARTESIAN_POINT('Ctrl Pts',(76.4805083041517,390.745054214566,45.5937297894312));
#42078=CARTESIAN_POINT('Ctrl Pts',(81.103484898854,390.214664190685,49.4836219539805));
#42079=CARTESIAN_POINT('Ctrl Pts',(81.5924175469392,389.790352171581,53.861674712741));
#42080=CARTESIAN_POINT('Ctrl Pts',(80.0245140776873,389.366040152476,57.9784792750151));
#42081=CARTESIAN_POINT('Ctrl Pts',(74.5758737999407,388.835650128596,60.5891291501815));
#42082=CARTESIAN_POINT('Ctrl Pts',(68.3953150036631,388.199182099938,56.7573869514204));
#42083=CARTESIAN_POINT('Ctrl Pts',(68.2857990871763,387.562714071282,49.5002122847499));
#42084=CARTESIAN_POINT('Ctrl Pts',(74.3252968246704,386.926246042624,45.4749116801571));
#42085=CARTESIAN_POINT('Ctrl Pts',(80.9862825946566,386.289778013968,48.392586076667));
#42086=CARTESIAN_POINT('Ctrl Pts',(81.9259074700354,385.759387990087,54.3608587531254));
#42087=CARTESIAN_POINT('Ctrl Pts',(79.4242394760944,385.335075970982,57.9868838965773));
#42088=CARTESIAN_POINT('Ctrl Pts',(75.540973279493,384.910763951878,60.0669427272804));
#42089=CARTESIAN_POINT('Ctrl Pts',(69.71538839821,384.380373927996,58.4651517178295));
#42090=CARTESIAN_POINT('Ctrl Pts',(67.5616624731461,383.743905899341,51.5194321761466));
#42091=CARTESIAN_POINT('Ctrl Pts',(72.23770936152,383.107437870682,45.9684715947465));
#42092=CARTESIAN_POINT('Ctrl Pts',(79.4370158834858,382.470969842026,46.8896466493991));
#42093=CARTESIAN_POINT('Ctrl Pts',(82.5528425826936,381.834501813369,53.4602767023325));
#42094=CARTESIAN_POINT('Ctrl Pts',(79.3486946499408,381.304111789488,58.5824451564176));
#42095=CARTESIAN_POINT('Ctrl Pts',(75.0822563764807,380.879799770384,59.6796714555959));
#42096=CARTESIAN_POINT('Ctrl Pts',(70.7864481389756,380.455487751278,58.7037448807778));
#42097=CARTESIAN_POINT('Ctrl Pts',(67.4384856247272,379.925097727399,53.6743989342178));
#42098=CARTESIAN_POINT('Ctrl Pts',(70.3669295052165,379.288629698741,47.0181408449584));
#42099=CARTESIAN_POINT('Ctrl Pts',(77.5372518389146,378.652161670085,45.8933939803704));
#42100=CARTESIAN_POINT('Ctrl Pts',(82.3686694072851,378.015693641427,51.309664113827));
#42101=CARTESIAN_POINT('Ctrl Pts',(80.4125657049669,377.379225612771,58.3136068333089));
#42102=CARTESIAN_POINT('Ctrl Pts',(74.6346941598371,376.84883558889,60.0797818118907));
#42103=CARTESIAN_POINT('Ctrl Pts',(70.6940626090962,376.424523569785,58.1105626584799));
#42104=CARTESIAN_POINT('Ctrl Pts',(68.0906807684637,376.000211550681,54.5568597889763));
#42105=CARTESIAN_POINT('Ctrl Pts',(68.8608597118887,375.469821526799,48.564364645708));
#42106=CARTESIAN_POINT('Ctrl Pts',(75.4365206255027,374.833353498142,45.4591691830717));
#42107=CARTESIAN_POINT('Ctrl Pts',(81.5876230698536,374.196885469486,49.3117678641741));
#42108=CARTESIAN_POINT('Ctrl Pts',(81.6837318816807,373.560417440829,56.5691324667567));
#42109=CARTESIAN_POINT('Ctrl Pts',(75.6141987924881,372.923949412171,60.5744193967036));
#42110=CARTESIAN_POINT('Ctrl Pts',(70.0937908220254,372.393559388291,58.1191659501846));
#42111=CARTESIAN_POINT('Ctrl Pts',(68.4098960031221,371.969247369186,54.048428998265));
#42112=CARTESIAN_POINT('Ctrl Pts',(68.774611237156,371.544935350082,49.6582827716665));
#42113=CARTESIAN_POINT('Ctrl Pts',(73.2855399397156,371.014545326201,45.6389923010219));
#42114=CARTESIAN_POINT('Ctrl Pts',(80.2863097486117,370.378077297544,47.6064214343979));
#42115=CARTESIAN_POINT('Ctrl Pts',(82.4041200296613,369.741609268888,54.5485722172613));
#42116=CARTESIAN_POINT('Ctrl Pts',(77.71782626597,369.105141240229,60.0908847886452));
#42117=CARTESIAN_POINT('Ctrl Pts',(70.5089666544688,368.468673211574,59.1349044469688));
#42118=CARTESIAN_POINT('Ctrl Pts',(67.9510509515326,367.938283187692,53.6613095675806));
#42119=CARTESIAN_POINT('Ctrl Pts',(69.3490101067543,367.513971168588,49.48373715131));
#42120=CARTESIAN_POINT('Ctrl Pts',(72.5031100488934,367.089659149483,46.4083421119939));
#42121=CARTESIAN_POINT('Ctrl Pts',(78.5444099231439,366.559269125602,46.3317296040275));
#42122=CARTESIAN_POINT('Ctrl Pts',(82.5398749139707,365.922801096946,52.4077327984871));
#42123=CARTESIAN_POINT('Ctrl Pts',(79.5866549502363,365.286333068288,59.0377455981978));
#42124=CARTESIAN_POINT('Ctrl Pts',(72.4142669929032,364.649865039632,60.149244076846));
#42125=CARTESIAN_POINT('Ctrl Pts',(67.5984596608489,364.013397010975,54.700431816129));
#42126=CARTESIAN_POINT('Ctrl Pts',(69.2564282586696,363.483006987094,48.8905855379879));
#42127=CARTESIAN_POINT('Ctrl Pts',(73.0512341120044,363.058694967989,46.6532099261719));
#42128=CARTESIAN_POINT('Ctrl Pts',(77.4491933428809,362.634382948884,46.3995256806998));
#42129=CARTESIAN_POINT('Ctrl Pts',(82.0605959468057,362.103992925004,50.3031316638272));
#42130=CARTESIAN_POINT('Ctrl Pts',(81.092957438863,361.467524896347,57.5104356694839));
#42131=CARTESIAN_POINT('Ctrl Pts',(74.5158004127629,360.83105686769,60.5795696405825));
#42132=CARTESIAN_POINT('Ctrl Pts',(68.3718257628123,360.194588839033,56.715613975814));
#42133=CARTESIAN_POINT('Ctrl Pts',(68.3088414159556,359.558120810376,49.4439162177894));
#42134=CARTESIAN_POINT('Ctrl Pts',(73.3702810557735,359.027730786495,46.1446735138543));
#42135=CARTESIAN_POINT('Ctrl Pts',(77.7024589502714,358.603418767391,46.94382042355));
#42136=CARTESIAN_POINT('Ctrl Pts',(81.1892545126691,358.179106748286,49.6361535750933));
#42137=CARTESIAN_POINT('Ctrl Pts',(82.1111485232127,357.648716724405,55.6071907614047));
#42138=CARTESIAN_POINT('Ctrl Pts',(76.6545544313477,357.012248695748,60.4141790314787));
#42139=CARTESIAN_POINT('Ctrl Pts',(69.6763015836446,356.375780667091,58.41854252348));
#42140=CARTESIAN_POINT('Ctrl Pts',(67.5713198586051,355.739312638434,51.4724911404437));
#42141=CARTESIAN_POINT('Ctrl Pts',(72.2920211553507,355.102844609777,45.9410777063465));
#42142=CARTESIAN_POINT('Ctrl Pts',(78.2768000197099,354.572454585897,46.7690847061429));
#42143=CARTESIAN_POINT('Ctrl Pts',(81.0235601960107,354.148142566792,50.2131679842795));
#42144=CARTESIAN_POINT('Ctrl Pts',(81.8906440817231,353.723830547688,54.5322612488422));
#42145=CARTESIAN_POINT('Ctrl Pts',(78.6712966263086,353.193440523806,59.6448902798114));
#42146=CARTESIAN_POINT('Ctrl Pts',(71.3995065100964,352.55697249515,59.6961134949115));
#42147=CARTESIAN_POINT('Ctrl Pts',(67.4395381257376,351.920504466493,53.6135788034026));
#42148=CARTESIAN_POINT('Ctrl Pts',(70.4050013477498,351.284036437836,46.9890331014375));
#42149=CARTESIAN_POINT('Ctrl Pts',(77.5962200355992,350.647568409179,45.908325418698));
#42150=CARTESIAN_POINT('Ctrl Pts',(81.5717652720708,350.117178385298,50.4578543745087));
#42151=CARTESIAN_POINT('Ctrl Pts',(81.3871809202268,349.692866366193,54.8592552548996));
#42152=CARTESIAN_POINT('Ctrl Pts',(79.2096775036626,349.268554347089,58.6887304100229));
#42153=CARTESIAN_POINT('Ctrl Pts',(73.4265856234102,348.738164323208,60.4377363995915));
#42154=CARTESIAN_POINT('Ctrl Pts',(67.9028145600792,348.101696294551,55.7080949172044));
#42155=CARTESIAN_POINT('Ctrl Pts',(68.9015357974914,347.465228265894,48.5191357596856));
#42156=CARTESIAN_POINT('Ctrl Pts',(75.4843515237355,346.828760237237,45.4621576778466));
#42157=CARTESIAN_POINT('Ctrl Pts',(81.6223529455147,346.19229220858,49.3617081465855));
#42158=CARTESIAN_POINT('Ctrl Pts',(81.640626656908,345.661902184699,55.4034661455841));
#42159=CARTESIAN_POINT('Ctrl Pts',(78.6151450718763,345.237590165595,58.6054752448041));
#42160=CARTESIAN_POINT('Ctrl Pts',(74.4600423822037,344.81327814649,60.0688694948707));
#42161=CARTESIAN_POINT('Ctrl Pts',(68.9469512555899,344.282888122609,57.5972303875894));
#42162=CARTESIAN_POINT('Ctrl Pts',(67.8778758710427,343.646420093952,50.4042731977985));
#42163=CARTESIAN_POINT('Ctrl Pts',(73.3459081158512,343.009952065295,45.6315170497992));
#42164=CARTESIAN_POINT('Ctrl Pts',(80.3204623129854,342.373484036639,47.6400417894447));
#42165=CARTESIAN_POINT('Ctrl Pts',(82.3975937641188,341.737016007981,54.6090503449511));
#42166=CARTESIAN_POINT('Ctrl Pts',(78.4496417365585,341.206625984101,59.1825444616058));
#42167=CARTESIAN_POINT('Ctrl Pts',(74.0657646720175,340.782313964996,59.6161606234846));
#42168=CARTESIAN_POINT('Ctrl Pts',(69.9690846948357,340.358001945891,57.9964031547838));
#42169=CARTESIAN_POINT('Ctrl Pts',(67.427437723079,339.827611922011,52.5152350021043));
#42170=CARTESIAN_POINT('Ctrl Pts',(71.3369105306629,339.191143893354,46.3835486371008));
#42171=CARTESIAN_POINT('Ctrl Pts',(78.594889468703,338.554675864697,46.3656708996847));
#42172=CARTESIAN_POINT('Ctrl Pts',(82.5436142098468,337.91820783604,52.4555108645124));
#42173=CARTESIAN_POINT('Ctrl Pts',(79.5420704476381,337.281739807383,59.0791269732218));
#42174=CARTESIAN_POINT('Ctrl Pts',(73.5624097620586,336.751349783503,59.9433212409216));
#42175=CARTESIAN_POINT('Ctrl Pts',(69.9682598402852,336.327037764397,57.3960702849555));
#42176=CARTESIAN_POINT('Ctrl Pts',(67.9373971274161,335.902725745293,53.486850703718));
#42177=CARTESIAN_POINT('Ctrl Pts',(69.6126145806316,335.372335721412,47.6819544831614));
#42178=CARTESIAN_POINT('Ctrl Pts',(76.5849735178594,334.735867692755,45.6160972367699));
#42179=CARTESIAN_POINT('Ctrl Pts',(82.0764516212286,334.099399664098,50.3618580944983));
#42180=CARTESIAN_POINT('Ctrl Pts',(81.0644511917625,333.462931635441,57.5489599449865));
#42181=CARTESIAN_POINT('Ctrl Pts',(74.4550043118779,332.826463606784,60.581577173387));
#42182=CARTESIAN_POINT('Ctrl Pts',(69.3736998864156,332.296073582903,57.3130118944356));
#42183=CARTESIAN_POINT('Ctrl Pts',(68.3304293115324,331.871761563799,53.0330600722258));
#42184=CARTESIAN_POINT('Ctrl Pts',(69.3605171826439,331.447449544694,48.7499163587087));
#42185=CARTESIAN_POINT('Ctrl Pts',(74.4317337729813,330.917059520814,45.4657214892044));
#42186=CARTESIAN_POINT('Ctrl Pts',(81.0504866017737,330.280591492156,48.4779741850053));
#42187=CARTESIAN_POINT('Ctrl Pts',(82.0846109633492,329.6441234635,55.6619260698194));
#42188=CARTESIAN_POINT('Ctrl Pts',(76.6077708510018,329.007655434842,60.4245724205696));
#42189=CARTESIAN_POINT('Ctrl Pts',(69.6290842909404,328.371187406186,58.3801925125222));
#42190=CARTESIAN_POINT('Ctrl Pts',(67.9360017916063,327.840797382305,52.5804817182293));
#42191=CARTESIAN_POINT('Ctrl Pts',(69.9548185856608,327.4164853632,48.6650277413706));
#42192=CARTESIAN_POINT('Ctrl Pts',(73.5411086122976,326.992173344096,46.1067226505543));
#42193=CARTESIAN_POINT('Ctrl Pts',(79.5234017655623,326.461783320215,46.9525017442868));
#42194=CARTESIAN_POINT('Ctrl Pts',(82.5453250849273,325.825315291558,53.5668448533101));
#42195=CARTESIAN_POINT('Ctrl Pts',(78.6153693748776,325.188847262901,59.6688138794178));
#42196=CARTESIAN_POINT('Ctrl Pts',(71.3573697948376,324.552379234244,59.6732831827373));
#42197=CARTESIAN_POINT('Ctrl Pts',(67.4290363608638,323.915911205587,53.553662954036));
#42198=CARTESIAN_POINT('Ctrl Pts',(69.9537950412676,323.385521181707,48.0646951774213));
#42199=CARTESIAN_POINT('Ctrl Pts',(74.0454684476267,322.961209162602,46.4323319125358));
#42200=CARTESIAN_POINT('Ctrl Pts',(78.4306598152707,322.536897143497,46.8524482797421));
#42201=CARTESIAN_POINT('Ctrl Pts',(82.3926746904323,322.006507119616,51.4137651702888));
#42202=CARTESIAN_POINT('Ctrl Pts',(80.3370103154243,321.37003909096,58.3891360772251));
#42203=CARTESIAN_POINT('Ctrl Pts',(73.368673325257,320.733571062302,60.4191256018276));
#42204=CARTESIAN_POINT('Ctrl Pts',(67.8859719201152,320.097103033646,55.6632278757842));
#42205=CARTESIAN_POINT('Ctrl Pts',(68.9328954799997,319.460635004988,48.4670131505437));
#42206=CARTESIAN_POINT('Ctrl Pts',(74.4383504208568,318.930244981108,45.9784112255296));
#42207=CARTESIAN_POINT('Ctrl Pts',(78.5979391335097,318.505932962003,47.4290051847139));
#42208=CARTESIAN_POINT('Ctrl Pts',(81.6332652045092,318.081620942898,50.6216837992263));
#42209=CARTESIAN_POINT('Ctrl Pts',(81.6335938519759,317.551230919018,56.6634694242698));
#42210=CARTESIAN_POINT('Ctrl Pts',(75.5076280460444,316.91476289036,60.5819000101759));
#42211=CARTESIAN_POINT('Ctrl Pts',(68.9154312388058,316.278294861704,57.5452045804096));
#42212=CARTESIAN_POINT('Ctrl Pts',(67.8945802877852,315.641826833047,50.3593545113968));
#42213=CARTESIAN_POINT('Ctrl Pts',(73.403762837781,315.00535880439,45.6127280311658));
#42214=CARTESIAN_POINT('Ctrl Pts',(79.1922124087143,314.474968780509,47.3439198783492));
#42215=CARTESIAN_POINT('Ctrl Pts',(81.3814962674079,314.050656761405,51.1666724571746));
#42216=CARTESIAN_POINT('Ctrl Pts',(81.5796314386246,313.626344742299,55.5674841489855));
#42217=CARTESIAN_POINT('Ctrl Pts',(77.6181128194239,313.095954718419,60.1292320460879));
#42218=CARTESIAN_POINT('Ctrl Pts',(70.423600772617,312.459486689762,59.0706708903866));
#42219=CARTESIAN_POINT('Ctrl Pts',(67.4377549602559,311.823018661105,52.4552871023261));
#42220=CARTESIAN_POINT('Ctrl Pts',(71.3789767527993,311.186550632448,46.3605886962923));
#42221=CARTESIAN_POINT('Ctrl Pts',(78.6508901146131,310.550082603791,46.3894221886695));
#42222=CARTESIAN_POINT('Ctrl Pts',(81.8859638407731,310.019692579911,51.4921147752653));
#42223=CARTESIAN_POINT('Ctrl Pts',(81.0321823382649,309.595380560806,55.813857275557));
#42224=CARTESIAN_POINT('Ctrl Pts',(78.2960393425849,309.171068541701,59.2663813667178));
#42225=CARTESIAN_POINT('Ctrl Pts',(72.3138382383004,308.640678517821,60.1128112781015));
#42226=CARTESIAN_POINT('Ctrl Pts',(67.576128370855,308.004210489163,54.5959588671773));
#42227=CARTESIAN_POINT('Ctrl Pts',(69.6597135717515,307.367742460507,47.6434592742872));
#42228=CARTESIAN_POINT('Ctrl Pts',(76.6317888771799,306.731274431849,45.6263465322803));
#42229=CARTESIAN_POINT('Ctrl Pts',(82.1031575825955,306.094806403193,50.4165114356426));
#42230=CARTESIAN_POINT('Ctrl Pts',(81.1996524681894,305.564416379312,56.3903587851514));
#42231=CARTESIAN_POINT('Ctrl Pts',(77.7211629929319,305.140104360207,59.0934148451279));
#42232=CARTESIAN_POINT('Ctrl Pts',(73.3914661664338,304.715792341103,59.9058965270541));
#42233=CARTESIAN_POINT('Ctrl Pts',(68.3198923136149,304.185402317221,56.6222533822537));
#42234=CARTESIAN_POINT('Ctrl Pts',(68.3604871663677,303.548934288565,49.3503961662505));
#42235=CARTESIAN_POINT('Ctrl Pts',(74.4925357667877,302.912466259908,45.4675418243239));
#42236=CARTESIAN_POINT('Ctrl Pts',(81.0791113280825,302.275998231251,48.5164105085873));
#42237=CARTESIAN_POINT('Ctrl Pts',(82.0689361798398,301.639530202594,55.7207010409613));
#42238=CARTESIAN_POINT('Ctrl Pts',(77.4695744424442,301.109140178713,59.6384868002357));
#42239=CARTESIAN_POINT('Ctrl Pts',(73.0708549766314,300.684828159609,59.3983448548522));
#42240=CARTESIAN_POINT('Ctrl Pts',(69.2691783424173,300.260516140504,57.1726638665426));
#42241=CARTESIAN_POINT('Ctrl Pts',(67.5933293757376,299.730126116623,51.3679499297607));
#42242=CARTESIAN_POINT('Ctrl Pts',(72.3923372591493,299.093658087966,45.9043358651546));
#42243=CARTESIAN_POINT('Ctrl Pts',(79.568113468025,298.457190059309,46.9937456496989));
#42244=CARTESIAN_POINT('Ctrl Pts',(82.5417329130637,297.820722030653,53.6146342059745));
#42245=CARTESIAN_POINT('Ctrl Pts',(78.5649945721503,297.184254001995,59.7029104382029));
#42246=CARTESIAN_POINT('Ctrl Pts',(72.5234874474323,296.653863978115,59.6448991550778));
#42247=CARTESIAN_POINT('Ctrl Pts',(69.3599334673634,296.22955195901,56.5792300098432));
#42248=CARTESIAN_POINT('Ctrl Pts',(67.9491184008433,295.805239939905,52.4059816418528));
#42249=CARTESIAN_POINT('Ctrl Pts',(70.4901690530445,295.274849916025,46.9245370120187));
#42250=CARTESIAN_POINT('Ctrl Pts',(77.6960510788033,294.638381887367,45.9463654816353));
#42251=CARTESIAN_POINT('Ctrl Pts',(82.3993871341864,294.001913858711,51.4742229172667));
#42252=CARTESIAN_POINT('Ctrl Pts',(80.3029614283332,293.365445830054,58.4228614269583));
#42253=CARTESIAN_POINT('Ctrl Pts',(73.3082824193387,292.728977801396,60.4118362566478));
#42254=CARTESIAN_POINT('Ctrl Pts',(68.7849999031238,292.198587777516,56.4064537623666));
#42255=CARTESIAN_POINT('Ctrl Pts',(68.4067693560527,291.774275758411,52.0174512850244));
#42256=CARTESIAN_POINT('Ctrl Pts',(70.0781225968146,291.349963739307,47.9415489999532));
#42257=CARTESIAN_POINT('Ctrl Pts',(75.5909447974727,290.819573715426,45.4693101298355));
#42258=CARTESIAN_POINT('Ctrl Pts',(81.6727811963644,290.183105686769,49.4558902844448));
#42259=CARTESIAN_POINT('Ctrl Pts',(81.5990179045781,289.546637658112,56.7135164015244));
#42260=CARTESIAN_POINT('Ctrl Pts',(75.4598065759558,288.910169629455,60.5850357597409));
#42261=CARTESIAN_POINT('Ctrl Pts',(68.8746160885175,288.273701600798,57.5001011484147));
#42262=CARTESIAN_POINT('Ctrl Pts',(68.0859902013625,287.743311576918,51.5100057520876));
#42263=CARTESIAN_POINT('Ctrl Pts',(70.6784180277171,287.318999557812,47.9483040439154));
#42264=CARTESIAN_POINT('Ctrl Pts',(74.6129677721632,286.894687538709,45.9669612161011));
#42265=CARTESIAN_POINT('Ctrl Pts',(80.3962498951809,286.364297514827,47.7153380440689));
#42266=CARTESIAN_POINT('Ctrl Pts',(82.3739091167288,285.727829486171,54.7132248190485));
#42267=CARTESIAN_POINT('Ctrl Pts',(77.5591908754027,285.091361457513,60.144344973784));
#42268=CARTESIAN_POINT('Ctrl Pts',(70.3854394892496,284.454893428857,59.0416805061446));
#42269=CARTESIAN_POINT('Ctrl Pts',(67.4365152020778,283.8184254002,52.3944705003951));
#42270=CARTESIAN_POINT('Ctrl Pts',(70.7689767411451,283.288035376319,47.3548401828391));
#42271=CARTESIAN_POINT('Ctrl Pts',(75.0617597872492,282.863723357214,46.3656916540868));
#42272=CARTESIAN_POINT('Ctrl Pts',(79.3315561430612,282.43941133811,47.4497766012886));
#42273=CARTESIAN_POINT('Ctrl Pts',(82.5514597900143,281.909021314229,52.5620553643578));
#42274=CARTESIAN_POINT('Ctrl Pts',(79.4558785027385,281.272553285572,59.14224774801));
#42275=CARTESIAN_POINT('Ctrl Pts',(72.259442357487,280.636085256915,60.0855847428586));
#42276=CARTESIAN_POINT('Ctrl Pts',(67.5663265020588,279.999617228258,54.5490477885832));
#42277=CARTESIAN_POINT('Ctrl Pts',(69.698656693656,279.363149199601,47.5967299545071));
#42278=CARTESIAN_POINT('Ctrl Pts',(75.5192821269783,278.83275917572,45.977009851541));
#42279=CARTESIAN_POINT('Ctrl Pts',(79.408934314618,278.408447156615,48.0451024394208));
#42280=CARTESIAN_POINT('Ctrl Pts',(81.9217548016931,277.984135137511,51.6634078843202));
#42281=CARTESIAN_POINT('Ctrl Pts',(81.0005103947078,277.45374511363,57.6345453295302));
#42282=CARTESIAN_POINT('Ctrl Pts',(74.348539571935,276.817277084973,60.5727147400631));
#42283=CARTESIAN_POINT('Ctrl Pts',(68.296676761267,276.180809056316,56.5660285283193));
#42284=CARTESIAN_POINT('Ctrl Pts',(68.3838476789665,275.54434102766,49.3085510664432));
#42285=CARTESIAN_POINT('Ctrl Pts',(74.5525794359645,274.907872999002,45.4577973970669));
#42286=CARTESIAN_POINT('Ctrl Pts',(80.0092319483338,274.377482975122,48.0516588055164));
#42287=CARTESIAN_POINT('Ctrl Pts',(81.5898034221531,273.953170956017,52.1636163574618));
#42288=CARTESIAN_POINT('Ctrl Pts',(81.1143528981921,273.528858936913,56.5431537636407));
#42289=CARTESIAN_POINT('Ctrl Pts',(76.5033750007141,272.998468913031,60.4472614050817));
#42290=CARTESIAN_POINT('Ctrl Pts',(69.5545150337097,272.362000884375,58.3036895096301));
#42291=CARTESIAN_POINT('Ctrl Pts',(67.6126698935678,271.725532855717,51.3102772287588));
#42292=CARTESIAN_POINT('Ctrl Pts',(72.4374133801518,271.089064827061,45.88806106125));
#42293=CARTESIAN_POINT('Ctrl Pts',(79.6198359734671,270.452596798404,47.0257609351353));
#42294=CARTESIAN_POINT('Ctrl Pts',(82.0387273789565,269.922206774523,52.5621982386224));
#42295=CARTESIAN_POINT('Ctrl Pts',(80.5357298745602,269.497894755419,56.7031401115096));
#42296=CARTESIAN_POINT('Ctrl Pts',(77.304981575641,269.073582736314,59.697913311918));
#42297=CARTESIAN_POINT('Ctrl Pts',(71.2636734023524,268.543192712433,59.6219580464909));
#42298=CARTESIAN_POINT('Ctrl Pts',(67.422901911245,267.906724683776,53.4470062519336));
#42299=CARTESIAN_POINT('Ctrl Pts',(70.5425886864608,267.270256655119,46.8936763881869));
#42300=CARTESIAN_POINT('Ctrl Pts',(77.7407552738591,266.633788626463,45.9636357124148));
#42301=CARTESIAN_POINT('Ctrl Pts',(82.4174441785092,265.997320597805,51.5323102585822));
#42302=CARTESIAN_POINT('Ctrl Pts',(80.6133050746085,265.466930573925,57.2984403074771));
#42303=CARTESIAN_POINT('Ctrl Pts',(76.763215206849,265.042618554819,59.4392833897759));
#42304=CARTESIAN_POINT('Ctrl Pts',(72.3602526468608,264.618306535715,59.5818378993367));
#42305=CARTESIAN_POINT('Ctrl Pts',(67.8488867063496,264.087916511834,55.5630382031854));
#42306=CARTESIAN_POINT('Ctrl Pts',(68.9982017502957,263.451448483178,48.3824650894454));
#42307=CARTESIAN_POINT('Ctrl Pts',(75.6507576527478,262.81498045452,45.4803834497805));
#42308=CARTESIAN_POINT('Ctrl Pts',(81.6952081767768,262.178512425863,49.4982430467674));
#42309=CARTESIAN_POINT('Ctrl Pts',(81.5745614419011,261.542044397206,56.7692126985655));
#42310=CARTESIAN_POINT('Ctrl Pts',(76.4314293975865,261.011654373326,59.9396017002077));
#42311=CARTESIAN_POINT('Ctrl Pts',(72.1208112787717,260.587342354221,59.0313217177135));
#42312=CARTESIAN_POINT('Ctrl Pts',(68.7031090722866,260.163030335117,56.2518050833615));
#42313=CARTESIAN_POINT('Ctrl Pts',(67.9322782008732,259.632640311235,50.2593937644792));
#42314=CARTESIAN_POINT('Ctrl Pts',(73.5085094149935,258.996172282579,45.5917176019033));
#42315=CARTESIAN_POINT('Ctrl Pts',(80.4341473613234,258.359704253922,47.7629193232736));
#42316=CARTESIAN_POINT('Ctrl Pts',(82.3630695451455,257.723236225265,54.7599070385188));
#42317=CARTESIAN_POINT('Ctrl Pts',(77.5042046999709,257.086768196608,60.1703587505607));
#42318=CARTESIAN_POINT('Ctrl Pts',(71.542241236904,256.556378172727,59.1914995614827));
#42319=CARTESIAN_POINT('Ctrl Pts',(68.8833202238815,256.132066153623,55.6791584420352));
#42320=CARTESIAN_POINT('Ctrl Pts',(68.1255702744068,255.707754134518,51.3395483089789));
#42321=CARTESIAN_POINT('Ctrl Pts',(71.4729856187442,255.177364110637,46.3098381623122));
#42322=CARTESIAN_POINT('Ctrl Pts',(78.7437506296847,254.54089608198,46.4422446111449));
#42323=CARTESIAN_POINT('Ctrl Pts',(82.5488719109899,253.904428053323,52.6228295278893));
#42324=CARTESIAN_POINT('Ctrl Pts',(79.4170838257604,253.267960024666,59.1703848936531));
#42325=CARTESIAN_POINT('Ctrl Pts',(72.200869981999,252.631491996009,60.0691691130958));
#42326=CARTESIAN_POINT('Ctrl Pts',(68.3414682869996,252.101101972129,55.4207078404137));
#42327=CARTESIAN_POINT('Ctrl Pts',(68.6371295416553,251.676789953024,51.0253710483865));
#42328=CARTESIAN_POINT('Ctrl Pts',(70.9106332758805,251.252477933919,47.2520990116368));
#42329=CARTESIAN_POINT('Ctrl Pts',(76.7360438614395,250.722087910039,45.649674237537));
#42330=CARTESIAN_POINT('Ctrl Pts',(82.1386298989004,250.085619881381,50.5172834473894));
#42331=CARTESIAN_POINT('Ctrl Pts',(80.9587052447333,249.449151852725,57.6787327203381));
#42332=CARTESIAN_POINT('Ctrl Pts',(74.3007993835847,248.812683824068,60.5685194637872));
#42333=CARTESIAN_POINT('Ctrl Pts',(68.2632189551499,248.176215795411,56.5152272362032));
#42334=CARTESIAN_POINT('Ctrl Pts',(68.3975059844324,247.64582577153,50.4749341439143));
#42335=CARTESIAN_POINT('Ctrl Pts',(71.5028739501969,247.221513752425,47.3503396278119));
#42336=CARTESIAN_POINT('Ctrl Pts',(75.6936026826867,246.797201733321,45.9923286618994));
#42337=CARTESIAN_POINT('Ctrl Pts',(81.1425269447101,246.26681170944,48.6023857558582));
#42338=CARTESIAN_POINT('Ctrl Pts',(82.0296386774106,245.630343680783,55.8200438307264));
#42339=CARTESIAN_POINT('Ctrl Pts',(76.4428373212789,244.993875652126,60.4532099712461));
#42340=CARTESIAN_POINT('Ctrl Pts',(69.5212222752298,244.357407623469,58.2692175186869));
#42341=CARTESIAN_POINT('Ctrl Pts',(67.6207211562919,243.720939594812,51.2499831723409));
#42342=CARTESIAN_POINT('Ctrl Pts',(71.6828955652401,243.190549570931,46.7776333740493));
#42343=CARTESIAN_POINT('Ctrl Pts',(76.0763237452923,242.766237551827,46.45484874062));
#42344=CARTESIAN_POINT('Ctrl Pts',(80.1307985436868,242.341925532722,48.1775313004769));
#42345=CARTESIAN_POINT('Ctrl Pts',(82.5332351792175,241.811535508841,53.7211286757604));
#42346=CARTESIAN_POINT('Ctrl Pts',(78.4701832321027,241.175067480184,59.7521455209579));
#42347=CARTESIAN_POINT('Ctrl Pts',(71.2140669720661,240.538599451527,59.5867529595707));
#42348=CARTESIAN_POINT('Ctrl Pts',(67.4203702079031,239.90213142287,53.3991490016473));
#42349=CARTESIAN_POINT('Ctrl Pts',(70.5882038573061,239.265663394213,46.8534339695275));
#42350=CARTESIAN_POINT('Ctrl Pts',(76.5877790024693,238.735273370333,46.1405021884087));
#42351=CARTESIAN_POINT('Ctrl Pts',(80.1164646781247,238.310961351228,48.777693591261));
#42352=CARTESIAN_POINT('Ctrl Pts',(82.0479717482962,237.886649332123,52.7369462392655));
#42353=CARTESIAN_POINT('Ctrl Pts',(80.2267142779113,237.356259308243,58.4976922737264));
#42354=CARTESIAN_POINT('Ctrl Pts',(73.2044152927096,236.719791279586,60.3868381850957));
#42355=CARTESIAN_POINT('Ctrl Pts',(67.8345189347357,236.083323250929,55.503930139356));
#42356=CARTESIAN_POINT('Ctrl Pts',(69.0276716499313,235.446855222272,48.3446728820177));
#42357=CARTESIAN_POINT('Ctrl Pts',(75.7115850601304,234.810387193615,45.4799116638757));
#42358=CARTESIAN_POINT('Ctrl Pts',(80.7087378343276,234.279997169734,48.875738190411));
#42359=CARTESIAN_POINT('Ctrl Pts',(81.6436066234392,233.855685150629,53.180668089956));
#42360=CARTESIAN_POINT('Ctrl Pts',(80.5056974287515,233.431373131525,57.4364363822277));
#42361=CARTESIAN_POINT('Ctrl Pts',(75.3531715102732,232.900983107644,60.5915354783531));
#42362=CARTESIAN_POINT('Ctrl Pts',(68.8125886089893,232.264515078988,57.4131191079744));
#42363=CARTESIAN_POINT('Ctrl Pts',(67.9601893709513,231.62804705033,50.2053459832478));
#42364=CARTESIAN_POINT('Ctrl Pts',(73.5555405130985,230.991579021674,45.5825088160508));
#42365=CARTESIAN_POINT('Ctrl Pts',(80.4803812584472,230.355110993016,47.8024493476742));
#42366=CARTESIAN_POINT('Ctrl Pts',(82.0264807435618,229.824720969135,53.643061475614));
#42367=CARTESIAN_POINT('Ctrl Pts',(79.9094420644716,229.400408950031,57.5062917720994));
#42368=CARTESIAN_POINT('Ctrl Pts',(76.2596980440375,228.976096930926,59.973227052842));
#42369=CARTESIAN_POINT('Ctrl Pts',(70.3006682467896,228.445706907045,58.9766642005573));
#42370=CARTESIAN_POINT('Ctrl Pts',(67.4467211576931,227.809238878389,52.2881261445181));
#42371=CARTESIAN_POINT('Ctrl Pts',(71.5294991123255,227.172770849731,46.2873343582343));
#42372=CARTESIAN_POINT('Ctrl Pts',(78.7852974416126,226.536302821075,46.4661316001294));
#42373=CARTESIAN_POINT('Ctrl Pts',(82.5578574497902,225.899834792418,52.6829914441579));
#42374=CARTESIAN_POINT('Ctrl Pts',(79.8953068284501,225.369444768537,58.1064587746505));
#42375=CARTESIAN_POINT('Ctrl Pts',(75.7637206843553,224.945132749432,59.6349864757668));
#42376=CARTESIAN_POINT('Ctrl Pts',(71.3905354195408,224.520820730328,59.1042775958139));
#42377=CARTESIAN_POINT('Ctrl Pts',(67.5449574653074,223.990430706447,54.4443737834338));
#42378=CARTESIAN_POINT('Ctrl Pts',(69.7760950598774,223.35396267779,47.5231325790778));
#42379=CARTESIAN_POINT('Ctrl Pts',(76.7934678689953,222.717494649133,45.6697413792555));
#42380=CARTESIAN_POINT('Ctrl Pts',(82.1543340864813,222.081026620476,50.5625614860971));
#42381=CARTESIAN_POINT('Ctrl Pts',(80.9260398287832,221.444558591819,57.7300468280508));
#42382=CARTESIAN_POINT('Ctrl Pts',(75.359501788676,220.914168567939,60.0788422184516));
#42383=CARTESIAN_POINT('Ctrl Pts',(71.2378684220514,220.489856548833,58.5236805851131));
#42384=CARTESIAN_POINT('Ctrl Pts',(68.2841225777918,220.065544529729,55.2553780454862));
#42385=CARTESIAN_POINT('Ctrl Pts',(68.4363561824632,219.535154505848,49.2155095945404));
#42386=CARTESIAN_POINT('Ctrl Pts',(74.6592976343922,218.898686477191,45.4530110656439));
#42387=CARTESIAN_POINT('Ctrl Pts',(81.1727368883548,218.262218448534,48.6551890733252));
#42388=CARTESIAN_POINT('Ctrl Pts',(82.0117795796358,217.625750419878,55.8645297869897));
#42389=CARTESIAN_POINT('Ctrl Pts',(76.384577826177,216.98928239122,60.4705254569844));
#42390=CARTESIAN_POINT('Ctrl Pts',(70.6415458845036,216.45889236734,58.5937451401108));
#42391=CARTESIAN_POINT('Ctrl Pts',(68.5496937837328,216.034580348235,54.7169044211844));
#42392=CARTESIAN_POINT('Ctrl Pts',(68.4623324423871,215.61026832913,50.3125466480765));
#42393=CARTESIAN_POINT('Ctrl Pts',(72.5386807300418,215.07987830525,45.8521629591067));
#42394=CARTESIAN_POINT('Ctrl Pts',(79.7025171230519,214.443410276593,47.0922650620929));
#42395=CARTESIAN_POINT('Ctrl Pts',(82.5232975753281,213.806942247936,53.7805499308915));
#42396=CARTESIAN_POINT('Ctrl Pts',(78.4240017018063,213.170474219279,59.7744967819837));
#42397=CARTESIAN_POINT('Ctrl Pts',(71.1654941498381,212.534006190622,59.5607360970782));
#42398=CARTESIAN_POINT('Ctrl Pts',(67.4185710112033,211.897538161965,53.3437815500908));
#42399=CARTESIAN_POINT('Ctrl Pts',(70.6324017692262,211.261070133308,46.8223018905017));
#42400=CARTESIAN_POINT('Ctrl Pts',(76.6375952493495,210.730680109427,46.1520114449674));
#42401=CARTESIAN_POINT('Ctrl Pts',(80.1468768325872,210.306368090323,48.8148937493606));
#42402=CARTESIAN_POINT('Ctrl Pts',(82.0499126329196,209.882056071218,52.7878264085024));
#42403=CARTESIAN_POINT('Ctrl Pts',(80.187041012264,209.351666047337,58.5353849828742));
#42404=CARTESIAN_POINT('Ctrl Pts',(73.1513480712217,208.71519801868,60.3737594076079));
#42405=CARTESIAN_POINT('Ctrl Pts',(67.8167943497098,208.078729990023,55.4522634200252));
#42406=CARTESIAN_POINT('Ctrl Pts',(69.061584800203,207.442261961366,48.3017856987611));
#42407=CARTESIAN_POINT('Ctrl Pts',(75.7659852692241,206.805793932709,45.4853322826586));
#42408=CARTESIAN_POINT('Ctrl Pts',(80.7385115746561,206.275403908829,48.917120171924));
#42409=CARTESIAN_POINT('Ctrl Pts',(81.6422938479955,205.851091889724,53.2286852712132));
#42410=CARTESIAN_POINT('Ctrl Pts',(80.4737098842069,205.426779870619,57.4761316610172));
#42411=CARTESIAN_POINT('Ctrl Pts',(75.2985532891292,204.896389846738,60.5939738241731));
#42412=CARTESIAN_POINT('Ctrl Pts',(68.7810733356024,204.259921818082,57.3684493759649));
#42413=CARTESIAN_POINT('Ctrl Pts',(67.9807002766952,203.623453789425,50.1547139936352));
#42414=CARTESIAN_POINT('Ctrl Pts',(73.6092597236957,202.986985760768,45.5723675823186));
#42415=CARTESIAN_POINT('Ctrl Pts',(80.5179032622457,202.350517732111,47.8422132228922));
#42416=CARTESIAN_POINT('Ctrl Pts',(82.0218224346228,201.82012770823,53.6938284243281));
#42417=CARTESIAN_POINT('Ctrl Pts',(79.876965580564,201.395815689125,57.5416837167277));
#42418=CARTESIAN_POINT('Ctrl Pts',(76.2095175909059,200.971503670021,59.9822218218007));
#42419=CARTESIAN_POINT('Ctrl Pts',(70.2578331089008,200.44111364614,58.9426904260413));
#42420=CARTESIAN_POINT('Ctrl Pts',(67.4522182081061,199.804645617483,52.23373518964));
#42421=CARTESIAN_POINT('Ctrl Pts',(71.57818569271,199.168177588826,46.2625569001401));
#42422=CARTESIAN_POINT('Ctrl Pts',(78.8325051420938,198.531709560169,46.4937001791837));
#42423=CARTESIAN_POINT('Ctrl Pts',(82.5601122160283,197.895241531512,52.7376172843988));
#42424=CARTESIAN_POINT('Ctrl Pts',(79.8585005077304,197.364851507631,58.1417331066808));
#42425=CARTESIAN_POINT('Ctrl Pts',(75.7159935420101,196.940539488527,59.6404115688682));
#42426=CARTESIAN_POINT('Ctrl Pts',(71.3467511986132,196.516227469422,59.0781639035877));
#42427=CARTESIAN_POINT('Ctrl Pts',(67.5348945669068,195.985837445541,54.3906354859434));
#42428=CARTESIAN_POINT('Ctrl Pts',(69.8159110313352,195.349369416884,47.485672111573));
#42429=CARTESIAN_POINT('Ctrl Pts',(76.8464732813378,194.712901388227,45.6829596200234));
#42430=CARTESIAN_POINT('Ctrl Pts',(82.1718984779573,194.07643335957,50.6143310675762));
#42431=CARTESIAN_POINT('Ctrl Pts',(80.8919221238434,193.439965330914,57.7727677575927));
#42432=CARTESIAN_POINT('Ctrl Pts',(75.3085833923628,192.909575307032,60.0813392328799));
#42433=CARTESIAN_POINT('Ctrl Pts',(71.1982763155723,192.485263287928,58.496480618573));
#42434=CARTESIAN_POINT('Ctrl Pts',(68.2681911584664,192.060951268823,55.2069514630609));
#42435=CARTESIAN_POINT('Ctrl Pts',(68.4639919993237,191.530561244943,49.1683393975527));
#42436=CARTESIAN_POINT('Ctrl Pts',(74.7139298693017,190.894093216286,45.4508359431595));
#42437=CARTESIAN_POINT('Ctrl Pts',(81.2040747184487,190.257625187628,48.6999277725212));
#42438=CARTESIAN_POINT('Ctrl Pts',(81.9911195461561,189.621157158972,55.9151296628155));
#42439=CARTESIAN_POINT('Ctrl Pts',(76.3307548517939,188.984689130314,60.4804146307914));
#42440=CARTESIAN_POINT('Ctrl Pts',(70.6015541912865,188.454299106434,58.5622296974156));
#42441=CARTESIAN_POINT('Ctrl Pts',(68.5375189050122,188.029987087329,54.6704229923146));
#42442=CARTESIAN_POINT('Ctrl Pts',(68.48234794078,187.605675068225,50.2654987866604));
#42443=CARTESIAN_POINT('Ctrl Pts',(72.5898628211001,187.075285044344,45.8347544750419));
#42444=CARTESIAN_POINT('Ctrl Pts',(79.7462199487381,186.438817015687,47.1263070189644));
#42445=CARTESIAN_POINT('Ctrl Pts',(82.515742576707,185.80234898703,53.8351312297857));
#42446=CARTESIAN_POINT('Ctrl Pts',(78.3787509657197,185.165880958373,59.7986770113781));
#42447=CARTESIAN_POINT('Ctrl Pts',(71.1116061485101,184.529412929716,59.5337968163666));
#42448=CARTESIAN_POINT('Ctrl Pts',(68.0438817587522,183.999022905836,54.3287760944599));
#42449=CARTESIAN_POINT('Ctrl Pts',(69.0375063166156,183.574710886731,50.0370268787132));
#42450=CARTESIAN_POINT('Ctrl Pts',(71.8842836054319,183.150398867626,46.6751434540935));
#42451=CARTESIAN_POINT('Ctrl Pts',(77.8908088143546,182.620008843745,46.0233547141099));
#42452=CARTESIAN_POINT('Ctrl Pts',(82.4469328887749,181.983540815089,51.6910957747526));
#42453=CARTESIAN_POINT('Ctrl Pts',(80.1387527656007,181.347072786431,58.572293519151));
#42454=CARTESIAN_POINT('Ctrl Pts',(73.1048721785186,180.710604757775,60.3620146608933));
#42455=CARTESIAN_POINT('Ctrl Pts',(67.7918860949547,180.074136729118,55.3967619797233));
#42456=CARTESIAN_POINT('Ctrl Pts',(68.8888389242243,179.543746705237,49.4553927656997));
#42457=CARTESIAN_POINT('Ctrl Pts',(72.4532421114072,179.119434686132,46.866680535255));
#42458=CARTESIAN_POINT('Ctrl Pts',(76.8070319366311,178.695122667027,46.1951783009844));
#42459=CARTESIAN_POINT('Ctrl Pts',(81.7693387994904,178.164732643147,49.6417250141177));
#42460=CARTESIAN_POINT('Ctrl Pts',(81.4927052653565,177.52826461449,56.9084319161333));
#42461=CARTESIAN_POINT('Ctrl Pts',(75.2378426878872,176.891796585833,60.5901804158958));
#42462=CARTESIAN_POINT('Ctrl Pts',(68.7537112920353,176.255328557176,57.329104225455));
#42463=CARTESIAN_POINT('Ctrl Pts',(67.998274828751,175.618860528519,50.0964787642586));
#42464=CARTESIAN_POINT('Ctrl Pts',(72.7223922704138,175.088470504638,46.3300629555132));
#42465=CARTESIAN_POINT('Ctrl Pts',(77.1109979378639,174.664158485534,46.7128702026749));
#42466=CARTESIAN_POINT('Ctrl Pts',(80.8384205813792,174.239846466429,49.0607887552361));
#42467=CARTESIAN_POINT('Ctrl Pts',(82.324952858378,173.709456442548,54.9168450593055));
#42468=CARTESIAN_POINT('Ctrl Pts',(77.3511135899792,173.072988413891,60.2217935269295));
#42469=CARTESIAN_POINT('Ctrl Pts',(70.2144838384759,172.436520385234,58.9000168179176));
#42470=CARTESIAN_POINT('Ctrl Pts',(67.4573598306935,171.800052356578,52.1860876341802));
#42471=CARTESIAN_POINT('Ctrl Pts',(71.6296407940811,171.16358432792,46.2301135849953));
#42472=CARTESIAN_POINT('Ctrl Pts',(77.6660806668148,170.63319430404,46.4842145685839));
#42473=CARTESIAN_POINT('Ctrl Pts',(80.7284491521708,170.208882284935,49.6509637460135));
#42474=CARTESIAN_POINT('Ctrl Pts',(82.0030480812232,169.78457026583,53.8678107509346));
#42475=CARTESIAN_POINT('Ctrl Pts',(79.2853972047954,169.25418024195,59.2638785193046));
#42476=CARTESIAN_POINT('Ctrl Pts',(72.051559380782,168.617712213293,60.0076161396274));
#42477=CARTESIAN_POINT('Ctrl Pts',(67.5301482489436,167.981244184636,54.3299917019408));
#42478=CARTESIAN_POINT('Ctrl Pts',(69.8510367706492,167.344776155979,47.4530698361387));
#42479=CARTESIAN_POINT('Ctrl Pts',(76.9065957314089,166.708308127322,45.6922055417502));
#42480=CARTESIAN_POINT('Ctrl Pts',(81.297471019284,166.177918103441,49.8423125106509));
#42481=CARTESIAN_POINT('Ctrl Pts',(81.5330257953548,165.753606084336,54.2412800077259));
#42482=CARTESIAN_POINT('Ctrl Pts',(79.730240888043,165.329294065231,58.2607784429569));
#42483=CARTESIAN_POINT('Ctrl Pts',(74.1400699594029,164.798904041351,60.5527563301915));
#42484=CARTESIAN_POINT('Ctrl Pts',(68.1908518359154,164.162436012694,56.3708477908785));
#42485=CARTESIAN_POINT('Ctrl Pts',(68.5001743561956,163.525967984037,49.1194412061544));
#42486=CARTESIAN_POINT('Ctrl Pts',(74.7618279289903,162.88949995538,45.4492542336917));
#42487=CARTESIAN_POINT('Ctrl Pts',(81.2434042036485,162.253031926723,48.7463323807481));
#42488=CARTESIAN_POINT('Ctrl Pts',(81.8371631184601,161.722641902843,54.7588712785909));
#42489=CARTESIAN_POINT('Ctrl Pts',(79.1304811166209,161.298329883738,58.2345400824001));
#42490=CARTESIAN_POINT('Ctrl Pts',(75.1336863785303,160.874017864633,60.0871147541545));
#42491=CARTESIAN_POINT('Ctrl Pts',(69.4102083038376,160.343627840753,58.1519216435066));
#42492=CARTESIAN_POINT('Ctrl Pts',(67.6607577848386,159.707159812095,51.0935239362658));
#42493=CARTESIAN_POINT('Ctrl Pts',(72.6492443092724,159.070691783438,45.8215622450095));
#42494=CARTESIAN_POINT('Ctrl Pts',(79.7834200297725,158.434223754782,47.1565209213571));
#42495=CARTESIAN_POINT('Ctrl Pts',(82.5150074441991,157.797755726124,53.8959560244911));
#42496=CARTESIAN_POINT('Ctrl Pts',(79.0207050214086,157.267365702244,58.8247514376798));
#42497=CARTESIAN_POINT('Ctrl Pts',(74.6980745371252,156.843053683139,59.674025709748));
#42498=CARTESIAN_POINT('Ctrl Pts',(70.46572023205,156.418741664035,58.4519053682248));
#42499=CARTESIAN_POINT('Ctrl Pts',(67.4134691141883,155.888351640154,53.2377959753846));
#42500=CARTESIAN_POINT('Ctrl Pts',(70.7210260768666,155.251883611497,46.7615607842688));
#42501=CARTESIAN_POINT('Ctrl Pts',(77.9442921949654,154.61541558284,46.0523327069526));
#42502=CARTESIAN_POINT('Ctrl Pts',(82.4552067574609,153.978947554183,51.7383003192767));
#42503=CARTESIAN_POINT('Ctrl Pts',(80.0983132341476,153.342479525526,58.6177340337456));
#42504=CARTESIAN_POINT('Ctrl Pts',(74.2281758826995,152.812089501645,60.0476505075739));
#42505=CARTESIAN_POINT('Ctrl Pts',(70.40770839454,152.387777482541,57.8543814258676));
#42506=CARTESIAN_POINT('Ctrl Pts',(68.0136702024717,151.963465463436,54.1564114114174));
#42507=CARTESIAN_POINT('Ctrl Pts',(69.1282650058018,151.433075439555,48.2183265289509));
#42508=CARTESIAN_POINT('Ctrl Pts',(75.8721092904904,150.796607410898,45.4976428693019));
#42509=CARTESIAN_POINT('Ctrl Pts',(81.7907169371403,150.160139382241,49.6986738622307));
#42510=CARTESIAN_POINT('Ctrl Pts',(81.467998682892,149.523671353584,56.949496629814));
#42511=CARTESIAN_POINT('Ctrl Pts',(75.1775143387812,148.887203324927,60.597970561269));
#42512=CARTESIAN_POINT('Ctrl Pts',(69.8079399719556,148.356813301047,57.8283415669595));
#42513=CARTESIAN_POINT('Ctrl Pts',(68.3616844717522,147.932501281942,53.6672424187795));
#42514=CARTESIAN_POINT('Ctrl Pts',(68.9790535910217,147.508189262837,49.3054473223284));
#42515=CARTESIAN_POINT('Ctrl Pts',(73.7143370496216,146.977799238956,45.5530795080406));
#42516=CARTESIAN_POINT('Ctrl Pts',(80.589949789624,146.3413312103,47.9210965606662));
#42517=CARTESIAN_POINT('Ctrl Pts',(82.3037503541374,145.704863181643,54.9738595301416));
#42518=CARTESIAN_POINT('Ctrl Pts',(77.3055329106097,145.068395152986,60.2365964859227));
#42519=CARTESIAN_POINT('Ctrl Pts',(70.1638278773739,144.431927124329,58.8663393822131));
#42520=CARTESIAN_POINT('Ctrl Pts',(67.9259359356944,143.901537100448,53.2542975697928));
#42521=CARTESIAN_POINT('Ctrl Pts',(69.5625651603511,143.477225081343,49.1643286366771));
#42522=CARTESIAN_POINT('Ctrl Pts',(72.8888275031151,143.052913062239,46.276010800987));
#42523=CARTESIAN_POINT('Ctrl Pts',(78.9244860291356,142.522523038358,46.5480398513935));
#42524=CARTESIAN_POINT('Ctrl Pts',(82.5627811275167,141.886055009701,52.844416911982));
#42525=CARTESIAN_POINT('Ctrl Pts',(79.2320033963073,141.249586981044,59.29302122484));
#42526=CARTESIAN_POINT('Ctrl Pts',(72.0074393750885,140.613118952387,59.9889038168333));
#42527=CARTESIAN_POINT('Ctrl Pts',(67.5139863609418,139.97665092373,54.2713488042719));
#42528=CARTESIAN_POINT('Ctrl Pts',(69.5043555657909,139.446260899849,48.5668239270031));
#42529=CARTESIAN_POINT('Ctrl Pts',(73.4219126606781,139.021948880745,46.5520913141847));
#42530=CARTESIAN_POINT('Ctrl Pts',(77.8271823334845,138.59763686164,46.5525415404871));
#42531=CARTESIAN_POINT('Ctrl Pts',(82.2057117749606,138.06724683776,50.7156718023356));
#42532=CARTESIAN_POINT('Ctrl Pts',(80.8239056608555,137.430778809102,57.8551512774115));
#42533=CARTESIAN_POINT('Ctrl Pts',(74.0806480912595,136.794310780446,60.5397471927433));
#42534=CARTESIAN_POINT('Ctrl Pts',(68.1698115367609,136.157842751788,56.3277893220453));
#42535=CARTESIAN_POINT('Ctrl Pts',(68.5264259506943,135.521374723132,49.0645681721848));
#42536=CARTESIAN_POINT('Ctrl Pts',(73.769765012496,134.990984699251,46.0628071673783));
#42537=CARTESIAN_POINT('Ctrl Pts',(78.0486265721898,134.566672680146,47.1105403613868));
#42538=CARTESIAN_POINT('Ctrl Pts',(81.3742984631555,134.142360661042,49.9995380364455));
#42539=CARTESIAN_POINT('Ctrl Pts',(81.9501965609975,133.611970637161,56.0138139719088));
#42540=CARTESIAN_POINT('Ctrl Pts',(76.2253814360378,132.975502608504,60.4980136883621));
#42541=CARTESIAN_POINT('Ctrl Pts',(69.373875401297,132.339034579847,58.1031352082631));
#42542=CARTESIAN_POINT('Ctrl Pts',(67.673107048528,131.70256655119,51.0472181956595));
#42543=CARTESIAN_POINT('Ctrl Pts',(72.7050459680729,131.066098522533,45.797347147531));
#42544=CARTESIAN_POINT('Ctrl Pts',(78.6320914040458,130.535708498652,46.9692285608586));
#42545=CARTESIAN_POINT('Ctrl Pts',(81.1755929512698,130.111396479547,50.5660328330036));
#42546=CARTESIAN_POINT('Ctrl Pts',(81.7920704914035,129.687084460443,54.927954030752));
#42547=CARTESIAN_POINT('Ctrl Pts',(78.2831441745266,129.156694436562,59.8463490687415));
#42548=CARTESIAN_POINT('Ctrl Pts',(71.0205093031994,128.520226407905,59.4779877817043));
#42549=CARTESIAN_POINT('Ctrl Pts',(67.4180284889611,127.883758379248,53.1771378500223));
#42550=CARTESIAN_POINT('Ctrl Pts',(70.7607136997943,127.247290350591,46.7346978262573));
#42551=CARTESIAN_POINT('Ctrl Pts',(78.0023008142659,126.610822321934,46.0706410700047));
#42552=CARTESIAN_POINT('Ctrl Pts',(81.7087694529541,126.080432298053,50.8419368979128));
#42553=CARTESIAN_POINT('Ctrl Pts',(81.2705819659427,125.656120278949,55.2253593985487));
#42554=CARTESIAN_POINT('Ctrl Pts',(78.8757879458262,125.231808259844,58.9228399859306));
#42555=CARTESIAN_POINT('Ctrl Pts',(73.0014294075374,124.701418235964,60.3353149098227));
#42556=CARTESIAN_POINT('Ctrl Pts',(67.7597037493354,124.064950207307,55.2948915708406));
#42557=CARTESIAN_POINT('Ctrl Pts',(69.1714825404732,123.42848217865,48.1755195112118));
#42558=CARTESIAN_POINT('Ctrl Pts',(75.9196881304625,122.792014149993,45.5033856833937));
#42559=CARTESIAN_POINT('Ctrl Pts',(81.8225079909851,122.155546121336,49.7505344924449));
#42560=CARTESIAN_POINT('Ctrl Pts',(81.4922108712684,121.625156097455,55.7832848983293));
#42561=CARTESIAN_POINT('Ctrl Pts',(78.2870485036781,121.20084407835,58.805425743862));
#42562=CARTESIAN_POINT('Ctrl Pts',(74.0544444813281,120.776532059246,60.0266809517681));
#42563=CARTESIAN_POINT('Ctrl Pts',(68.6931200384709,120.246142035365,57.2411156832066));
#42564=CARTESIAN_POINT('Ctrl Pts',(68.0407764999982,119.609674006708,49.9984640127326));
#42565=CARTESIAN_POINT('Ctrl Pts',(73.7750359268359,118.973205978051,45.5490992598435));
#42566=CARTESIAN_POINT('Ctrl Pts',(80.6221059669441,118.336737949394,47.9566311380089));
#42567=CARTESIAN_POINT('Ctrl Pts',(82.2937460603617,117.700269920737,55.0338604482749));
#42568=CARTESIAN_POINT('Ctrl Pts',(78.088530493305,117.169879896857,59.3719862742016));
#42569=CARTESIAN_POINT('Ctrl Pts',(73.6869395192513,116.745567877751,59.5519806907294));
#42570=CARTESIAN_POINT('Ctrl Pts',(69.6905235374256,116.321255858647,57.6985890987921));
#42571=CARTESIAN_POINT('Ctrl Pts',(67.4693101247587,115.790865834766,52.0799251452905));
#42572=CARTESIAN_POINT('Ctrl Pts',(71.7260004416496,115.15439780611,46.1839822301925));
#42573=CARTESIAN_POINT('Ctrl Pts',(78.9729234825307,114.517929777452,46.5848367151104));
#42574=CARTESIAN_POINT('Ctrl Pts',(82.5637579476127,113.881461748796,52.8923311243753));
#42575=CARTESIAN_POINT('Ctrl Pts',(79.1851059110305,113.244993720138,59.3317616681195));
#42576=CARTESIAN_POINT('Ctrl Pts',(73.1655494534761,112.714603696258,59.849558637312));
#42577=CARTESIAN_POINT('Ctrl Pts',(69.72433240327,112.290291677153,57.099208422117));
#42578=CARTESIAN_POINT('Ctrl Pts',(67.9223691332186,111.865979658048,53.0793415752875));
#42579=CARTESIAN_POINT('Ctrl Pts',(69.9296729059342,111.335589634168,47.3807535737706));
#42580=CARTESIAN_POINT('Ctrl Pts',(77.0095966255024,110.699121605511,45.7205621880855));
#42581=CARTESIAN_POINT('Ctrl Pts',(82.2181531997852,110.062653576854,50.7752151228603));
#42582=CARTESIAN_POINT('Ctrl Pts',(80.7932244767869,109.426185548197,57.8919669109238));
#42583=CARTESIAN_POINT('Ctrl Pts',(74.0198374268243,108.78971751954,60.5382441419418));
#42584=CARTESIAN_POINT('Ctrl Pts',(69.1355541332214,108.259327495659,56.9819890393342));
#42585=CARTESIAN_POINT('Ctrl Pts',(68.3409253064168,107.835015476555,52.6489801401436));
#42586=CARTESIAN_POINT('Ctrl Pts',(69.6163861471822,107.41070345745,48.4323937558124));
#42587=CARTESIAN_POINT('Ctrl Pts',(74.8686177891412,106.880313433569,45.4462195435136));
#42588=CARTESIAN_POINT('Ctrl Pts',(81.3025753690411,106.243845404912,48.8352821236455));
#42589=CARTESIAN_POINT('Ctrl Pts',(81.9205455942097,105.607377376255,56.066927211683));
#42590=CARTESIAN_POINT('Ctrl Pts',(76.1780761879914,104.970909347598,60.5056908905895));
#42591=CARTESIAN_POINT('Ctrl Pts',(69.3289491003867,104.334441318941,58.0621251661116));
#42592=CARTESIAN_POINT('Ctrl Pts',(67.9732632547269,103.80405129506,52.1744015368241));
#42593=CARTESIAN_POINT('Ctrl Pts',(70.2145949202179,103.379739275956,48.3819309096312));
#42594=CARTESIAN_POINT('Ctrl Pts',(73.9424974086653,102.955427256851,46.0347743044002));
#42595=CARTESIAN_POINT('Ctrl Pts',(79.8660360264369,102.42503723297,47.2242548173817));
#42596=CARTESIAN_POINT('Ctrl Pts',(82.5013547012883,101.788569204314,54.0019130260837));
#42597=CARTESIAN_POINT('Ctrl Pts',(78.2259299444734,101.152101175657,59.8670064633057));
#42598=CARTESIAN_POINT('Ctrl Pts',(70.9797598094013,100.515633147,59.452764683521));
#42599=CARTESIAN_POINT('Ctrl Pts',(67.4110006732993,99.8791651183428,53.1167159510304));
#42600=CARTESIAN_POINT('Ctrl Pts',(70.2482054094664,99.3487750944619,47.7825390761917));
#42601=CARTESIAN_POINT('Ctrl Pts',(74.4272333632649,98.9244630753572,46.3889371049594));
#42602=CARTESIAN_POINT('Ctrl Pts',(78.7808858401211,98.5001510562527,47.0613292551355));
#42603=CARTESIAN_POINT('Ctrl Pts',(82.4731666214545,97.9697610323718,51.8436128392389));
#42604=CARTESIAN_POINT('Ctrl Pts',(80.0185264981547,97.333293003715,58.6887788107176));
#42605=CARTESIAN_POINT('Ctrl Pts',(72.9446871853008,96.696824975058,60.3133942281181));
#42606=CARTESIAN_POINT('Ctrl Pts',(67.7454774742435,96.0603569464011,55.249127621888));
#42607=CARTESIAN_POINT('Ctrl Pts',(69.2057968763822,95.4238889177441,48.1252928009685));
#42608=CARTESIAN_POINT('Ctrl Pts',(74.8456470784505,94.8934988938634,45.9584371654408));
#42609=CARTESIAN_POINT('Ctrl Pts',(78.9146258307725,94.4691868747586,47.6465760833042));
#42610=CARTESIAN_POINT('Ctrl Pts',(81.7607158793379,94.0448748556541,51.0090413289703));
#42611=CARTESIAN_POINT('Ctrl Pts',(81.4125019872028,93.5144848317732,57.0407840897579));
#42612=CARTESIAN_POINT('Ctrl Pts',(75.0706895264074,92.8780168031164,60.5992908024265));
#42613=CARTESIAN_POINT('Ctrl Pts',(68.6646538088411,92.2415487744594,57.1873581735787));
#42614=CARTESIAN_POINT('Ctrl Pts',(68.0600443925932,91.6050807458025,49.954583786643));
#42615=CARTESIAN_POINT('Ctrl Pts',(73.8338782107808,90.9686127171454,45.5336790882854));
#42616=CARTESIAN_POINT('Ctrl Pts',(79.5128178695483,90.4382226932647,47.5959152530032));
#42617=CARTESIAN_POINT('Ctrl Pts',(81.4779266132071,90.0139106741601,51.5385981870534));
#42618=CARTESIAN_POINT('Ctrl Pts',(81.4218552681473,89.5895986550554,55.9435110235478));
#42619=CARTESIAN_POINT('Ctrl Pts',(77.2037733255249,89.0592086311748,60.2691275544382));
#42620=CARTESIAN_POINT('Ctrl Pts',(70.0823097037432,88.4227406025177,58.7972881625044));
#42621=CARTESIAN_POINT('Ctrl Pts',(67.4830684886971,87.7862725738608,52.020672267787));
#42622=CARTESIAN_POINT('Ctrl Pts',(71.7693211340833,87.1498045452038,46.1634872665727));
#42623=CARTESIAN_POINT('Ctrl Pts',(79.0274606885328,86.5133365165468,46.6117790467127));
#42624=CARTESIAN_POINT('Ctrl Pts',(81.9627797571738,85.9829464926663,51.8926005369987));
#42625=CARTESIAN_POINT('Ctrl Pts',(80.8611049603024,85.5586344735614,56.157892289598));
#42626=CARTESIAN_POINT('Ctrl Pts',(77.9303474730929,85.134322454457,59.4468224566914));
#42627=CARTESIAN_POINT('Ctrl Pts',(71.9092796279463,84.603932430576,59.9467381007079));
#42628=CARTESIAN_POINT('Ctrl Pts',(67.4977191562266,83.9674644019192,54.1657615814364));
#42629=CARTESIAN_POINT('Ctrl Pts',(69.9789141933655,83.3309963732622,47.3450395473547));
#42630=CARTESIAN_POINT('Ctrl Pts',(77.0557427525776,82.6945283446052,45.7334951259842));
#42631=CARTESIAN_POINT('Ctrl Pts',(82.241661812508,82.0580603159484,50.8313180746414));
#42632=CARTESIAN_POINT('Ctrl Pts',(80.9950386405475,81.5276702920675,56.7430948222971));
#42633=CARTESIAN_POINT('Ctrl Pts',(77.3664066985287,81.1033582729629,59.2409801924079));
#42634=CARTESIAN_POINT('Ctrl Pts',(72.9970495209555,80.6790462538583,59.802334757404));
#42635=CARTESIAN_POINT('Ctrl Pts',(68.1233504155356,80.1486562299775,56.2315882420625));
#42636=CARTESIAN_POINT('Ctrl Pts',(68.5833807300341,79.5121882013205,48.9741832360189));
#42637=CARTESIAN_POINT('Ctrl Pts',(74.9292135124444,78.8757201726637,45.4515444273673));
#42638=CARTESIAN_POINT('Ctrl Pts',(81.3289350878523,78.2392521440066,48.875305756051));
#42639=CARTESIAN_POINT('Ctrl Pts',(81.901506270828,77.6027841153497,56.1247000447093));
#42640=CARTESIAN_POINT('Ctrl Pts',(77.0837927133066,77.0723940914689,59.7706306151759));
#42641=CARTESIAN_POINT('Ctrl Pts',(72.7062521999963,76.6480820723642,59.2771327456936));
#42642=CARTESIAN_POINT('Ctrl Pts',(69.0393031340058,76.2237700532596,56.8358450444417));
#42643=CARTESIAN_POINT('Ctrl Pts',(67.7011107449014,75.6933800293789,50.9441207826716));
#42644=CARTESIAN_POINT('Ctrl Pts',(72.8073145925882,75.0569120007219,45.7664535880871));
#42645=CARTESIAN_POINT('Ctrl Pts',(79.9082939652046,74.4204439720649,47.2680093906491));
#42646=CARTESIAN_POINT('Ctrl Pts',(82.4950116121594,73.783975943408,54.0494155644056));
#42647=CARTESIAN_POINT('Ctrl Pts',(78.1736720527292,73.1475079147511,59.8981401881259));
#42648=CARTESIAN_POINT('Ctrl Pts',(72.1455728758162,72.6171178908703,59.4916995894));
#42649=CARTESIAN_POINT('Ctrl Pts',(69.164141470346,72.1928058717657,56.2486350098195));
#42650=CARTESIAN_POINT('Ctrl Pts',(67.9964246803533,71.768493852661,52.0009487465438));
#42651=CARTESIAN_POINT('Ctrl Pts',(70.8494602565119,71.2381038287802,46.6752223502516));
#42652=CARTESIAN_POINT('Ctrl Pts',(78.0997711246432,70.6016358001233,46.1143768925114));
#42653=CARTESIAN_POINT('Ctrl Pts',(82.4763801653275,69.9651677714664,51.9043571328517));
#42654=CARTESIAN_POINT('Ctrl Pts',(79.9825887478364,69.3286997428094,58.7204837634665));
#42655=CARTESIAN_POINT('Ctrl Pts',(72.8848173646578,68.6922317141525,60.3026331572165));
#42656=CARTESIAN_POINT('Ctrl Pts',(68.6001325998369,68.1618416902717,56.0429794021445));
#42657=CARTESIAN_POINT('Ctrl Pts',(68.4757272381901,67.737529671167,51.6394666681051));
#42658=CARTESIAN_POINT('Ctrl Pts',(70.3794300405974,67.3132176520624,47.6667702622669));
#42659=CARTESIAN_POINT('Ctrl Pts',(76.0256912719453,66.7828276281816,45.5166754377604));
#42660=CARTESIAN_POINT('Ctrl Pts',(81.8674190268599,66.1463595995248,49.8474689158044));
#42661=CARTESIAN_POINT('Ctrl Pts',(81.3750964829256,65.5098915708677,57.0887530830819));
#42662=CARTESIAN_POINT('Ctrl Pts',(75.0227667999605,64.8734235422109,60.5996625774228));
#42663=CARTESIAN_POINT('Ctrl Pts',(68.6265085836188,64.2369555135538,57.1399752878129));
#42664=CARTESIAN_POINT('Ctrl Pts',(68.1847561090447,63.7065654896731,51.1143609292439));
#42665=CARTESIAN_POINT('Ctrl Pts',(70.9783360671663,63.2822534705684,47.7081442434712));
#42666=CARTESIAN_POINT('Ctrl Pts',(75.0206341615341,62.8579414514639,45.9570796503953));
#42667=CARTESIAN_POINT('Ctrl Pts',(80.6934236010896,62.327551427583,48.0361740738063));
#42668=CARTESIAN_POINT('Ctrl Pts',(82.2640911799573,61.6910833989261,55.1364950995558));
#42669=CARTESIAN_POINT('Ctrl Pts',(77.1440776652516,61.054615370269,60.2808161906002));
#42670=CARTESIAN_POINT('Ctrl Pts',(70.0458843870298,60.4181473416123,58.766144588061));
#42671=CARTESIAN_POINT('Ctrl Pts',(67.4853392181704,59.7816793129551,51.9598854282703));
#42672=CARTESIAN_POINT('Ctrl Pts',(71.1029800499966,59.2512892890746,47.1208929237402));
#42673=CARTESIAN_POINT('Ctrl Pts',(75.4456765806947,58.8269772699698,46.3810362246994));
#42674=CARTESIAN_POINT('Ctrl Pts',(79.6458228213659,58.4026652508653,47.7096342262889));
#42675=CARTESIAN_POINT('Ctrl Pts',(82.5654440617889,57.8722752269843,52.999150788269));
#42676=CARTESIAN_POINT('Ctrl Pts',(79.0954161603868,57.2358071983275,59.3898050329843));
#42677=CARTESIAN_POINT('Ctrl Pts',(71.8565449965068,56.5993391696705,59.9164188870352));
#42678=CARTESIAN_POINT('Ctrl Pts',(67.490639844384,55.9628711410137,54.1183631714356));
#42679=CARTESIAN_POINT('Ctrl Pts',(70.0204882082515,55.3264031123566,47.3006346224358));
#42680=CARTESIAN_POINT('Ctrl Pts',(75.9248594739311,54.7960130884758,46.0193955331134));
#42681=CARTESIAN_POINT('Ctrl Pts',(79.6887286312557,54.3717010693712,48.3084324614724));
#42682=CARTESIAN_POINT('Ctrl Pts',(81.9886294577527,53.9473890502666,52.0656731086939));
#42683=CARTESIAN_POINT('Ctrl Pts',(80.7244528662546,53.4169990263858,57.9737211105724));
#42684=CARTESIAN_POINT('Ctrl Pts',(73.9140612514626,52.7805309977289,60.5232546689272));
#42685=CARTESIAN_POINT('Ctrl Pts',(68.1034170573312,52.144062969072,56.1741177513611));
#42686=CARTESIAN_POINT('Ctrl Pts',(68.6091163227816,51.5075949404148,48.9337554585296));
#42687=CARTESIAN_POINT('Ctrl Pts',(74.9897193286527,50.8711269117581,45.4452800618159));
#42688=CARTESIAN_POINT('Ctrl Pts',(80.2876483184124,50.3407368878771,48.3496082227601));
#42689=CARTESIAN_POINT('Ctrl Pts',(81.6283745877845,49.9164248687726,52.5458987469576));
#42690=CARTESIAN_POINT('Ctrl Pts',(80.9010666018048,49.492112849668,56.890714529748));
#42691=CARTESIAN_POINT('Ctrl Pts',(76.0725453005356,48.9617228257872,60.5223196418405));
#42692=CARTESIAN_POINT('Ctrl Pts',(69.2589173778265,48.3252547971302,57.9814477751606));
#42693=CARTESIAN_POINT('Ctrl Pts',(67.7237461093988,47.6887867684733,50.8876598550767));
#42694=CARTESIAN_POINT('Ctrl Pts',(72.8532545152761,47.0523187398164,45.7528062648988));
#42695=CARTESIAN_POINT('Ctrl Pts',(79.9580834172726,46.4158507111594,47.3029551562518));
#42696=CARTESIAN_POINT('Ctrl Pts',(82.0535572989614,45.8854606872788,52.9697146233679));
#42697=CARTESIAN_POINT('Ctrl Pts',(80.3141778168881,45.4611486681739,57.0170545041042));
#42698=CARTESIAN_POINT('Ctrl Pts',(76.9160457242635,45.0368366490694,59.8204630319368));
#42699=CARTESIAN_POINT('Ctrl Pts',(70.8891803301883,44.5064466251886,59.3961198115476));
#42700=CARTESIAN_POINT('Ctrl Pts',(67.4110293127906,43.8699785965316,53.0098829844179));
#42701=CARTESIAN_POINT('Ctrl Pts',(70.9035728970707,43.2335105678747,46.6474371347127));
#42702=CARTESIAN_POINT('Ctrl Pts',(78.1434045755907,42.5970425392179,46.1341972831528));
#42703=CARTESIAN_POINT('Ctrl Pts',(82.4910561621044,41.9605745105607,51.9633894222313));
#42704=CARTESIAN_POINT('Ctrl Pts',(80.3572818064038,41.4301844866801,57.6158385061191));
#42705=CARTESIAN_POINT('Ctrl Pts',(76.3901015894628,41.0058724675753,59.5310100961249));
#42706=CARTESIAN_POINT('Ctrl Pts',(71.986247835856,40.5815604484709,59.419326571397));
#42707=CARTESIAN_POINT('Ctrl Pts',(67.7142338204333,40.0511704245899,55.1469654093431));
#42708=CARTESIAN_POINT('Ctrl Pts',(69.275871844425,39.4147023959331,48.0446529694379));
#42709=CARTESIAN_POINT('Ctrl Pts',(76.0847657125096,38.778234367276,45.5311808347832));
#42710=CARTESIAN_POINT('Ctrl Pts',(81.8873653875674,38.1417663386191,49.8910449255035));
#42711=CARTESIAN_POINT('Ctrl Pts',(81.3474677094592,37.5052983099622,57.1429457666064));
#42712=CARTESIAN_POINT('Ctrl Pts',(76.0300056776799,36.9749082860814,60.0113549402709));
#42713=CARTESIAN_POINT('Ctrl Pts',(71.7789637198702,36.5505962669768,58.8559141733789));
#42714=CARTESIAN_POINT('Ctrl Pts',(68.5272996093743,36.1262842478722,55.8838641056007));
#42715=CARTESIAN_POINT('Ctrl Pts',(68.1034461174788,35.5958942239914,49.8569642504253));
#42716=CARTESIAN_POINT('Ctrl Pts',(73.9396624076152,34.9594261953344,45.5187463297918));
#42717=CARTESIAN_POINT('Ctrl Pts',(80.7285130577238,34.3229581666775,48.0858623632235));
#42718=CARTESIAN_POINT('Ctrl Pts',(82.2505766296694,33.6864901380205,55.1824742562947));
#42719=CARTESIAN_POINT('Ctrl Pts',(77.0876823646044,33.0500221093636,60.3036145708011));
#42720=CARTESIAN_POINT('Ctrl Pts',(71.1921167813803,32.5196320854828,58.9824483810628));
#42721=CARTESIAN_POINT('Ctrl Pts',(68.7402458099335,32.0953200663781,55.3225672585752));
#42722=CARTESIAN_POINT('Ctrl Pts',(68.2341037132805,31.6710080472735,50.946470678878));
#42723=CARTESIAN_POINT('Ctrl Pts',(71.8661011659931,31.1406180233927,46.1182444891829));
#42724=CARTESIAN_POINT('Ctrl Pts',(79.1171193063283,30.5041499947358,46.6698704896195));
#42725=CARTESIAN_POINT('Ctrl Pts',(82.5593545172997,29.8676819660789,53.0596744512932));
#42726=CARTESIAN_POINT('Ctrl Pts',(79.0550629000917,29.231213937422,59.4156573061479));
#42727=CARTESIAN_POINT('Ctrl Pts',(71.7990171583499,28.5947459087649,59.8966516467535));
#42728=CARTESIAN_POINT('Ctrl Pts',(68.2142059078879,28.0643558848842,55.0332883940346));
#42729=CARTESIAN_POINT('Ctrl Pts',(68.7629354775493,27.6400438657795,50.6623277839382));
#42730=CARTESIAN_POINT('Ctrl Pts',(71.2503276753517,27.215731846675,47.0264947721512));
#42731=CARTESIAN_POINT('Ctrl Pts',(77.1584783503202,26.6853418227941,45.7627984010655));
#42732=CARTESIAN_POINT('Ctrl Pts',(82.2712616960307,26.0488737941373,50.9339684465705));
#42733=CARTESIAN_POINT('Ctrl Pts',(80.6801681651456,25.4124057654802,58.0154235336963));
#42734=CARTESIAN_POINT('Ctrl Pts',(73.866642710383,24.7759377368233,60.5163117476636));
#42735=CARTESIAN_POINT('Ctrl Pts',(68.0729453817716,24.1394697081664,56.12147205692));
#42736=CARTESIAN_POINT('Ctrl Pts',(68.5554653314807,23.6090796842856,50.0989820315547));
#42737=CARTESIAN_POINT('Ctrl Pts',(71.8359141101355,23.1847676651809,47.1587399770951));
#42738=CARTESIAN_POINT('Ctrl Pts',(76.0980073818475,22.7604556460764,46.044738731972));
#42739=CARTESIAN_POINT('Ctrl Pts',(81.3872823714418,22.2300656221955,48.9648097787581));
#42740=CARTESIAN_POINT('Ctrl Pts',(81.8565481913765,21.5935975935386,56.2215875539192));
#42741=CARTESIAN_POINT('Ctrl Pts',(76.0117562751922,20.9571295648817,60.5248076967008));
#42742=CARTESIAN_POINT('Ctrl Pts',(69.2276857397562,20.3206615362247,57.9450335920459));
#42743=CARTESIAN_POINT('Ctrl Pts',(67.7352284395576,19.6841935075678,50.8280874080433));
#42744=CARTESIAN_POINT('Ctrl Pts',(72.0487341561334,19.153803483687,46.5970962084509));
#42745=CARTESIAN_POINT('Ctrl Pts',(76.4533287195552,18.7294914645823,46.5289391655419));
#42746=CARTESIAN_POINT('Ctrl Pts',(80.4019430431638,18.3051794454777,48.481393986882));
#42747=CARTESIAN_POINT('Ctrl Pts',(82.479976533845,17.7747894215969,54.1571331492716));
#42748=CARTESIAN_POINT('Ctrl Pts',(78.0768644284893,17.13832139294,59.9386486421499));
#42749=CARTESIAN_POINT('Ctrl Pts',(70.8404208569049,16.5018533642831,59.3639367716877));
#42750=CARTESIAN_POINT('Ctrl Pts',(67.4137579998166,15.8653853356261,52.9507745892659));
#42751=CARTESIAN_POINT('Ctrl Pts',(70.3570038465839,15.3349953117452,47.6862554085638));
#42752=CARTESIAN_POINT('Ctrl Pts',(74.5788989575806,14.9106832926407,46.370762759139));
#42753=CARTESIAN_POINT('Ctrl Pts',(76.7327422243518,14.6985272830883,46.7693660572235));
#42754=CARTESIAN_POINT('Ctrl Pts',(77.6994510401983,14.5924492783122,47.2211751965707));
#42755=CARTESIAN_POINT('Ctrl Pts',(70.0990315389037,416.,55.841954369316));
#42756=CARTESIAN_POINT('Ctrl Pts',(69.6292862985721,415.893921995224,55.0273288624995));
#42757=CARTESIAN_POINT('Ctrl Pts',(69.1165406058533,415.681765985672,53.1663787797211));
#42758=CARTESIAN_POINT('Ctrl Pts',(69.9524819678234,415.257453966567,49.3601406988557));
#42759=CARTESIAN_POINT('Ctrl Pts',(74.352298526842,414.727063942686,46.3781169629522));
#42760=CARTESIAN_POINT('Ctrl Pts',(80.2420155782074,414.090595914029,48.9020647204953));
#42761=CARTESIAN_POINT('Ctrl Pts',(81.293491257306,413.454127885372,55.2122271685484));
#42762=CARTESIAN_POINT('Ctrl Pts',(76.5500783965337,412.817659856716,59.5150838971706));
#42763=CARTESIAN_POINT('Ctrl Pts',(71.4097383128725,412.287269832834,58.1195031021403));
#42764=CARTESIAN_POINT('Ctrl Pts',(69.397075484847,411.86295781373,54.8001736486049));
#42765=CARTESIAN_POINT('Ctrl Pts',(69.1240494715453,411.438645794625,50.9277902465141));
#42766=CARTESIAN_POINT('Ctrl Pts',(72.5128743250655,410.908255770745,46.8207854764477));
#42767=CARTESIAN_POINT('Ctrl Pts',(78.8743400235446,410.271787742087,47.5933144106201));
#42768=CARTESIAN_POINT('Ctrl Pts',(81.6520725540428,409.635319713431,53.3547651639986));
#42769=CARTESIAN_POINT('Ctrl Pts',(78.3155544127733,408.998851684773,58.8116972627153));
#42770=CARTESIAN_POINT('Ctrl Pts',(71.90864214512,408.362383656117,58.9480975871434));
#42771=CARTESIAN_POINT('Ctrl Pts',(68.9450950083279,407.831993632236,54.524794049794));
#42772=CARTESIAN_POINT('Ctrl Pts',(69.6010890929968,407.407681613131,50.6984892817582));
#42773=CARTESIAN_POINT('Ctrl Pts',(71.9347077043872,406.983369594027,47.5960537873647));
#42774=CARTESIAN_POINT('Ctrl Pts',(77.1859865465286,406.452979570146,46.7172645440322));
#42775=CARTESIAN_POINT('Ctrl Pts',(81.4825007141912,405.816511541489,51.4719982227287));
#42776=CARTESIAN_POINT('Ctrl Pts',(79.8016393924563,405.180043512832,57.643270644141));
#42777=CARTESIAN_POINT('Ctrl Pts',(73.704367667017,404.543575484175,59.575416161524));
#42778=CARTESIAN_POINT('Ctrl Pts',(68.7776943304863,403.907107455519,55.477194252816));
#42779=CARTESIAN_POINT('Ctrl Pts',(69.4407233960758,403.376717431636,50.194338734914));
#42780=CARTESIAN_POINT('Ctrl Pts',(72.4450042051697,402.952405412533,47.7356388492427));
#42781=CARTESIAN_POINT('Ctrl Pts',(76.2412371124112,402.528093393428,46.9235284074953));
#42782=CARTESIAN_POINT('Ctrl Pts',(80.7821829418601,401.997703369548,49.7034531632788));
#42783=CARTESIAN_POINT('Ctrl Pts',(80.9082303071252,401.36123534089,56.1106090638576));
#42784=CARTESIAN_POINT('Ctrl Pts',(75.5925088429904,400.724767312234,59.6677158495928));
#42785=CARTESIAN_POINT('Ctrl Pts',(69.7221234542071,400.088299283577,57.1283303225627));
#42786=CARTESIAN_POINT('Ctrl Pts',(68.6898157193372,399.451831254919,50.8036267423682));
#42787=CARTESIAN_POINT('Ctrl Pts',(72.6545162366563,398.921441231039,47.2498512386062));
#42788=CARTESIAN_POINT('Ctrl Pts',(76.5349782081459,398.497129211934,47.3635296330406));
#42789=CARTESIAN_POINT('Ctrl Pts',(79.9336475688305,398.072817192829,49.2396838010189));
#42790=CARTESIAN_POINT('Ctrl Pts',(81.5391758901464,397.542427168949,54.31614411719));
#42791=CARTESIAN_POINT('Ctrl Pts',(77.4329911410624,396.905959140291,59.2361828813744));
#42792=CARTESIAN_POINT('Ctrl Pts',(71.0871415122597,396.269491111636,58.436122929515));
#42793=CARTESIAN_POINT('Ctrl Pts',(68.3201615171243,395.633023082977,52.6695186301911));
#42794=CARTESIAN_POINT('Ctrl Pts',(71.6880557805561,394.996555054321,47.2174710456321));
#42795=CARTESIAN_POINT('Ctrl Pts',(77.0117036986669,394.46616503044,47.1341441224853));
#42796=CARTESIAN_POINT('Ctrl Pts',(79.8669002864431,394.041853011336,49.7644977739172));
#42797=CARTESIAN_POINT('Ctrl Pts',(81.2026403625402,393.617540992231,53.409591234385));
#42798=CARTESIAN_POINT('Ctrl Pts',(79.0860339449119,393.087150968349,58.2950950779045));
#42799=CARTESIAN_POINT('Ctrl Pts',(72.7596690106956,392.450682939694,59.3171720578613));
#42800=CARTESIAN_POINT('Ctrl Pts',(68.4931906324375,391.814214911036,54.5519789152622));
#42801=CARTESIAN_POINT('Ctrl Pts',(70.1854506547193,391.177746882379,48.3838220223643));
#42802=CARTESIAN_POINT('Ctrl Pts',(76.3032611663828,390.541278853722,46.4759621802336));
#42803=CARTESIAN_POINT('Ctrl Pts',(80.3772412432425,390.010888829841,49.9039144648412));
#42804=CARTESIAN_POINT('Ctrl Pts',(80.8081112306684,389.586576810737,53.7620563674119));
#42805=CARTESIAN_POINT('Ctrl Pts',(79.4264024191887,389.162264791632,57.3899743166933));
#42806=CARTESIAN_POINT('Ctrl Pts',(74.6248094448821,388.631874767752,59.6905993277034));
#42807=CARTESIAN_POINT('Ctrl Pts',(69.1782161333895,387.995406739095,56.3138914734408));
#42808=CARTESIAN_POINT('Ctrl Pts',(69.0817056595131,387.358938710438,49.9185346290693));
#42809=CARTESIAN_POINT('Ctrl Pts',(74.4039894636263,386.72247068178,46.3712541852796));
#42810=CARTESIAN_POINT('Ctrl Pts',(80.2739571702038,386.086002653124,48.9424433571557));
#42811=CARTESIAN_POINT('Ctrl Pts',(81.1019979235157,385.555612629243,54.201960354281));
#42812=CARTESIAN_POINT('Ctrl Pts',(78.897412769893,385.131300610139,57.3973808566349));
#42813=CARTESIAN_POINT('Ctrl Pts',(75.4752995936722,384.706988591033,59.2304245810384));
#42814=CARTESIAN_POINT('Ctrl Pts',(70.3415256590186,384.176598567153,57.8188525070491));
#42815=CARTESIAN_POINT('Ctrl Pts',(68.4435630952913,383.540130538496,51.6979642757119));
#42816=CARTESIAN_POINT('Ctrl Pts',(72.5643111612702,382.903662509839,46.8062019332478));
#42817=CARTESIAN_POINT('Ctrl Pts',(78.9086719290272,382.267194481182,47.6179838540664));
#42818=CARTESIAN_POINT('Ctrl Pts',(81.65448204411,381.630726452525,53.4083259377208));
#42819=CARTESIAN_POINT('Ctrl Pts',(78.8308391867579,381.100336428644,57.9222168919113));
#42820=CARTESIAN_POINT('Ctrl Pts',(75.0710571136364,380.67602440954,58.8891432847));
#42821=CARTESIAN_POINT('Ctrl Pts',(71.2853928743543,380.251712390435,58.0291118004746));
#42822=CARTESIAN_POINT('Ctrl Pts',(68.3350139784818,379.721322366554,53.5970203186811));
#42823=CARTESIAN_POINT('Ctrl Pts',(70.9156937160722,379.084854337897,47.7312188622881));
#42824=CARTESIAN_POINT('Ctrl Pts',(77.2345122810668,378.448386309241,46.7400400786665));
#42825=CARTESIAN_POINT('Ctrl Pts',(81.4921801522575,377.811918280583,51.5131069896837));
#42826=CARTESIAN_POINT('Ctrl Pts',(79.7683714008492,377.175450251926,57.6853041691651));
#42827=CARTESIAN_POINT('Ctrl Pts',(74.676644657417,376.645060228046,59.2417389742301));
#42828=CARTESIAN_POINT('Ctrl Pts',(71.2039784868037,376.220748208941,57.5063722827453));
#42829=CARTESIAN_POINT('Ctrl Pts',(68.9097584028537,375.796436189837,54.3746855019773));
#42830=CARTESIAN_POINT('Ctrl Pts',(69.5884755901131,375.266046165955,49.0938225505349));
#42831=CARTESIAN_POINT('Ctrl Pts',(75.3832511001032,374.629578137299,46.3573811711787));
#42832=CARTESIAN_POINT('Ctrl Pts',(80.8038861164523,373.993110108642,49.7524687190848));
#42833=CARTESIAN_POINT('Ctrl Pts',(80.8885816316862,373.356642079985,56.1479929437374));
#42834=CARTESIAN_POINT('Ctrl Pts',(75.5398292911409,372.720174051328,59.677636414875));
#42835=CARTESIAN_POINT('Ctrl Pts',(70.6749913177946,372.189784027447,57.5139538999746));
#42836=CARTESIAN_POINT('Ctrl Pts',(69.1910655822406,371.765472008342,53.9266328524801));
#42837=CARTESIAN_POINT('Ctrl Pts',(69.5124694584528,371.341159989238,50.0578336285873));
#42838=CARTESIAN_POINT('Ctrl Pts',(73.4877077677736,370.810769965357,46.5158495918775));
#42839=CARTESIAN_POINT('Ctrl Pts',(79.6571088321875,370.1743019367,48.2496388351935));
#42840=CARTESIAN_POINT('Ctrl Pts',(81.5234208748353,369.537833908044,54.367382111753));
#42841=CARTESIAN_POINT('Ctrl Pts',(77.3936427899844,368.901365879386,59.2515234291501));
#42842=CARTESIAN_POINT('Ctrl Pts',(71.0408633993679,368.26489785073,58.4090694850156));
#42843=CARTESIAN_POINT('Ctrl Pts',(68.7867101717712,367.734507826848,53.5854853654303));
#42844=CARTESIAN_POINT('Ctrl Pts',(70.0186562199422,367.310195807744,49.904015982041));
#42845=CARTESIAN_POINT('Ctrl Pts',(72.7981944809444,366.885883788639,47.1938361094012));
#42846=CARTESIAN_POINT('Ctrl Pts',(78.1220664110398,366.355493764758,47.126321635835));
#42847=CARTESIAN_POINT('Ctrl Pts',(81.643054336671,365.719025736102,52.4807757313887));
#42848=CARTESIAN_POINT('Ctrl Pts',(79.0405407724415,365.082557707444,58.3234486288234));
#42849=CARTESIAN_POINT('Ctrl Pts',(72.7199018846829,364.446089678788,59.302952324055));
#42850=CARTESIAN_POINT('Ctrl Pts',(68.4759904733059,363.809621650131,54.5012077904277));
#42851=CARTESIAN_POINT('Ctrl Pts',(69.9370688277395,363.279231626249,49.3813034383522));
#42852=CARTESIAN_POINT('Ctrl Pts',(73.2812266717887,362.854919607146,47.4096249147279));
#42853=CARTESIAN_POINT('Ctrl Pts',(77.1569110752008,362.43060758804,47.1860666637397));
#42854=CARTESIAN_POINT('Ctrl Pts',(81.2206916178702,361.90021756416,50.6261041974329));
#42855=CARTESIAN_POINT('Ctrl Pts',(80.3679639602247,361.263749535503,56.9775127164719));
#42856=CARTESIAN_POINT('Ctrl Pts',(74.5718700069468,360.627281506846,59.6821750471879));
#42857=CARTESIAN_POINT('Ctrl Pts',(69.1575163315875,359.990813478189,56.2770792017615));
#42858=CARTESIAN_POINT('Ctrl Pts',(69.1020116217968,359.354345449532,49.8689239398295));
#42859=CARTESIAN_POINT('Ctrl Pts',(73.5623855454864,358.823955425652,46.9614791866025));
#42860=CARTESIAN_POINT('Ctrl Pts',(77.3801004030129,358.399643406547,47.665724281053));
#42861=CARTESIAN_POINT('Ctrl Pts',(80.4528253805887,357.975331387442,50.0383323604923));
#42862=CARTESIAN_POINT('Ctrl Pts',(81.2652408784827,357.444941363561,55.3002855711336));
#42863=CARTESIAN_POINT('Ctrl Pts',(76.4566386365349,356.808473334904,59.5364252185682));
#42864=CARTESIAN_POINT('Ctrl Pts',(70.3070805562703,356.172005306247,57.777778336482));
#42865=CARTESIAN_POINT('Ctrl Pts',(68.4520736285264,355.53553727759,51.6565976712477));
#42866=CARTESIAN_POINT('Ctrl Pts',(72.6121732175607,354.899069248933,46.7820611760358));
#42867=CARTESIAN_POINT('Ctrl Pts',(77.886236228337,354.368679225053,47.5117391122231));
#42868=CARTESIAN_POINT('Ctrl Pts',(80.3068079108729,353.944367205948,50.5468240560329));
#42869=CARTESIAN_POINT('Ctrl Pts',(81.0709222002272,353.520055186843,54.3530081345088));
#42870=CARTESIAN_POINT('Ctrl Pts',(78.2338848228655,352.989665162963,58.858492509318));
#42871=CARTESIAN_POINT('Ctrl Pts',(71.8256481706415,352.353197134305,58.9036327676611));
#42872=CARTESIAN_POINT('Ctrl Pts',(68.3359414908884,351.716729105649,53.5434228158304));
#42873=CARTESIAN_POINT('Ctrl Pts',(70.9492443786796,351.080261076991,47.7055677769413));
#42874=CARTESIAN_POINT('Ctrl Pts',(77.2864777741945,350.443793048335,46.7531983504033));
#42875=CARTESIAN_POINT('Ctrl Pts',(80.7899114940622,349.913403024454,50.7624529822129));
#42876=CARTESIAN_POINT('Ctrl Pts',(80.6272472545832,349.48909100535,54.6411703258245));
#42877=CARTESIAN_POINT('Ctrl Pts',(78.7083308692968,349.064778986245,58.0158803567333));
#42878=CARTESIAN_POINT('Ctrl Pts',(73.6120037259175,348.534388962364,59.557185057255));
#42879=CARTESIAN_POINT('Ctrl Pts',(68.7442020401091,347.897920933707,55.3892069645249));
#42880=CARTESIAN_POINT('Ctrl Pts',(69.6243212317588,347.26145290505,49.0539647712928));
#42881=CARTESIAN_POINT('Ctrl Pts',(75.4254018924481,346.624984876393,46.3600147705323));
#42882=CARTESIAN_POINT('Ctrl Pts',(80.8344916837998,345.988516847736,49.7964783980026));
#42883=CARTESIAN_POINT('Ctrl Pts',(80.8505953206296,345.458126823855,55.1207540487439));
#42884=CARTESIAN_POINT('Ctrl Pts',(78.1844014847269,345.033814804751,57.942512067397));
#42885=CARTESIAN_POINT('Ctrl Pts',(74.5227334601851,344.609502785646,59.2321225374558));
#42886=CARTESIAN_POINT('Ctrl Pts',(69.664343426917,344.079112761766,57.0540002229753));
#42887=CARTESIAN_POINT('Ctrl Pts',(68.7222249177504,343.442644733109,50.7152347794114));
#42888=CARTESIAN_POINT('Ctrl Pts',(73.540906987327,342.806176704451,46.5092620559193));
#42889=CARTESIAN_POINT('Ctrl Pts',(79.6872056462168,342.169708675795,48.279266641831));
#42890=CARTESIAN_POINT('Ctrl Pts',(81.5176696288029,341.533240647137,54.4206782256844));
#42891=CARTESIAN_POINT('Ctrl Pts',(78.0385523165719,341.002850623257,58.4510520619348));
#42892=CARTESIAN_POINT('Ctrl Pts',(74.1752777672687,340.578538604152,58.8331746118364));
#42893=CARTESIAN_POINT('Ctrl Pts',(70.5650945300378,340.154226585048,57.4057696657705));
#42894=CARTESIAN_POINT('Ctrl Pts',(68.3252780582827,339.623836561167,52.5755116286618));
#42895=CARTESIAN_POINT('Ctrl Pts',(71.7704857081252,338.98736853251,47.1719869564409));
#42896=CARTESIAN_POINT('Ctrl Pts',(78.1665513135014,338.350900503852,47.1562322701325));
#42897=CARTESIAN_POINT('Ctrl Pts',(81.6463495765641,337.714432475197,52.522879965557));
#42898=CARTESIAN_POINT('Ctrl Pts',(79.0012508535765,337.077964446539,58.3599158040183));
#42899=CARTESIAN_POINT('Ctrl Pts',(73.7316982178695,336.547574422658,59.1214836287799));
#42900=CARTESIAN_POINT('Ctrl Pts',(70.5643676301849,336.123262403554,56.8767286678197));
#42901=CARTESIAN_POINT('Ctrl Pts',(68.7746777925706,335.698950384449,53.4317441727057));
#42902=CARTESIAN_POINT('Ctrl Pts',(70.2509566334843,335.168560360568,48.3162020395523));
#42903=CARTESIAN_POINT('Ctrl Pts',(76.3953207281506,334.532092331911,46.4956734058825));
#42904=CARTESIAN_POINT('Ctrl Pts',(81.2346643690577,333.895624303255,50.6778566352051));
#42905=CARTESIAN_POINT('Ctrl Pts',(80.3428429412503,333.259156274597,57.0114620838672));
#42906=CARTESIAN_POINT('Ctrl Pts',(74.5182936803783,332.622688245941,59.6839441776349));
#42907=CARTESIAN_POINT('Ctrl Pts',(70.0404139918865,332.09229822206,56.8035337854184));
#42908=CARTESIAN_POINT('Ctrl Pts',(69.1210358704998,331.667986202955,53.0318429502156));
#42909=CARTESIAN_POINT('Ctrl Pts',(70.0287967856483,331.24367418385,49.257339273258));
#42910=CARTESIAN_POINT('Ctrl Pts',(74.4977866088157,330.71328415997,46.3631553653794));
#42911=CARTESIAN_POINT('Ctrl Pts',(80.3305367008356,330.076816131312,49.0176912942896));
#42912=CARTESIAN_POINT('Ctrl Pts',(81.2418547574505,329.440348102656,55.3485208479978));
#42913=CARTESIAN_POINT('Ctrl Pts',(76.4154107889894,328.803880073999,59.5455843521308));
#42914=CARTESIAN_POINT('Ctrl Pts',(70.265470501402,328.167412045342,57.7439825390367));
#42915=CARTESIAN_POINT('Ctrl Pts',(68.7734481583349,327.637022021461,52.6330100425361));
#42916=CARTESIAN_POINT('Ctrl Pts',(70.5525225770171,327.212710002356,49.182531510618));
#42917=CARTESIAN_POINT('Ctrl Pts',(73.7129266627949,326.788397983251,46.9280351364722));
#42918=CARTESIAN_POINT('Ctrl Pts',(78.984799150373,326.258007959371,47.6733746610617));
#42919=CARTESIAN_POINT('Ctrl Pts',(81.6478572785503,325.621539930714,53.5022387047481));
#42920=CARTESIAN_POINT('Ctrl Pts',(78.1845991508713,324.985071902057,58.8795750880781));
#42921=CARTESIAN_POINT('Ctrl Pts',(71.7885153548133,324.3486038734,58.8835136441829));
#42922=CARTESIAN_POINT('Ctrl Pts',(68.3266868515903,323.712135844743,53.4906222074762));
#42923=CARTESIAN_POINT('Ctrl Pts',(70.5516205825161,323.181745820863,48.6534907822217));
#42924=CARTESIAN_POINT('Ctrl Pts',(74.1573917987538,322.757433801757,47.2149770274767));
#42925=CARTESIAN_POINT('Ctrl Pts',(78.0218245725355,322.333121782654,47.5852029360215));
#42926=CARTESIAN_POINT('Ctrl Pts',(81.5133347143192,321.802731758772,51.6048456392999));
#42927=CARTESIAN_POINT('Ctrl Pts',(79.7017885087686,321.166263730116,57.7518640205145));
#42928=CARTESIAN_POINT('Ctrl Pts',(73.5609687392484,320.529795701458,59.5407843643785));
#42929=CARTESIAN_POINT('Ctrl Pts',(68.7293595293914,319.893327672802,55.3496680594258));
#42930=CARTESIAN_POINT('Ctrl Pts',(69.6519568295469,319.256859644144,49.0080319254632));
#42931=CARTESIAN_POINT('Ctrl Pts',(74.5036175039259,318.726469620264,46.8149611940725));
#42932=CARTESIAN_POINT('Ctrl Pts',(78.1692388187073,318.302157601159,48.0932914577593));
#42933=CARTESIAN_POINT('Ctrl Pts',(80.8441080694396,317.877845582055,50.9068270231865));
#42934=CARTESIAN_POINT('Ctrl Pts',(80.8443976887383,317.347455558173,56.2311270192722));
#42935=CARTESIAN_POINT('Ctrl Pts',(75.4459142368694,316.710987529517,59.6842286762946));
#42936=CARTESIAN_POINT('Ctrl Pts',(69.6365665351741,316.07451950086,57.0081526834969));
#42937=CARTESIAN_POINT('Ctrl Pts',(68.7369456197939,315.438051472203,50.6756503623739));
#42938=CARTESIAN_POINT('Ctrl Pts',(73.5918912351737,314.801583443546,46.4927043065974));
#42939=CARTESIAN_POINT('Ctrl Pts',(78.6929398225512,314.271193419665,48.0183103636822));
#42940=CARTESIAN_POINT('Ctrl Pts',(80.6222376764774,313.846881400561,51.3870961504713));
#42941=CARTESIAN_POINT('Ctrl Pts',(80.7968435226311,313.422569381455,55.2652942739464));
#42942=CARTESIAN_POINT('Ctrl Pts',(77.3057707044781,312.892179357576,59.2853168000712));
#42943=CARTESIAN_POINT('Ctrl Pts',(70.9656350492383,312.255711328918,58.3524639140331));
#42944=CARTESIAN_POINT('Ctrl Pts',(68.3343700832684,311.619243300261,52.5226827760076));
#42945=CARTESIAN_POINT('Ctrl Pts',(71.8075564021643,310.982775271605,47.1517535982347));
#42946=CARTESIAN_POINT('Ctrl Pts',(78.2159016640937,310.346307242947,47.1771630008298));
#42947=CARTESIAN_POINT('Ctrl Pts',(81.0667977561599,309.815917219067,51.6738909228237));
#42948=CARTESIAN_POINT('Ctrl Pts',(80.3144061400767,309.391605199962,55.4824096299437));
#42949=CARTESIAN_POINT('Ctrl Pts',(77.9031908065171,308.967293180857,58.5249330072815));
#42950=CARTESIAN_POINT('Ctrl Pts',(72.6313994367438,308.436903156976,59.2708460623881));
#42951=CARTESIAN_POINT('Ctrl Pts',(68.456311111176,307.80043512832,54.4091414120066));
#42952=CARTESIAN_POINT('Ctrl Pts',(70.2924624355432,307.163967099663,48.28227828701));
#42953=CARTESIAN_POINT('Ctrl Pts',(76.4365765807934,306.527499071006,46.5047055575397));
#42954=CARTESIAN_POINT('Ctrl Pts',(81.2581988932575,305.891031042348,50.7260196787322));
#42955=CARTESIAN_POINT('Ctrl Pts',(80.4619885383012,305.360641018468,55.9904493347213));
#42956=CARTESIAN_POINT('Ctrl Pts',(77.3965832675933,304.936328999363,58.372506935359));
#42957=CARTESIAN_POINT('Ctrl Pts',(73.5810548415566,304.512016980259,59.0885032457832));
#42958=CARTESIAN_POINT('Ctrl Pts',(69.1117501822202,303.981626956378,56.1948055431484));
#42959=CARTESIAN_POINT('Ctrl Pts',(69.1475242377325,303.345158927721,49.7865097594955));
#42960=CARTESIAN_POINT('Ctrl Pts',(74.551368128498,302.708690899064,46.3647595285971));
#42961=CARTESIAN_POINT('Ctrl Pts',(80.3557621291498,302.072222870407,49.0515631543982));
#42962=CARTESIAN_POINT('Ctrl Pts',(81.2280414156741,301.435754841751,55.4003160618702));
#42963=CARTESIAN_POINT('Ctrl Pts',(77.1748718396303,300.905364817869,58.8528494679402));
#42964=CARTESIAN_POINT('Ctrl Pts',(73.2985174821482,300.481052798765,58.6412253160407));
#42965=CARTESIAN_POINT('Ctrl Pts',(69.9483047892701,300.05674077966,56.6798526337298));
#42966=CARTESIAN_POINT('Ctrl Pts',(68.4714694295786,299.526350755779,51.5644711374421));
#42967=CARTESIAN_POINT('Ctrl Pts',(72.700576392418,298.889882727122,46.7496825719188));
#42968=CARTESIAN_POINT('Ctrl Pts',(79.0242011636225,298.253414698465,47.7097206916977));
#42969=CARTESIAN_POINT('Ctrl Pts',(81.6446916911186,297.616946669809,53.544352885223));
#42970=CARTESIAN_POINT('Ctrl Pts',(78.1402065526217,296.980478641151,58.909622547401));
#42971=CARTESIAN_POINT('Ctrl Pts',(72.8161519838604,296.450088617271,58.8585003306135));
#42972=CARTESIAN_POINT('Ctrl Pts',(70.0282823888382,296.025776598166,56.1568913641665));
#42973=CARTESIAN_POINT('Ctrl Pts',(68.7850071190202,295.601464579061,52.4792325314445));
#42974=CARTESIAN_POINT('Ctrl Pts',(71.0242980864921,295.071074555181,47.6487308499217));
#42975=CARTESIAN_POINT('Ctrl Pts',(77.3744534912965,294.434606526524,46.7867210073652));
#42976=CARTESIAN_POINT('Ctrl Pts',(81.5192500291734,293.798138497867,51.6581237928087));
#42977=CARTESIAN_POINT('Ctrl Pts',(79.6717830599399,293.16167046921,57.7815843533094));
#42978=CARTESIAN_POINT('Ctrl Pts',(73.5077494891626,292.525202440553,59.5343606573951));
#42979=CARTESIAN_POINT('Ctrl Pts',(69.5216244297834,291.994812416672,56.0046329705635));
#42980=CARTESIAN_POINT('Ctrl Pts',(69.188310236716,291.570500397568,52.1368416712381));
#42981=CARTESIAN_POINT('Ctrl Pts',(70.6611837554908,291.146188378463,48.5449686940674));
#42982=CARTESIAN_POINT('Ctrl Pts',(75.519336798809,290.615798354582,46.3663178409258));
#42983=CARTESIAN_POINT('Ctrl Pts',(80.8789313829989,289.979330325925,49.8794760393219));
#42984=CARTESIAN_POINT('Ctrl Pts',(80.8139277700718,289.342862297268,56.2752307226039));
#42985=CARTESIAN_POINT('Ctrl Pts',(75.4037717530398,288.706394268611,59.6869920433574));
#42986=CARTESIAN_POINT('Ctrl Pts',(69.6005983433171,288.069926239955,56.9684054601267));
#42987=CARTESIAN_POINT('Ctrl Pts',(68.9056248589062,287.539536216073,51.6896572763087));
#42988=CARTESIAN_POINT('Ctrl Pts',(71.1901917605342,287.115224196969,48.5509215501885));
#42989=CARTESIAN_POINT('Ctrl Pts',(74.6574983630918,286.690912177864,46.8048709179623));
#42990=CARTESIAN_POINT('Ctrl Pts',(79.7539931571663,286.160522153983,48.3456211722762));
#42991=CARTESIAN_POINT('Ctrl Pts',(81.496797625751,285.524054125327,54.5124815743055));
#42992=CARTESIAN_POINT('Ctrl Pts',(77.2538459713296,284.887586096669,59.2986350086054));
#42993=CARTESIAN_POINT('Ctrl Pts',(70.9320055672451,284.251118068013,58.3269162510927));
#42994=CARTESIAN_POINT('Ctrl Pts',(68.3332775512137,283.614650039355,52.4690883829723));
#42995=CARTESIAN_POINT('Ctrl Pts',(71.2699962732185,283.084260015475,48.0279338393853));
#42996=CARTESIAN_POINT('Ctrl Pts',(75.0529945743877,282.65994799637,47.1562505598691));
#42997=CARTESIAN_POINT('Ctrl Pts',(78.8157359444728,282.235635977266,48.1115961875279));
#42998=CARTESIAN_POINT('Ctrl Pts',(81.6532634634593,281.705245953385,52.6167718901163));
#42999=CARTESIAN_POINT('Ctrl Pts',(78.9252945386105,281.068777924728,58.415540740389));
#43000=CARTESIAN_POINT('Ctrl Pts',(72.5834632791282,280.432309896071,59.2468527844925));
#43001=CARTESIAN_POINT('Ctrl Pts',(68.4476732525639,279.795841867414,54.3678012071275));
#43002=CARTESIAN_POINT('Ctrl Pts',(70.326780909695,279.159373838757,48.2410982563761));
#43003=CARTESIAN_POINT('Ctrl Pts',(75.4561843501935,278.628983814876,46.8137262387156));
#43004=CARTESIAN_POINT('Ctrl Pts',(78.8839251560877,278.204671795772,48.6362247583429));
#43005=CARTESIAN_POINT('Ctrl Pts',(81.0983384007498,277.780359776667,51.8248423064824));
#43006=CARTESIAN_POINT('Ctrl Pts',(80.2864953634584,277.249969752786,57.0868838698871));
#43007=CARTESIAN_POINT('Ctrl Pts',(74.4244720439219,276.613501724129,59.6761341928656));
#43008=CARTESIAN_POINT('Ctrl Pts',(69.0912915673428,275.977033695473,56.1452576101099));
#43009=CARTESIAN_POINT('Ctrl Pts',(69.1681105982651,275.340565666815,49.7496339286456));
#43010=CARTESIAN_POINT('Ctrl Pts',(74.6042813775611,274.704097638159,46.3561722901173));
#43011=CARTESIAN_POINT('Ctrl Pts',(79.412935102352,274.173707614278,48.6420025303696));
#43012=CARTESIAN_POINT('Ctrl Pts',(80.8058075434052,273.749395595173,52.2656490707197));
#43013=CARTESIAN_POINT('Ctrl Pts',(80.3868186252344,273.325083576069,56.1250993130324));
#43014=CARTESIAN_POINT('Ctrl Pts',(76.3234123534648,272.794693552187,59.5655789311586));
#43015=CARTESIAN_POINT('Ctrl Pts',(70.1997566345717,272.158225523531,57.6765645663912));
#43016=CARTESIAN_POINT('Ctrl Pts',(68.4885131854145,271.521757494873,51.5136472948276));
#43017=CARTESIAN_POINT('Ctrl Pts',(72.740299548083,270.885289466217,46.7353404645114));
#43018=CARTESIAN_POINT('Ctrl Pts',(79.0697814196283,270.24882143756,47.737934037007));
#43019=CARTESIAN_POINT('Ctrl Pts',(81.2014200278245,269.718431413679,52.6168977975042));
#43020=CARTESIAN_POINT('Ctrl Pts',(79.8769093444932,269.294119394574,56.2660866575358));
#43021=CARTESIAN_POINT('Ctrl Pts',(77.0298250182992,268.86980737547,58.9052188493705));
#43022=CARTESIAN_POINT('Ctrl Pts',(71.7059457747086,268.339417351589,58.8382835682292));
#43023=CARTESIAN_POINT('Ctrl Pts',(68.3212808918114,267.702949322932,53.396631405116));
#43024=CARTESIAN_POINT('Ctrl Pts',(71.0704926838037,267.066481294275,47.6215350456437));
#43025=CARTESIAN_POINT('Ctrl Pts',(77.413848888673,266.430013265619,46.8019403308202));
#43026=CARTESIAN_POINT('Ctrl Pts',(81.5351627289913,265.793545236961,51.7093130355808));
#43027=CARTESIAN_POINT('Ctrl Pts',(79.9452721866972,265.26315521308,56.7906926312932));
#43028=CARTESIAN_POINT('Ctrl Pts',(76.5523955207542,264.838843193976,58.677302240125));
#43029=CARTESIAN_POINT('Ctrl Pts',(72.6723019530944,264.414531174871,58.8029278451709));
#43030=CARTESIAN_POINT('Ctrl Pts',(68.6966783295341,263.88414115099,55.2613763015696));
#43031=CARTESIAN_POINT('Ctrl Pts',(69.7095077253019,263.247673122334,48.9335242766798));
#43032=CARTESIAN_POINT('Ctrl Pts',(75.5720466440224,262.611205093676,46.3760761608992));
#43033=CARTESIAN_POINT('Ctrl Pts',(80.8986950719364,261.97473706502,49.9167992457815));
#43034=CARTESIAN_POINT('Ctrl Pts',(80.7923756078113,261.338269036362,56.3243128669436));
#43035=CARTESIAN_POINT('Ctrl Pts',(76.2600105715705,260.807879012482,59.1182057980456));
#43036=CARTESIAN_POINT('Ctrl Pts',(72.4612951821995,260.383566993377,58.317787609226));
#43037=CARTESIAN_POINT('Ctrl Pts',(69.4494584547942,259.959254974273,55.8683494259096));
#43038=CARTESIAN_POINT('Ctrl Pts',(68.7701667585371,259.428864950391,50.5875603443804));
#43039=CARTESIAN_POINT('Ctrl Pts',(73.6841987474315,258.792396921735,46.4741889478306));
#43040=CARTESIAN_POINT('Ctrl Pts',(79.78739015126,258.155928893078,48.3875519888271));
#43041=CARTESIAN_POINT('Ctrl Pts',(81.4872452956088,257.519460864421,54.5536200979751));
#43042=CARTESIAN_POINT('Ctrl Pts',(77.2053896188859,256.882992835764,59.321559547837));
#43043=CARTESIAN_POINT('Ctrl Pts',(71.9514325914311,256.352602811883,58.458943708744));
#43044=CARTESIAN_POINT('Ctrl Pts',(69.608268828627,255.928290792779,55.3637068087443));
#43045=CARTESIAN_POINT('Ctrl Pts',(68.9405046437633,255.503978773674,51.5394423200026));
#43046=CARTESIAN_POINT('Ctrl Pts',(71.8904013482855,254.973588749793,47.1070298882851));
#43047=CARTESIAN_POINT('Ctrl Pts',(78.2977346304908,254.337120721136,47.2237125544275));
#43048=CARTESIAN_POINT('Ctrl Pts',(81.6509829051717,253.700652692479,52.6703288844776));
#43049=CARTESIAN_POINT('Ctrl Pts',(78.8911068809706,253.064184663823,58.4403364901449));
#43050=CARTESIAN_POINT('Ctrl Pts',(72.531846601885,252.427716635165,59.2323865748476));
#43051=CARTESIAN_POINT('Ctrl Pts',(69.1307639245367,251.897326611285,55.1359482250076));
#43052=CARTESIAN_POINT('Ctrl Pts',(69.3913142509957,251.47301459218,51.2625748355938));
#43053=CARTESIAN_POINT('Ctrl Pts',(71.3948305414538,251.048702573075,47.9373935833451));
#43054=CARTESIAN_POINT('Ctrl Pts',(76.5284508786805,250.518312549195,46.5252630067303));
#43055=CARTESIAN_POINT('Ctrl Pts',(81.2894587335241,249.881844520538,50.8148246206893));
#43056=CARTESIAN_POINT('Ctrl Pts',(80.2496547382429,249.245376491881,57.1258238355375));
#43057=CARTESIAN_POINT('Ctrl Pts',(74.3824011893066,248.608908463224,59.6724371220249));
#43058=CARTESIAN_POINT('Ctrl Pts',(69.0618070063151,247.972440434567,56.1004891697511));
#43059=CARTESIAN_POINT('Ctrl Pts',(69.1801469266377,247.442050410686,50.777504462329));
#43060=CARTESIAN_POINT('Ctrl Pts',(71.9167403237001,247.017738391581,48.0239677428365));
#43061=CARTESIAN_POINT('Ctrl Pts',(75.6098036593971,246.593426372477,46.8272258805422));
#43062=CARTESIAN_POINT('Ctrl Pts',(80.4116468937403,246.063036348596,49.1273285054245));
#43063=CARTESIAN_POINT('Ctrl Pts',(81.1934106450685,245.426568319939,55.4878615075355));
#43064=CARTESIAN_POINT('Ctrl Pts',(76.2700637597904,244.790100291282,59.5708210818689));
#43065=CARTESIAN_POINT('Ctrl Pts',(70.1704175211297,244.153632262625,57.6461862589446));
#43066=CARTESIAN_POINT('Ctrl Pts',(68.4956083292596,243.517164233968,51.4605133929858));
#43067=CARTESIAN_POINT('Ctrl Pts',(72.0753836691866,242.986774210088,47.5192725924447));
#43068=CARTESIAN_POINT('Ctrl Pts',(75.9470751017479,242.562462190983,47.234819894324));
#43069=CARTESIAN_POINT('Ctrl Pts',(79.520065189934,242.138150171878,48.7529271751713));
#43070=CARTESIAN_POINT('Ctrl Pts',(81.6372030963402,241.607760147998,53.6382007209877));
#43071=CARTESIAN_POINT('Ctrl Pts',(78.0566544293302,240.97129211934,58.9530107718744));
#43072=CARTESIAN_POINT('Ctrl Pts',(71.6622303016729,240.334824090684,58.8072592228149));
#43073=CARTESIAN_POINT('Ctrl Pts',(68.3190498381245,239.698356062027,53.3544573901267));
#43074=CARTESIAN_POINT('Ctrl Pts',(71.1106908750382,239.06188803337,47.586071571299));
#43075=CARTESIAN_POINT('Ctrl Pts',(76.3977930505111,238.531498009489,46.9578032223369));
#43076=CARTESIAN_POINT('Ctrl Pts',(79.507433526864,238.107185990384,49.2818178510052));
#43077=CARTESIAN_POINT('Ctrl Pts',(81.209566592217,237.68287397128,52.770893790888));
#43078=CARTESIAN_POINT('Ctrl Pts',(79.6045905562849,237.152483947399,57.8475287448985));
#43079=CARTESIAN_POINT('Ctrl Pts',(73.4162169892982,236.516015918742,59.5123312044275));
#43080=CARTESIAN_POINT('Ctrl Pts',(68.6840167868883,235.879547890085,55.2092875510666));
#43081=CARTESIAN_POINT('Ctrl Pts',(69.735477959311,235.243079861428,48.9002200414177));
#43082=CARTESIAN_POINT('Ctrl Pts',(75.6256505593195,234.60661183277,46.3756604014124));
#43083=CARTESIAN_POINT('Ctrl Pts',(80.0293719336459,234.076221808891,49.3682192712584));
#43084=CARTESIAN_POINT('Ctrl Pts',(80.8532214045015,233.651909789785,53.1619219396033));
#43085=CARTESIAN_POINT('Ctrl Pts',(79.8504433688653,233.227597770682,56.9123011334566));
#43086=CARTESIAN_POINT('Ctrl Pts',(75.3098000176901,232.697207746799,59.6927198950109));
#43087=CARTESIAN_POINT('Ctrl Pts',(69.5459368691264,232.060739718144,56.8917528765499));
#43088=CARTESIAN_POINT('Ctrl Pts',(68.7947633682085,231.424271689486,50.5399309481628));
#43089=CARTESIAN_POINT('Ctrl Pts',(73.7256447190361,230.78780366083,46.4660737412472));
#43090=CARTESIAN_POINT('Ctrl Pts',(79.8281335926119,230.151335632172,48.4223876685125));
#43091=CARTESIAN_POINT('Ctrl Pts',(81.1906277281917,229.620945608292,53.5694043056184));
#43092=CARTESIAN_POINT('Ctrl Pts',(79.3249956567615,229.196633589187,56.973860923079));
#43093=CARTESIAN_POINT('Ctrl Pts',(76.1086729866622,228.772321570083,59.1478380087876));
#43094=CARTESIAN_POINT('Ctrl Pts',(70.8573012407579,228.241931546201,58.2696208856052));
#43095=CARTESIAN_POINT('Ctrl Pts',(68.3422715097577,227.605463517545,52.3753728345039));
#43096=CARTESIAN_POINT('Ctrl Pts',(71.9402036438859,226.968995488888,47.087198498792));
#43097=CARTESIAN_POINT('Ctrl Pts',(78.3343475963114,226.332527460231,47.2447628702198));
#43098=CARTESIAN_POINT('Ctrl Pts',(81.6589013761616,225.696059431574,52.7233463383287));
#43099=CARTESIAN_POINT('Ctrl Pts',(79.3125390351989,225.165669407693,57.5027557511392));
#43100=CARTESIAN_POINT('Ctrl Pts',(75.6715948746436,224.741357388588,58.8497648206672));
#43101=CARTESIAN_POINT('Ctrl Pts',(71.8177424321106,224.317045369484,58.3820796919963));
#43102=CARTESIAN_POINT('Ctrl Pts',(68.4288418723472,223.786655345603,54.2755576487171));
#43103=CARTESIAN_POINT('Ctrl Pts',(70.395023167623,223.150187316946,48.1762408565892));
#43104=CARTESIAN_POINT('Ctrl Pts',(76.5790555611666,222.513719288289,46.5429470970313));
#43105=CARTESIAN_POINT('Ctrl Pts',(81.3032979875237,221.877251259633,50.8547257155437));
#43106=CARTESIAN_POINT('Ctrl Pts',(80.2208684679564,221.240783230975,57.1710441926388));
#43107=CARTESIAN_POINT('Ctrl Pts',(75.3153785508202,220.710393207095,59.2409109611796));
#43108=CARTESIAN_POINT('Ctrl Pts',(71.6832052365558,220.286081187989,57.8704308428568));
#43109=CARTESIAN_POINT('Ctrl Pts',(69.0802282421642,219.861769168886,54.9902519886439));
#43110=CARTESIAN_POINT('Ctrl Pts',(69.2143835119882,219.331379145004,49.6676414947474));
#43111=CARTESIAN_POINT('Ctrl Pts',(74.698326373318,218.694911116347,46.3519543542357));
#43112=CARTESIAN_POINT('Ctrl Pts',(80.4382692886431,218.05844308769,49.1738612228084));
#43113=CARTESIAN_POINT('Ctrl Pts',(81.177672384873,217.421975059033,55.5270645828276));
#43114=CARTESIAN_POINT('Ctrl Pts',(76.2187228071657,216.785507030377,59.5860802860795));
#43115=CARTESIAN_POINT('Ctrl Pts',(71.1576983282718,216.255117006495,57.9321749584298));
#43116=CARTESIAN_POINT('Ctrl Pts',(69.31426183066,215.830804987392,54.5157242093268));
#43117=CARTESIAN_POINT('Ctrl Pts',(69.2372749896401,215.406492968286,50.6344011155516));
#43118=CARTESIAN_POINT('Ctrl Pts',(72.829541004845,214.876102944406,46.7037054021372));
#43119=CARTESIAN_POINT('Ctrl Pts',(79.1426438599285,214.239634915749,47.7965405392687));
#43120=CARTESIAN_POINT('Ctrl Pts',(81.6284456217072,213.603166887092,53.6905654701027));
#43121=CARTESIAN_POINT('Ctrl Pts',(78.0159571360404,212.966698858435,58.9727077333983));
#43122=CARTESIAN_POINT('Ctrl Pts',(71.6194256917035,212.330230829778,58.7843319643082));
#43123=CARTESIAN_POINT('Ctrl Pts',(68.3174643030566,211.693762801121,53.3056650395866));
#43124=CARTESIAN_POINT('Ctrl Pts',(71.1496401123775,211.057294772464,47.5586365481913));
#43125=CARTESIAN_POINT('Ctrl Pts',(76.4416934236012,210.526904748583,46.9679457097492));
#43126=CARTESIAN_POINT('Ctrl Pts',(79.5342341192608,210.102592729479,49.3146003451081));
#43127=CARTESIAN_POINT('Ctrl Pts',(81.2112769892146,209.678280710374,52.8157317414015));
#43128=CARTESIAN_POINT('Ctrl Pts',(79.5696286458101,209.147890686493,57.8807452976899));
#43129=CARTESIAN_POINT('Ctrl Pts',(73.3694517075265,208.511422657837,59.5008055828234));
#43130=CARTESIAN_POINT('Ctrl Pts',(68.6683970655276,207.874954629179,55.1637564563535));
#43131=CARTESIAN_POINT('Ctrl Pts',(69.7653637905974,207.238486600523,48.8624258785963));
#43132=CARTESIAN_POINT('Ctrl Pts',(75.6735905312152,206.602018571865,46.3804373005538));
#43133=CARTESIAN_POINT('Ctrl Pts',(80.0556099260794,206.071628547985,49.4046869809193));
#43134=CARTESIAN_POINT('Ctrl Pts',(80.8520645262666,205.64731652888,53.2042368931363));
#43135=CARTESIAN_POINT('Ctrl Pts',(79.8222544701088,205.223004509775,56.947282442927));
#43136=CARTESIAN_POINT('Ctrl Pts',(75.2616679235261,204.692614485895,59.6948686777458));
#43137=CARTESIAN_POINT('Ctrl Pts',(69.5181641574838,204.056146457238,56.8523878495988));
#43138=CARTESIAN_POINT('Ctrl Pts',(68.8128385238247,203.419678428581,50.4953117049742));
#43139=CARTESIAN_POINT('Ctrl Pts',(73.7729845636653,202.783210399924,46.4571368186103));
#43140=CARTESIAN_POINT('Ctrl Pts',(79.8611997119805,202.146742371267,48.4574294283178));
#43141=CARTESIAN_POINT('Ctrl Pts',(81.1865226116244,201.616352347386,53.6141424809881));
#43142=CARTESIAN_POINT('Ctrl Pts',(79.2963758820999,201.192040328282,57.0050499361194));
#43143=CARTESIAN_POINT('Ctrl Pts',(76.064451658235,200.767728309176,59.1557646138185));
#43144=CARTESIAN_POINT('Ctrl Pts',(70.8195529427137,200.237338285297,58.2396816294403));
#43145=CARTESIAN_POINT('Ctrl Pts',(68.3471157639746,199.600870256639,52.3274410178494));
#43146=CARTESIAN_POINT('Ctrl Pts',(71.9831085027866,198.964402227983,47.0653634605732));
#43147=CARTESIAN_POINT('Ctrl Pts',(78.3759491980706,198.327934199325,47.2690575728888));
#43148=CARTESIAN_POINT('Ctrl Pts',(81.6608883801067,197.691466170669,52.7714851467922));
#43149=CARTESIAN_POINT('Ctrl Pts',(79.2801036087496,197.161076146787,57.5338411185366));
#43150=CARTESIAN_POINT('Ctrl Pts',(75.6295355167696,196.736764127683,58.8545456627842));
#43151=CARTESIAN_POINT('Ctrl Pts',(71.7791577583434,196.312452108578,58.3590671026649));
#43152=CARTESIAN_POINT('Ctrl Pts',(68.4199739824153,195.782062084697,54.2282009838377));
#43153=CARTESIAN_POINT('Ctrl Pts',(70.4301108370362,195.14559405604,48.1432289658392));
#43154=CARTESIAN_POINT('Ctrl Pts',(76.6257663738702,194.509126027384,46.5545956201064));
#43155=CARTESIAN_POINT('Ctrl Pts',(81.3187765389438,193.872657998727,50.9003474571235));
#43156=CARTESIAN_POINT('Ctrl Pts',(80.1908023736674,193.236189970069,57.208691845023));
#43157=CARTESIAN_POINT('Ctrl Pts',(75.2705069128446,192.705799946189,59.2431114453968));
#43158=CARTESIAN_POINT('Ctrl Pts',(71.6483148472814,192.281487927084,57.8464609785267));
#43159=CARTESIAN_POINT('Ctrl Pts',(69.0661887410767,191.857175907979,54.9475762519299));
#43160=CARTESIAN_POINT('Ctrl Pts',(69.2387374677117,191.326785884099,49.6260729427954));
#43161=CARTESIAN_POINT('Ctrl Pts',(74.746470817058,190.690317855442,46.3500375360377));
#43162=CARTESIAN_POINT('Ctrl Pts',(80.4658856290766,190.053849826785,49.2132870268233));
#43163=CARTESIAN_POINT('Ctrl Pts',(81.1594658110218,189.417381798128,55.571655525867));
#43164=CARTESIAN_POINT('Ctrl Pts',(76.1712915211055,188.780913769471,59.5947950818913));
#43165=CARTESIAN_POINT('Ctrl Pts',(71.122455804744,188.25052374559,57.9044020975852));
#43166=CARTESIAN_POINT('Ctrl Pts',(69.3035327663159,187.826211726486,54.4747626315898));
#43167=CARTESIAN_POINT('Ctrl Pts',(69.2549135694621,187.40189970738,50.5929403713447));
#43168=CARTESIAN_POINT('Ctrl Pts',(72.8746450227851,186.871509683501,46.6883642435143));
#43169=CARTESIAN_POINT('Ctrl Pts',(79.1811568044568,186.235041654843,47.8265398808685));
#43170=CARTESIAN_POINT('Ctrl Pts',(81.6217878086657,185.598573626186,53.738665026678));
#43171=CARTESIAN_POINT('Ctrl Pts',(77.9760801015144,184.962105597529,58.9940164661573));
#43172=CARTESIAN_POINT('Ctrl Pts',(71.5719371009017,184.325637568872,58.760591828347));
#43173=CARTESIAN_POINT('Ctrl Pts',(68.8685169582398,183.795247544992,54.1736876365801));
#43174=CARTESIAN_POINT('Ctrl Pts',(69.7441447209343,183.370935525887,50.3916003943771));
#43175=CARTESIAN_POINT('Ctrl Pts',(72.2528560934249,182.946623506783,47.4289537505847));
#43176=CARTESIAN_POINT('Ctrl Pts',(77.5460829854539,182.416233482901,46.8545674679323));
#43177=CARTESIAN_POINT('Ctrl Pts',(81.5611495397949,181.779765454245,51.8492421518375));
#43178=CARTESIAN_POINT('Ctrl Pts',(79.5270748169464,181.143297425587,57.9132708011999));
#43179=CARTESIAN_POINT('Ctrl Pts',(73.3284950085148,180.506829396931,59.4904555706305));
#43180=CARTESIAN_POINT('Ctrl Pts',(68.6464467632618,179.870361368274,55.1148460287544));
#43181=CARTESIAN_POINT('Ctrl Pts',(69.6131321617587,179.339971344393,49.8790376028731));
#43182=CARTESIAN_POINT('Ctrl Pts',(72.7542485557096,178.915659325288,47.5977450556339));
#43183=CARTESIAN_POINT('Ctrl Pts',(76.5910088428193,178.491347306184,47.0059863330989));
#43184=CARTESIAN_POINT('Ctrl Pts',(80.9640223938111,177.960957282303,50.0432421693827));
#43185=CARTESIAN_POINT('Ctrl Pts',(80.7202401717823,177.324489253646,56.4469992589398));
#43186=CARTESIAN_POINT('Ctrl Pts',(75.208166943184,176.688021224989,59.6915257515102));
#43187=CARTESIAN_POINT('Ctrl Pts',(69.4940514634066,176.051553196332,56.8177150893079));
#43188=CARTESIAN_POINT('Ctrl Pts',(68.828326029216,175.415085167675,50.4439921364254));
#43189=CARTESIAN_POINT('Ctrl Pts',(72.9914360826229,174.884695143794,47.1248529083393));
#43190=CARTESIAN_POINT('Ctrl Pts',(76.8588776947801,174.46038312469,47.4622003004928));
#43191=CARTESIAN_POINT('Ctrl Pts',(80.1436543482285,174.036071105585,49.5312943591081));
#43192=CARTESIAN_POINT('Ctrl Pts',(81.4536551141952,173.505681081704,54.6919211161372));
#43193=CARTESIAN_POINT('Ctrl Pts',(77.0704786758444,172.869213053048,59.3668862437205));
#43194=CARTESIAN_POINT('Ctrl Pts',(70.781351567379,172.23274502439,58.2020756788708));
#43195=CARTESIAN_POINT('Ctrl Pts',(68.351646798808,171.596276995734,52.2854517956076));
#43196=CARTESIAN_POINT('Ctrl Pts',(72.0284531099989,170.959808967076,47.0367729157542));
#43197=CARTESIAN_POINT('Ctrl Pts',(77.3480421827307,170.429418943196,47.260698415578));
#43198=CARTESIAN_POINT('Ctrl Pts',(80.0467424555462,170.005106924091,50.0513837657998));
#43199=CARTESIAN_POINT('Ctrl Pts',(81.1699777859826,169.580794904987,53.767463727116));
#43200=CARTESIAN_POINT('Ctrl Pts',(78.7750585603247,169.050404881106,58.5227273827689));
#43201=CARTESIAN_POINT('Ctrl Pts',(72.4002672174427,168.413936852449,59.1781432572696));
#43202=CARTESIAN_POINT('Ctrl Pts',(68.415791308239,167.777468823792,54.1747588859273));
#43203=CARTESIAN_POINT('Ctrl Pts',(70.4610652576824,167.141000795135,48.1144983378858));
#43204=CARTESIAN_POINT('Ctrl Pts',(76.6787490482889,166.504532766478,46.5627435525341));
#43205=CARTESIAN_POINT('Ctrl Pts',(80.5481907545866,165.974142742597,50.220009117647));
#43206=CARTESIAN_POINT('Ctrl Pts',(80.7557724814388,165.549830723493,54.0965820517106));
#43207=CARTESIAN_POINT('Ctrl Pts',(79.1670753196014,165.125518704388,57.6387493563994));
#43208=CARTESIAN_POINT('Ctrl Pts',(74.2407590117034,164.595128680508,59.6585459220802));
#43209=CARTESIAN_POINT('Ctrl Pts',(68.9980337649973,163.95866065185,55.9732553471886));
#43210=CARTESIAN_POINT('Ctrl Pts',(69.2706230284558,163.322192623193,49.5829816025151));
#43211=CARTESIAN_POINT('Ctrl Pts',(74.7886807951738,162.685724594536,46.3486436607436));
#43212=CARTESIAN_POINT('Ctrl Pts',(80.5005445843739,162.04925656588,49.2541809066686));
#43213=CARTESIAN_POINT('Ctrl Pts',(81.0237923101313,161.518866541998,54.5527073385821));
#43214=CARTESIAN_POINT('Ctrl Pts',(78.6385393623837,161.094554522894,57.6156269035887));
#43215=CARTESIAN_POINT('Ctrl Pts',(75.1163796021698,160.670242503789,59.2482011009735));
#43216=CARTESIAN_POINT('Ctrl Pts',(70.0725868922178,160.139852479909,57.5428197268428));
#43217=CARTESIAN_POINT('Ctrl Pts',(68.530890451871,159.503384451252,51.3226343019818));
#43218=CARTESIAN_POINT('Ctrl Pts',(72.9269747274227,158.866916422595,46.6767386422982));
#43219=CARTESIAN_POINT('Ctrl Pts',(79.2139392306464,158.230448393938,47.8531657644027));
#43220=CARTESIAN_POINT('Ctrl Pts',(81.6211399760129,157.593980365281,53.7922666395636));
#43221=CARTESIAN_POINT('Ctrl Pts',(78.5417996070232,157.0635903414,58.135748356356));
#43222=CARTESIAN_POINT('Ctrl Pts',(74.7324983674773,156.639278322295,58.8841679932114));
#43223=CARTESIAN_POINT('Ctrl Pts',(71.002752658437,156.214966303191,57.8071792131713));
#43224=CARTESIAN_POINT('Ctrl Pts',(68.3129682762291,155.68457627931,53.2122656656242));
#43225=CARTESIAN_POINT('Ctrl Pts',(71.2277399375131,155.048108250653,47.5051086854453));
#43226=CARTESIAN_POINT('Ctrl Pts',(77.5932150058283,154.411640221996,46.8801042110002));
#43227=CARTESIAN_POINT('Ctrl Pts',(81.5684408542748,153.775172193339,51.8908409724219));
#43228=CARTESIAN_POINT('Ctrl Pts',(79.4914376377215,153.138704164682,57.9533150772952));
#43229=CARTESIAN_POINT('Ctrl Pts',(74.3184020126598,152.608314140801,59.2134233877355));
#43230=CARTESIAN_POINT('Ctrl Pts',(70.9516299530984,152.184002121697,57.2806135715887));
#43231=CARTESIAN_POINT('Ctrl Pts',(68.8418931422078,151.759690102592,54.0217919325278));
#43232=CARTESIAN_POINT('Ctrl Pts',(69.8241254614745,151.229300078712,48.7888778110099));
#43233=CARTESIAN_POINT('Ctrl Pts',(75.7671119106681,150.592832050054,46.3912859569748));
#43234=CARTESIAN_POINT('Ctrl Pts',(80.982861794159,149.956364021397,50.0934281194647));
#43235=CARTESIAN_POINT('Ctrl Pts',(80.6984675924352,149.31989599274,56.4831873775621));
#43236=CARTESIAN_POINT('Ctrl Pts',(75.1550028210449,148.683427964083,59.698390786709));
#43237=CARTESIAN_POINT('Ctrl Pts',(70.4230863720779,148.153037940203,57.2576660475808));
#43238=CARTESIAN_POINT('Ctrl Pts',(69.1485793584295,147.728725921098,53.5907136673885));
#43239=CARTESIAN_POINT('Ctrl Pts',(69.6926334846929,147.304413901994,49.7468987662606));
#43240=CARTESIAN_POINT('Ctrl Pts',(73.8655835469356,146.774023878113,46.4401392784498));
#43241=CARTESIAN_POINT('Ctrl Pts',(79.9246904329767,146.137555849456,48.5269450617855));
#43242=CARTESIAN_POINT('Ctrl Pts',(81.434970490104,145.501087820799,54.7421648959878));
#43243=CARTESIAN_POINT('Ctrl Pts',(77.0303108800882,144.864619792142,59.3799312935453));
#43244=CARTESIAN_POINT('Ctrl Pts',(70.7367111994093,144.228151763485,58.1723975701266));
#43245=CARTESIAN_POINT('Ctrl Pts',(68.764577662108,143.697761739604,53.2268076312774));
#43246=CARTESIAN_POINT('Ctrl Pts',(70.206850777246,143.273449720499,49.6225384754308));
#43247=CARTESIAN_POINT('Ctrl Pts',(73.1381064817095,142.849137701395,47.0772196581726));
#43248=CARTESIAN_POINT('Ctrl Pts',(78.4570069957002,142.318747677514,47.3169441968919));
#43249=CARTESIAN_POINT('Ctrl Pts',(81.6632403479369,141.682279648857,52.8656019016743));
#43250=CARTESIAN_POINT('Ctrl Pts',(78.7280054750341,141.0458116202,58.5484092782544));
#43251=CARTESIAN_POINT('Ctrl Pts',(72.3613866346612,140.409343591543,59.1616530958568));
#43252=CARTESIAN_POINT('Ctrl Pts',(68.4015487075305,139.772875562886,54.1230800612873));
#43253=CARTESIAN_POINT('Ctrl Pts',(70.1555537992788,139.242485539006,49.0959897825756));
#43254=CARTESIAN_POINT('Ctrl Pts',(73.6078856957486,138.818173519901,47.320514532662));
#43255=CARTESIAN_POINT('Ctrl Pts',(77.490012397573,138.393861500796,47.3209112928323));
#43256=CARTESIAN_POINT('Ctrl Pts',(81.3485743749271,137.863471476916,50.9896535840151));
#43257=CARTESIAN_POINT('Ctrl Pts',(80.1308631311827,137.227003448258,57.2812920002539));
#43258=CARTESIAN_POINT('Ctrl Pts',(74.1883937223739,136.590535419602,59.6470816704889));
#43259=CARTESIAN_POINT('Ctrl Pts',(68.9794920835046,135.954067390944,55.9353102396218));
#43260=CARTESIAN_POINT('Ctrl Pts',(69.2937571436266,135.317599362288,49.534624955543));
#43261=CARTESIAN_POINT('Ctrl Pts',(73.9144292228386,134.787209338407,46.8893347883613));
#43262=CARTESIAN_POINT('Ctrl Pts',(77.6851592684559,134.362897319302,47.8126455754286));
#43263=CARTESIAN_POINT('Ctrl Pts',(80.6158946395786,133.938585300198,50.3585634984749));
#43264=CARTESIAN_POINT('Ctrl Pts',(81.1234025901064,133.408195276317,55.6586206880105));
#43265=CARTESIAN_POINT('Ctrl Pts',(76.0784316098281,132.77172724766,59.6103041826723));
#43266=CARTESIAN_POINT('Ctrl Pts',(70.0405686636907,132.135259219003,57.4998268712375));
#43267=CARTESIAN_POINT('Ctrl Pts',(68.5417731922881,131.498791190346,51.2818275488413));
#43268=CARTESIAN_POINT('Ctrl Pts',(72.9761497214014,130.862323161689,46.6553991821764));
#43269=CARTESIAN_POINT('Ctrl Pts',(78.1993353737933,130.331933137808,47.6881151028675));
#43270=CARTESIAN_POINT('Ctrl Pts',(80.4407861829379,129.907621118704,50.8577848264537));
#43271=CARTESIAN_POINT('Ctrl Pts',(80.9840546085708,129.483309099599,54.7017108538572));
#43272=CARTESIAN_POINT('Ctrl Pts',(77.8918269900061,128.952919075718,59.0360272806059));
#43273=CARTESIAN_POINT('Ctrl Pts',(71.4916583615966,128.316451047061,58.7114103344188));
#43274=CARTESIAN_POINT('Ctrl Pts',(68.3169862074485,127.679983018404,53.1588109294466));
#43275=CARTESIAN_POINT('Ctrl Pts',(71.2627145002853,127.043514989747,47.4814358085654));
#43276=CARTESIAN_POINT('Ctrl Pts',(77.644334875132,126.40704696109,46.8962383844676));
#43277=CARTESIAN_POINT('Ctrl Pts',(80.9106458936276,125.87665693721,51.1009242065776));
#43278=CARTESIAN_POINT('Ctrl Pts',(80.5244948813005,125.452344918105,54.9637981732141));
#43279=CARTESIAN_POINT('Ctrl Pts',(78.414091999895,125.028032899,58.2221885065829));
#43280=CARTESIAN_POINT('Ctrl Pts',(73.2373364704086,124.49764287512,59.4669265192302));
#43281=CARTESIAN_POINT('Ctrl Pts',(68.6180861968185,123.861174846463,55.0250731286094));
#43282=CARTESIAN_POINT('Ctrl Pts',(69.8622107451905,123.224706817806,48.7511542937376));
#43283=CARTESIAN_POINT('Ctrl Pts',(75.8090405776548,122.588238789149,46.3963467894746));
#43284=CARTESIAN_POINT('Ctrl Pts',(81.0108775362534,121.951770760492,50.1391300973867));
#43285=CARTESIAN_POINT('Ctrl Pts',(80.7198044889218,121.421380736611,55.4554678418605));
#43286=CARTESIAN_POINT('Ctrl Pts',(77.8952676648289,120.997068717506,58.1187176641229));
#43287=CARTESIAN_POINT('Ctrl Pts',(74.1653018934157,120.572756698402,59.1949440485428));
#43288=CARTESIAN_POINT('Ctrl Pts',(69.4406556577397,120.042366674521,56.7401755299422));
#43289=CARTESIAN_POINT('Ctrl Pts',(68.8657804610841,119.405898645864,50.3576170192741));
#43290=CARTESIAN_POINT('Ctrl Pts',(73.9190741955237,118.769430617207,46.4366317002641));
#43291=CARTESIAN_POINT('Ctrl Pts',(79.9530279387085,118.13296258855,48.5582597693486));
#43292=CARTESIAN_POINT('Ctrl Pts',(81.4261542452689,117.496494559893,54.7950404708605));
#43293=CARTESIAN_POINT('Ctrl Pts',(77.7203244431643,116.966104536013,58.6179969197401));
#43294=CARTESIAN_POINT('Ctrl Pts',(73.841439580255,116.541792516908,58.7766162966422));
#43295=CARTESIAN_POINT('Ctrl Pts',(70.3196135975197,116.117480497803,57.1433221915374));
#43296=CARTESIAN_POINT('Ctrl Pts',(68.3621779488011,115.587090473922,52.1918965167118));
#43297=CARTESIAN_POINT('Ctrl Pts',(72.1133696732489,114.950622445266,46.9961198394222));
#43298=CARTESIAN_POINT('Ctrl Pts',(78.4996923124141,114.314154416609,47.3493712893946));
#43299=CARTESIAN_POINT('Ctrl Pts',(81.6641011668332,113.677686387952,52.9078261142979));
#43300=CARTESIAN_POINT('Ctrl Pts',(78.6866772492128,113.041218359294,58.5825491426592));
#43301=CARTESIAN_POINT('Ctrl Pts',(73.3819666201983,112.510828335414,59.0388557003805));
#43302=CARTESIAN_POINT('Ctrl Pts',(70.3494075285618,112.086516316309,56.6151203100856));
#43303=CARTESIAN_POINT('Ctrl Pts',(68.7614344313501,111.662204297205,53.0726283441146));
#43304=CARTESIAN_POINT('Ctrl Pts',(70.5303630449218,111.131814273324,48.0507699139827));
#43305=CARTESIAN_POINT('Ctrl Pts',(76.7695181841129,110.495346244667,46.587732736418));
#43306=CARTESIAN_POINT('Ctrl Pts',(81.359538331985,109.85887821601,51.0421259027817));
#43307=CARTESIAN_POINT('Ctrl Pts',(80.1038254574957,109.222410187353,57.3137356335653));
#43308=CARTESIAN_POINT('Ctrl Pts',(74.1348045617336,108.585942158696,59.6457571128379));
#43309=CARTESIAN_POINT('Ctrl Pts',(69.8305489765598,108.055552134815,56.5118211866107));
#43310=CARTESIAN_POINT('Ctrl Pts',(69.1302854250172,107.631240115711,52.6933740094433));
#43311=CARTESIAN_POINT('Ctrl Pts',(70.2542803117838,107.206928096606,48.9775237190036));
#43312=CARTESIAN_POINT('Ctrl Pts',(74.8827889425443,106.676538072725,46.3459693518712));
#43313=CARTESIAN_POINT('Ctrl Pts',(80.5526889428833,106.040070044068,49.3325675203539));
#43314=CARTESIAN_POINT('Ctrl Pts',(81.0972727913765,105.403602015411,55.7054265232176));
#43315=CARTESIAN_POINT('Ctrl Pts',(76.0367440446578,104.767133986754,59.6170696871648));
#43316=CARTESIAN_POINT('Ctrl Pts',(70.0009775363973,104.130665958098,57.4636869316869));
#43317=CARTESIAN_POINT('Ctrl Pts',(68.8062846772482,103.600275934217,52.2751534679328));
#43318=CARTESIAN_POINT('Ctrl Pts',(70.781449457728,103.175963915112,48.9330535328036));
#43319=CARTESIAN_POINT('Ctrl Pts',(74.0666489726483,102.751651896007,46.8646309372967));
#43320=CARTESIAN_POINT('Ctrl Pts',(79.2867442551898,102.221261872127,47.912855995854));
#43321=CARTESIAN_POINT('Ctrl Pts',(81.6091085496205,101.58479384347,53.8856408335813));
#43322=CARTESIAN_POINT('Ctrl Pts',(77.8414071731253,100.948325814813,59.0542315289232));
#43323=CARTESIAN_POINT('Ctrl Pts',(71.4557480292651,100.311857786156,58.689182577611));
#43324=CARTESIAN_POINT('Ctrl Pts',(68.3107929723319,99.6753897574989,53.1055643668355));
#43325=CARTESIAN_POINT('Ctrl Pts',(70.811068570169,99.144999733618,48.404841819497));
#43326=CARTESIAN_POINT('Ctrl Pts',(74.4938206403223,98.7206877145134,47.176735522705));
#43327=CARTESIAN_POINT('Ctrl Pts',(78.330459889719,98.2963756954088,47.7692784801554));
#43328=CARTESIAN_POINT('Ctrl Pts',(81.5842679143076,97.765985671528,51.9836472195184));
#43329=CARTESIAN_POINT('Ctrl Pts',(79.4211258880999,97.129517642871,58.0159230096566));
#43330=CARTESIAN_POINT('Ctrl Pts',(73.1873326085736,96.4930496142142,59.4476090040522));
#43331=CARTESIAN_POINT('Ctrl Pts',(68.6055493474303,95.8565815855572,54.9847438272487));
#43332=CARTESIAN_POINT('Ctrl Pts',(69.8924501197539,95.2201135569002,48.7068922014112));
#43333=CARTESIAN_POINT('Ctrl Pts',(74.8625460934215,94.6897235330196,46.7973591315942));
#43334=CARTESIAN_POINT('Ctrl Pts',(78.4483177343854,94.2654115139148,48.2850249627864));
#43335=CARTESIAN_POINT('Ctrl Pts',(80.9564234790893,93.8410994948103,51.2481843341032));
#43336=CARTESIAN_POINT('Ctrl Pts',(80.6495613460078,93.3107094709293,56.5636340952688));
#43337=CARTESIAN_POINT('Ctrl Pts',(75.0608638721642,92.6742414422724,59.6995542440752));
#43338=CARTESIAN_POINT('Ctrl Pts',(69.4155699040053,92.0377734136156,56.6928019344417));
#43339=CARTESIAN_POINT('Ctrl Pts',(68.8827602162151,91.4013053849584,50.3189477413327));
#43340=CARTESIAN_POINT('Ctrl Pts',(73.9709287285413,90.7648373563017,46.423042734276));
#43341=CARTESIAN_POINT('Ctrl Pts',(78.9754721333284,90.2344473324207,48.2403803038539));
#43342=CARTESIAN_POINT('Ctrl Pts',(80.7072165422673,89.8101353133163,51.7148542479994));
#43343=CARTESIAN_POINT('Ctrl Pts',(80.6578038883262,89.3858232942115,55.596666489217));
#43344=CARTESIAN_POINT('Ctrl Pts',(76.9406356429825,88.8554332703309,59.4085991706795));
#43345=CARTESIAN_POINT('Ctrl Pts',(70.6648736271285,88.2189652416738,58.1115464523212));
#43346=CARTESIAN_POINT('Ctrl Pts',(68.3743024533118,87.5824972130169,52.1396801497238));
#43347=CARTESIAN_POINT('Ctrl Pts',(72.1515458643403,86.9460291843599,46.9780587327407));
#43348=CARTESIAN_POINT('Ctrl Pts',(78.5477530123006,86.3095611557031,47.3731141139413));
#43349=CARTESIAN_POINT('Ctrl Pts',(81.1344914826134,85.7791711318223,52.0268174369308));
#43350=CARTESIAN_POINT('Ctrl Pts',(80.1636448686008,85.3548591127175,55.78558914302));
#43351=CARTESIAN_POINT('Ctrl Pts',(77.580926274119,84.9305470936132,58.683946013413));
#43352=CARTESIAN_POINT('Ctrl Pts',(72.2748837406891,84.4001570697319,59.1244947231283));
#43353=CARTESIAN_POINT('Ctrl Pts',(68.3872132968793,83.7636890410755,54.030031733356));
#43354=CARTESIAN_POINT('Ctrl Pts',(70.5737567372417,83.1272210124182,48.0192970676245));
#43355=CARTESIAN_POINT('Ctrl Pts',(76.8101842784523,82.4907529837615,46.5991298374534));
#43356=CARTESIAN_POINT('Ctrl Pts',(81.3802552051738,81.8542849551044,51.0915664100236));
#43357=CARTESIAN_POINT('Ctrl Pts',(80.2816734014653,81.3238949312238,56.3012965904414));
#43358=CARTESIAN_POINT('Ctrl Pts',(77.0839556680519,80.8995829121189,58.5025483215824));
#43359=CARTESIAN_POINT('Ctrl Pts',(73.2334767124565,80.4752708930145,58.9972398405646));
#43360=CARTESIAN_POINT('Ctrl Pts',(68.9385484018002,79.9448808691335,55.8505334134376));
#43361=CARTESIAN_POINT('Ctrl Pts',(69.3439483205791,79.3084128404767,49.4549735833925));
#43362=CARTESIAN_POINT('Ctrl Pts',(74.9361886871511,78.6719448118197,46.3506618849799));
#43363=CARTESIAN_POINT('Ctrl Pts',(80.5759183421823,78.0354767831628,49.3678381901666));
#43364=CARTESIAN_POINT('Ctrl Pts',(81.0804944619725,77.3990087545058,55.7563386067879));
#43365=CARTESIAN_POINT('Ctrl Pts',(76.8349031968461,76.8686187306251,58.969300688992));
#43366=CARTESIAN_POINT('Ctrl Pts',(72.9772127085787,76.4443067115204,58.5344076180339));
#43367=CARTESIAN_POINT('Ctrl Pts',(69.7457281592464,76.0199946924158,56.3830323616302));
#43368=CARTESIAN_POINT('Ctrl Pts',(68.5664513403961,75.489604668535,51.1909733561184));
#43369=CARTESIAN_POINT('Ctrl Pts',(73.0662735475183,74.853136639878,46.6281743535191));
#43370=CARTESIAN_POINT('Ctrl Pts',(79.323983898762,74.2166686112211,47.9514145427363));
#43371=CARTESIAN_POINT('Ctrl Pts',(81.6035187270877,73.5802005825642,53.9275022600366));
#43372=CARTESIAN_POINT('Ctrl Pts',(77.7953551100307,72.9437325539072,59.0816680023808));
#43373=CARTESIAN_POINT('Ctrl Pts',(72.4831162429305,72.4133425300264,58.7234938114221));
#43374=CARTESIAN_POINT('Ctrl Pts',(69.8557414558012,71.9890305109219,55.8655558109758));
#43375=CARTESIAN_POINT('Ctrl Pts',(68.8266955931637,71.5647184918171,52.1222988736249));
#43376=CARTESIAN_POINT('Ctrl Pts',(71.340922056943,71.0343284679364,47.4290232775165));
#43377=CARTESIAN_POINT('Ctrl Pts',(77.7302302056465,70.3978604392794,46.9347804073151));
#43378=CARTESIAN_POINT('Ctrl Pts',(81.5870998373005,69.7613924106225,52.0371778911306));
#43379=CARTESIAN_POINT('Ctrl Pts',(79.3894558859262,69.1249243819656,58.0438628754964));
#43380=CARTESIAN_POINT('Ctrl Pts',(73.1345725628523,68.4884563533086,59.4381258523295));
#43381=CARTESIAN_POINT('Ctrl Pts',(69.3587108404486,67.9580663294278,55.6843226095527));
#43382=CARTESIAN_POINT('Ctrl Pts',(69.249079101151,67.5337543103232,51.8037442031582));
#43383=CARTESIAN_POINT('Ctrl Pts',(70.9267097640773,67.1094422912186,48.3028210041651));
#43384=CARTESIAN_POINT('Ctrl Pts',(75.9024554322703,66.5790522673377,46.4080583336293));
#43385=CARTESIAN_POINT('Ctrl Pts',(81.050455211294,65.9425842386809,50.2245531795589));
#43386=CARTESIAN_POINT('Ctrl Pts',(80.6165978913874,65.3061162100238,56.6059065833737));
#43387=CARTESIAN_POINT('Ctrl Pts',(75.0186321565642,64.669648181367,59.6998818693395));
#43388=CARTESIAN_POINT('Ctrl Pts',(69.3819545731897,64.0331801527098,56.6510459513343));
#43389=CARTESIAN_POINT('Ctrl Pts',(68.9926619294876,63.5027901288293,51.3409968207));
#43390=CARTESIAN_POINT('Ctrl Pts',(71.4544933619757,63.0784781097245,48.3392816635851));
#43391=CARTESIAN_POINT('Ctrl Pts',(75.0167527772727,62.65416609062,46.7961628267598));
#43392=CARTESIAN_POINT('Ctrl Pts',(80.0158763253887,62.1237760667393,48.6283566709993));
#43393=CARTESIAN_POINT('Ctrl Pts',(81.4000209976796,61.4873080380821,54.8854868566357));
#43394=CARTESIAN_POINT('Ctrl Pts',(76.8880290754071,60.8508400094253,59.418899735667));
#43395=CARTESIAN_POINT('Ctrl Pts',(70.6327739589726,60.2143719807683,58.0841012989217));
#43396=CARTESIAN_POINT('Ctrl Pts',(68.3763035247955,59.5779039521114,52.0861119846998));
#43397=CARTESIAN_POINT('Ctrl Pts',(71.5643353852583,59.0475139282306,47.82176873059));
#43398=CARTESIAN_POINT('Ctrl Pts',(75.3913197498731,58.623201909126,47.1697729028191));
#43399=CARTESIAN_POINT('Ctrl Pts',(79.0926822278916,58.1988898900212,48.3405947051246));
#43400=CARTESIAN_POINT('Ctrl Pts',(81.6655870483687,57.6684998661406,53.0019605261004));
#43401=CARTESIAN_POINT('Ctrl Pts',(78.6076385065898,57.0320318374835,58.6336996313561));
#43402=CARTESIAN_POINT('Ctrl Pts',(72.2284115525991,56.3955638088267,59.0977760344396));
#43403=CARTESIAN_POINT('Ctrl Pts',(68.3809746809543,55.7590957801697,53.9882620695771));
#43404=CARTESIAN_POINT('Ctrl Pts',(70.610393675563,55.1226277515128,47.9801654008882));
#43405=CARTESIAN_POINT('Ctrl Pts',(75.8135978038988,54.592237727632,46.8510784551353));
#43406=CARTESIAN_POINT('Ctrl Pts',(79.1304928053609,54.1679257085273,48.8682833122854));
#43407=CARTESIAN_POINT('Ctrl Pts',(81.1572714303364,53.7436136894227,52.1793369650948));
#43408=CARTESIAN_POINT('Ctrl Pts',(80.0432207441853,53.2132236655419,57.3857812028527));
#43409=CARTESIAN_POINT('Ctrl Pts',(74.0415897201263,52.576755636885,59.6325476982599));
#43410=CARTESIAN_POINT('Ctrl Pts',(68.9209822076985,51.9402876082281,55.7998877678607));
#43411=CARTESIAN_POINT('Ctrl Pts',(69.366627711221,51.303819579571,49.4193467623025));
#43412=CARTESIAN_POINT('Ctrl Pts',(74.9895092014814,50.6673515509142,46.3451414372926));
#43413=CARTESIAN_POINT('Ctrl Pts',(79.6582884415991,50.1369615270333,48.9045692911776));
#43414=CARTESIAN_POINT('Ctrl Pts',(80.8397982325435,49.7126495079288,52.6025339341049));
#43415=CARTESIAN_POINT('Ctrl Pts',(80.1988609091723,49.2883374888241,56.4313858813532));
#43416=CARTESIAN_POINT('Ctrl Pts',(75.94374536206,48.7579474649434,59.6317237092895));
#43417=CARTESIAN_POINT('Ctrl Pts',(69.9392623542817,48.1214794362863,57.3925902958604));
#43418=CARTESIAN_POINT('Ctrl Pts',(68.586398666995,47.4850114076294,51.1412173840883));
#43419=CARTESIAN_POINT('Ctrl Pts',(73.1067579250465,46.8485433789726,46.6161477032359));
#43420=CARTESIAN_POINT('Ctrl Pts',(79.3678606590281,46.2120753503155,47.9822103622522));
#43421=CARTESIAN_POINT('Ctrl Pts',(81.2144888369357,45.6816853264348,52.9760200206947));
#43422=CARTESIAN_POINT('Ctrl Pts',(79.6816674585669,45.2573733073301,56.5427224905476));
#43423=CARTESIAN_POINT('Ctrl Pts',(76.6870768176045,44.8330612882254,59.0132153117264));
#43424=CARTESIAN_POINT('Ctrl Pts',(71.3759252168139,44.3026712643447,58.6392645053152));
#43425=CARTESIAN_POINT('Ctrl Pts',(68.3108182107715,43.6662032356877,53.011418232064));
#43426=CARTESIAN_POINT('Ctrl Pts',(71.38860861019,43.0297352070309,47.4045376647909));
#43427=CARTESIAN_POINT('Ctrl Pts',(77.7686820139573,42.3932671783739,46.9522470491929));
#43428=CARTESIAN_POINT('Ctrl Pts',(81.6000330021679,41.7567991497169,52.0891998656953));
#43429=CARTESIAN_POINT('Ctrl Pts',(79.7196526810578,41.2264091258361,57.0703985547842));
#43430=CARTESIAN_POINT('Ctrl Pts',(76.2235906019975,40.8020971067315,58.7581360420116));
#43431=CARTESIAN_POINT('Ctrl Pts',(72.3427116734402,40.3777850876269,58.6597153718375));
#43432=CARTESIAN_POINT('Ctrl Pts',(68.5780159994796,39.8473950637461,54.8947137762651));
#43433=CARTESIAN_POINT('Ctrl Pts',(69.9542034117819,39.2109270350892,48.6358286646777));
#43434=CARTESIAN_POINT('Ctrl Pts',(75.9545145524023,38.5744590064322,46.4208411581293));
#43435=CARTESIAN_POINT('Ctrl Pts',(81.0680328638006,37.9379909777753,50.2629543679937));
#43436=CARTESIAN_POINT('Ctrl Pts',(80.5922501426276,37.3015229491183,56.6536636741718));
#43437=CARTESIAN_POINT('Ctrl Pts',(75.9062574854849,36.7711329252376,59.1814380607402));
#43438=CARTESIAN_POINT('Ctrl Pts',(72.1600433554254,36.3468209061329,58.1632103955392));
#43439=CARTESIAN_POINT('Ctrl Pts',(69.2945270519295,35.9225088870284,55.5441028756294));
#43440=CARTESIAN_POINT('Ctrl Pts',(68.9210078168386,35.3921188631475,50.232920906129));
#43441=CARTESIAN_POINT('Ctrl Pts',(74.06415063904,34.7556508344905,46.4098832991481));
#43442=CARTESIAN_POINT('Ctrl Pts',(80.046798772065,34.1191828058336,48.6721442820747));
#43443=CARTESIAN_POINT('Ctrl Pts',(81.3881113529965,33.4827147771767,54.9260058090179));
#43444=CARTESIAN_POINT('Ctrl Pts',(76.8383309368684,32.8462467485197,59.4389907192186));
#43445=CARTESIAN_POINT('Ctrl Pts',(71.6428867818201,32.315856724639,58.2747181720951));
#43446=CARTESIAN_POINT('Ctrl Pts',(69.4821850598707,31.8915447055342,55.0494622203846));
#43447=CARTESIAN_POINT('Ctrl Pts',(69.0361493130766,31.4672326864297,51.1930441929765));
#43448=CARTESIAN_POINT('Ctrl Pts',(72.23683288965,30.9368426625488,46.9381887117852));
#43449=CARTESIAN_POINT('Ctrl Pts',(78.6267643192226,30.300374633892,47.4243069712248));
#43450=CARTESIAN_POINT('Ctrl Pts',(81.6602206610601,29.663906605235,53.0552967678677));
#43451=CARTESIAN_POINT('Ctrl Pts',(78.5720773534861,29.0274385765781,58.656481846159));
#43452=CARTESIAN_POINT('Ctrl Pts',(72.1777153698012,28.390970547921,59.0803562311091));
#43453=CARTESIAN_POINT('Ctrl Pts',(69.0186144497526,27.8605805240404,54.7945363502979));
#43454=CARTESIAN_POINT('Ctrl Pts',(69.5021802408798,27.4362685049357,50.9426443760508));
#43455=CARTESIAN_POINT('Ctrl Pts',(71.6941849048853,27.0119564858311,47.7385807280143));
#43456=CARTESIAN_POINT('Ctrl Pts',(76.9007196229027,26.4815664619503,46.6249532342245));
#43457=CARTESIAN_POINT('Ctrl Pts',(81.4063399869758,25.8450984332934,51.1820266495584));
#43458=CARTESIAN_POINT('Ctrl Pts',(80.0041950242122,25.2086304046363,57.4225313004325));
#43459=CARTESIAN_POINT('Ctrl Pts',(73.9998023159127,24.5721623759795,59.6264292760001));
#43460=CARTESIAN_POINT('Ctrl Pts',(68.8941291625674,23.9356943473224,55.7534939551535));
#43461=CARTESIAN_POINT('Ctrl Pts',(69.3193479845805,23.4053043234418,50.4461981309576));
#43462=CARTESIAN_POINT('Ctrl Pts',(72.2102306645205,22.980992304337,47.855121298611));
#43463=CARTESIAN_POINT('Ctrl Pts',(75.9661837218133,22.5566802852325,46.8734120501945));
#43464=CARTESIAN_POINT('Ctrl Pts',(80.6273366580689,22.0262902613516,49.4467132607705));
#43465=CARTESIAN_POINT('Ctrl Pts',(81.0408753299635,21.3898222326947,55.8417203460487));
#43466=CARTESIAN_POINT('Ctrl Pts',(75.890175270785,20.7533542040378,59.633916297922));
#43467=CARTESIAN_POINT('Ctrl Pts',(69.9117395951546,20.1168861753808,57.3605004391449));
#43468=CARTESIAN_POINT('Ctrl Pts',(68.5965174256227,19.4804181467239,51.0887193976995));
#43469=CARTESIAN_POINT('Ctrl Pts',(72.3977774992468,18.9500281228431,47.3601749200438));
#43470=CARTESIAN_POINT('Ctrl Pts',(76.2793092635613,18.5257161037384,47.3001117920513));
#43471=CARTESIAN_POINT('Ctrl Pts',(79.7590102216015,18.1014040846339,49.0207049813434));
#43472=CARTESIAN_POINT('Ctrl Pts',(81.5902691230174,17.571014060753,54.0224279611908));
#43473=CARTESIAN_POINT('Ctrl Pts',(77.7100437690878,16.9345460320961,59.1173659193523));
#43474=CARTESIAN_POINT('Ctrl Pts',(71.3329561213306,16.2980780034392,58.6109033270751));
#43475=CARTESIAN_POINT('Ctrl Pts',(68.3132228555609,15.6616099747823,52.9593291895844));
#43476=CARTESIAN_POINT('Ctrl Pts',(70.9069467681505,15.1312199509014,48.3199922132729));
#43477=CARTESIAN_POINT('Ctrl Pts',(74.6274753532391,14.7069079317968,47.1607194514));
#43478=CARTESIAN_POINT('Ctrl Pts',(76.5255413238862,14.4947519222445,47.5119870517647));
#43479=CARTESIAN_POINT('Ctrl Pts',(77.3774496940034,14.3886739174683,47.9101420920371));
#43480=CARTESIAN_POINT('',(70.0990315389018,416.,55.8419543693127));
#43481=CARTESIAN_POINT('Ctrl Pts',(70.0990315389037,416.,55.841954369316));
#43482=CARTESIAN_POINT('Ctrl Pts',(69.6292862985721,415.893921995224,55.0273288624995));
#43483=CARTESIAN_POINT('Ctrl Pts',(69.1165406058533,415.681765985672,53.1663787797211));
#43484=CARTESIAN_POINT('Ctrl Pts',(69.9524819678234,415.257453966567,49.3601406988557));
#43485=CARTESIAN_POINT('Ctrl Pts',(74.352298526842,414.727063942686,46.3781169629522));
#43486=CARTESIAN_POINT('Ctrl Pts',(79.5853747435743,414.161555332607,48.6206713789087));
#43487=CARTESIAN_POINT('Ctrl Pts',(80.618334511065,413.808202732081,51.7724009204073));
#43488=CARTESIAN_POINT('Ctrl Pts',(80.6269259201534,413.667006141107,53.0266694084182));
#43489=CARTESIAN_POINT('Ctrl Pts',(67.799287262509,416.,49.6622531841046));
#43490=CARTESIAN_POINT('Ctrl Pts',(67.7727972152803,416.,49.8439307127705));
#43491=CARTESIAN_POINT('Ctrl Pts',(67.7532000446317,416.,50.0264066333373));
#43492=CARTESIAN_POINT('Ctrl Pts',(67.7404788167283,416.,50.2092880641438));
#43493=CARTESIAN_POINT('Ctrl Pts',(67.7278723972532,416.,50.3905189994324));
#43494=CARTESIAN_POINT('Ctrl Pts',(67.7220188772554,416.,50.5721488441017));
#43495=CARTESIAN_POINT('Ctrl Pts',(67.7229416225055,416.,50.753763833248));
#43496=CARTESIAN_POINT('Ctrl Pts',(67.7238504120265,416.,50.9326320517298));
#43497=CARTESIAN_POINT('Ctrl Pts',(67.7313325809072,416.,51.1114863999918));
#43498=CARTESIAN_POINT('Ctrl Pts',(67.7454415376628,416.,51.2898920110631));
#43499=CARTESIAN_POINT('Ctrl Pts',(67.7591628710778,416.,51.463396183982));
#43500=CARTESIAN_POINT('Ctrl Pts',(67.7791524196438,416.,51.6364762550094));
#43501=CARTESIAN_POINT('Ctrl Pts',(67.805480958599,416.,51.808688414873));
#43502=CARTESIAN_POINT('Ctrl Pts',(67.8234105205741,416.,51.9259637638168));
#43503=CARTESIAN_POINT('Ctrl Pts',(67.8442802475463,416.,52.0428357113456));
#43504=CARTESIAN_POINT('Ctrl Pts',(67.8681165251726,416.,52.1591508831993));
#43505=CARTESIAN_POINT('Ctrl Pts',(67.8875438715047,416.,52.2539515547932));
#43506=CARTESIAN_POINT('Ctrl Pts',(67.9089419096746,416.,52.3483821840596));
#43507=CARTESIAN_POINT('Ctrl Pts',(67.9323259532379,416.,52.442353961058));
#43508=CARTESIAN_POINT('Ctrl Pts',(67.9395750602858,416.,52.4714854270979));
#43509=CARTESIAN_POINT('Ctrl Pts',(67.9470155216451,416.,52.5005743522527));
#43510=CARTESIAN_POINT('Ctrl Pts',(67.9546422512565,416.,52.5295976798077));
#43511=CARTESIAN_POINT('Ctrl Pts',(67.9964865806882,416.,52.688835222149));
#43512=CARTESIAN_POINT('Ctrl Pts',(68.0439703007979,416.,52.8462431417993));
#43513=CARTESIAN_POINT('Ctrl Pts',(68.0971152503823,416.,53.0014558004715));
#43514=CARTESIAN_POINT('Ctrl Pts',(68.1180500535734,416.,53.0625970093256));
#43515=CARTESIAN_POINT('Ctrl Pts',(68.1398635694756,416.,53.1233970689567));
#43516=CARTESIAN_POINT('Ctrl Pts',(68.1625579867857,416.,53.1838315598754));
#43517=CARTESIAN_POINT('Ctrl Pts',(68.2193464906623,416.,53.3350574880378));
#43518=CARTESIAN_POINT('Ctrl Pts',(68.2816503057749,416.,53.4839978932803));
#43519=CARTESIAN_POINT('Ctrl Pts',(68.349429310753,416.,53.630304289414));
#43520=CARTESIAN_POINT('Ctrl Pts',(68.416111980046,416.,53.7742441574007));
#43521=CARTESIAN_POINT('Ctrl Pts',(68.48809477141,416.,53.9156346722019));
#43522=CARTESIAN_POINT('Ctrl Pts',(68.5653421937902,416.,54.0540943533638));
#43523=CARTESIAN_POINT('Ctrl Pts',(68.6136238378459,416.,54.1406352480104));
#43524=CARTESIAN_POINT('Ctrl Pts',(68.6639621726723,416.,54.2260301943717));
#43525=CARTESIAN_POINT('Ctrl Pts',(68.7163474154008,416.,54.3101756515064));
#43526=CARTESIAN_POINT('Ctrl Pts',(68.7407921608684,416.,54.3494407989942));
#43527=CARTESIAN_POINT('Ctrl Pts',(68.7656825950477,416.,54.3884337573348));
#43528=CARTESIAN_POINT('Ctrl Pts',(68.7910175880391,416.,54.4271433901568));
#43529=CARTESIAN_POINT('Ctrl Pts',(68.8059692190121,416.,54.4499881624151));
#43530=CARTESIAN_POINT('Ctrl Pts',(68.8210705916636,416.,54.4727264570017));
#43531=CARTESIAN_POINT('Ctrl Pts',(68.8363201371293,416.,54.4953546820925));
#43532=CARTESIAN_POINT('Ctrl Pts',(68.9295715007333,416.,54.6337268618015));
#43533=CARTESIAN_POINT('Ctrl Pts',(69.0283775975531,416.,54.768007608802));
#43534=CARTESIAN_POINT('Ctrl Pts',(69.1326128816522,416.,54.8977087194485));
#43535=CARTESIAN_POINT('Ctrl Pts',(69.2033921426718,416.,54.9857801325435));
#43536=CARTESIAN_POINT('Ctrl Pts',(69.2766745528862,416.,55.0717387231204));
#43537=CARTESIAN_POINT('Ctrl Pts',(69.3524152746615,416.,55.1554160240979));
#43538=CARTESIAN_POINT('Ctrl Pts',(69.4007152851134,416.,55.2087772070529));
#43539=CARTESIAN_POINT('Ctrl Pts',(69.4500142507147,416.,55.2612100391359));
#43540=CARTESIAN_POINT('Ctrl Pts',(69.5003120398134,416.,55.312680490538));
#43541=CARTESIAN_POINT('Ctrl Pts',(69.5475874334726,416.,55.3610580811928));
#43542=CARTESIAN_POINT('Ctrl Pts',(69.5957454872076,416.,55.4085849866432));
#43543=CARTESIAN_POINT('Ctrl Pts',(69.6447558924706,416.,55.4552025719907));
#43544=CARTESIAN_POINT('Ctrl Pts',(69.7553610612021,416.,55.5604076986479));
#43545=CARTESIAN_POINT('Ctrl Pts',(69.8703283582921,416.,55.6610034002696));
#43546=CARTESIAN_POINT('Ctrl Pts',(69.9894762648668,416.,55.7564943579827));
#43547=CARTESIAN_POINT('Ctrl Pts',(70.0256123701293,416.,55.7854555995079));
#43548=CARTESIAN_POINT('Ctrl Pts',(70.0621327420081,416.,55.8139470646645));
#43549=CARTESIAN_POINT('Ctrl Pts',(70.0990315389037,416.,55.841954369316));
#43550=CARTESIAN_POINT('Origin',(74.9879498948689,423.667006141107,53.0228109606356));
#43551=CARTESIAN_POINT('',(79.8830110631917,416.,55.8460953909508));
#43552=CARTESIAN_POINT('Ctrl Pts',(79.8830110631917,416.,55.8460953909508));
#43553=CARTESIAN_POINT('Ctrl Pts',(79.8459760618144,415.991619351292,55.9103951483955));
#43554=CARTESIAN_POINT('Ctrl Pts',(78.8362070251561,415.771082693031,57.5815756537791));
#43555=CARTESIAN_POINT('Ctrl Pts',(75.0514316659349,415.338390025218,59.6975379999433));
#43556=CARTESIAN_POINT('Ctrl Pts',(69.3998575284373,414.701921996561,56.6778047341864));
#43557=CARTESIAN_POINT('Ctrl Pts',(68.8933949361463,414.065453967904,50.30071708643));
#43558=CARTESIAN_POINT('Ctrl Pts',(73.9883328942991,413.428985939247,46.4204917324893));
#43559=CARTESIAN_POINT('Ctrl Pts',(78.9900558741506,412.898595915367,48.2517506338942));
#43560=CARTESIAN_POINT('Ctrl Pts',(80.4714786825846,412.533265221915,51.2477571262032));
#43561=CARTESIAN_POINT('Ctrl Pts',(80.6285029194401,412.380090538016,52.6086444510753));
#43562=CARTESIAN_POINT('Ctrl Pts',(80.6310716108719,412.332993858894,53.0264521482468));
#43563=CARTESIAN_POINT('Origin',(74.9879498948689,416.,53.0228109606356));
#43564=CARTESIAN_POINT('Origin',(74.9879498948689,455.,53.0228109606356));
#43565=CARTESIAN_POINT('Ctrl Pts',(78.8686068361685,455.,50.1705810192551));
#43566=CARTESIAN_POINT('Ctrl Pts',(78.7971362865198,455.,50.0496527591843));
#43567=CARTESIAN_POINT('Ctrl Pts',(78.7205501200313,455.,49.9320764112506));
#43568=CARTESIAN_POINT('Ctrl Pts',(78.6391280567385,455.,49.8181536474318));
#43569=CARTESIAN_POINT('Ctrl Pts',(78.5567895823215,455.,49.7029486747886));
#43570=CARTESIAN_POINT('Ctrl Pts',(78.4695055308971,455.,49.5914792507712));
#43571=CARTESIAN_POINT('Ctrl Pts',(78.3775130294169,455.,49.4840669138619));
#43572=CARTESIAN_POINT('Ctrl Pts',(78.3375958441137,455.,49.4374587872508));
#43573=CARTESIAN_POINT('Ctrl Pts',(78.2967914896971,455.,49.3916147355805));
#43574=CARTESIAN_POINT('Ctrl Pts',(78.2551164948957,455.,49.3465621292919));
#43575=CARTESIAN_POINT('',(79.722466405091,455.,53.9090580914827));
#43576=CARTESIAN_POINT('Origin',(74.9879498948689,455.,53.0228109606356));
#43577=CARTESIAN_POINT('Ctrl Pts',(79.5259634687995,455.,54.9172708347116));
#43578=CARTESIAN_POINT('Ctrl Pts',(79.5671055435192,455.,54.7833057439901));
#43579=CARTESIAN_POINT('Ctrl Pts',(79.6025381242703,455.,54.6476488793227));
#43580=CARTESIAN_POINT('Ctrl Pts',(79.6320742294025,455.,54.5106387216536));
#43581=CARTESIAN_POINT('Ctrl Pts',(79.6610001784902,455.,54.3764589160396));
#43582=CARTESIAN_POINT('Ctrl Pts',(79.6842707237605,455.,54.2409805184599));
#43583=CARTESIAN_POINT('Ctrl Pts',(79.7016610667469,455.,54.1045284674012));
#43584=CARTESIAN_POINT('Ctrl Pts',(79.7099385218545,455.,54.0395800228609));
#43585=CARTESIAN_POINT('Ctrl Pts',(79.7168830527446,455.,53.9744111521296));
#43586=CARTESIAN_POINT('Ctrl Pts',(79.722466405091,455.,53.9090580914828));
#43587=CARTESIAN_POINT('Ctrl Pts',(75.8078350467992,437.941398947677,48.2763523965962));
#43588=CARTESIAN_POINT('Ctrl Pts',(75.0263656302742,437.987255402119,48.1413643496868));
#43589=CARTESIAN_POINT('Ctrl Pts',(73.3961753647049,438.078968311002,48.2651239894432));
#43590=CARTESIAN_POINT('Ctrl Pts',(71.3306174890971,438.216537674327,49.5884496895898));
#43591=CARTESIAN_POINT('Ctrl Pts',(70.1396312756662,438.354107037653,51.7327415034739));
#43592=CARTESIAN_POINT('Ctrl Pts',(70.1074607270008,438.491676400978,54.1854768655665));
#43593=CARTESIAN_POINT('Ctrl Pts',(71.242010804005,438.629245764303,56.360277322365));
#43594=CARTESIAN_POINT('Ctrl Pts',(73.2719781460082,438.766815127628,57.7372832840433));
#43595=CARTESIAN_POINT('Ctrl Pts',(75.7121534069691,438.904384490953,57.9873162880474));
#43596=CARTESIAN_POINT('Ctrl Pts',(77.9792050969341,439.041953854279,57.0506108876648));
#43597=CARTESIAN_POINT('Ctrl Pts',(79.5312149397283,439.179523217604,55.1510795096557));
#43598=CARTESIAN_POINT('Ctrl Pts',(79.9971786085583,439.317092580929,52.7427964908572));
#43599=CARTESIAN_POINT('Ctrl Pts',(79.2657116989475,439.454661944254,50.4014494245561));
#43600=CARTESIAN_POINT('Ctrl Pts',(77.5116668773773,439.592231307579,48.6867258388772));
#43601=CARTESIAN_POINT('Ctrl Pts',(75.1543402086109,439.729800670904,48.0085217694175));
#43602=CARTESIAN_POINT('Ctrl Pts',(72.7572387087512,439.86737003423,48.5289585575719));
#43603=CARTESIAN_POINT('Ctrl Pts',(70.8933776271112,440.004939397555,50.1236283637003));
#43604=CARTESIAN_POINT('Ctrl Pts',(70.0083036305712,440.14250876088,52.4113333252207));
#43605=CARTESIAN_POINT('Ctrl Pts',(70.3135892642953,440.280078124205,54.8452089672548));
#43606=CARTESIAN_POINT('Ctrl Pts',(71.7362575112132,440.41764748753,56.8434494476892));
#43607=CARTESIAN_POINT('Ctrl Pts',(73.9362266197783,440.555216850856,57.9283853364634));
#43608=CARTESIAN_POINT('Ctrl Pts',(76.387604935838,440.692786214181,57.8406681161432));
#43609=CARTESIAN_POINT('Ctrl Pts',(78.5044026893045,440.830355577506,56.6012661509721));
#43610=CARTESIAN_POINT('Ctrl Pts',(79.7806099252566,440.967924940831,54.5064523046412));
#43611=CARTESIAN_POINT('Ctrl Pts',(79.9111556636527,441.105494304156,52.0569813882592));
#43612=CARTESIAN_POINT('Ctrl Pts',(78.8648335961934,441.243063667482,49.8383872182613));
#43613=CARTESIAN_POINT('Ctrl Pts',(76.8917617991304,441.380633030807,48.3810136753364));
#43614=CARTESIAN_POINT('Ctrl Pts',(74.4635932533763,441.518202394132,48.0332386425771));
#43615=CARTESIAN_POINT('Ctrl Pts',(72.1607695498123,441.655771757457,48.8781960085396));
#43616=CARTESIAN_POINT('Ctrl Pts',(70.5337692194001,441.793341120782,50.713902925461));
#43617=CARTESIAN_POINT('Ctrl Pts',(69.9715185834993,441.930910484107,53.101542802499));
#43618=CARTESIAN_POINT('Ctrl Pts',(70.6084208548284,442.068479847433,55.4703622250742));
#43619=CARTESIAN_POINT('Ctrl Pts',(72.2922277192217,442.206049210758,57.2541067144605));
#43620=CARTESIAN_POINT('Ctrl Pts',(74.6204335364492,442.343618574083,58.0263810391802));
#43621=CARTESIAN_POINT('Ctrl Pts',(77.0364923077588,442.481187937408,57.6025768702869));
#43622=CARTESIAN_POINT('Ctrl Pts',(78.9628572235115,442.618757300733,56.0840024824643));
#43623=CARTESIAN_POINT('Ctrl Pts',(79.9390403500092,442.756326664059,53.8336655158004));
#43624=CARTESIAN_POINT('Ctrl Pts',(79.7316899753536,442.893896027384,51.389497808354));
#43625=CARTESIAN_POINT('Ctrl Pts',(78.390372173343,443.031465390709,49.335765470876));
#43626=CARTESIAN_POINT('Ctrl Pts',(76.2357222805272,443.169034754034,48.1634029845338));
#43627=CARTESIAN_POINT('Ctrl Pts',(73.7827986167874,443.306604117359,48.1526577596006));
#43628=CARTESIAN_POINT('Ctrl Pts',(71.6179603605938,443.444173480684,49.3060983885513));
#43629=CARTESIAN_POINT('Ctrl Pts',(70.2587013093226,443.581742844009,51.3480006368313));
#43630=CARTESIAN_POINT('Ctrl Pts',(70.0299455657551,443.719312207335,53.7902579471445));
#43631=CARTESIAN_POINT('Ctrl Pts',(70.9863760504612,443.85688157066,56.049060879655));
#43632=CARTESIAN_POINT('Ctrl Pts',(72.8993628221321,443.994450933985,57.5844538493555));
#43633=CARTESIAN_POINT('Ctrl Pts',(75.3116159257467,444.13202029731,58.0294088179703));
#43634=CARTESIAN_POINT('Ctrl Pts',(77.6464982775643,444.269589660636,57.2775615175402));
#43635=CARTESIAN_POINT('Ctrl Pts',(79.3458678865093,444.407159023961,55.5086372986467));
#43636=CARTESIAN_POINT('Ctrl Pts',(80.0034989158186,444.544728387286,53.1454886809583));
#43637=CARTESIAN_POINT('Ctrl Pts',(79.4621879450261,444.682297750611,50.7530145655511));
#43638=CARTESIAN_POINT('Ctrl Pts',(77.8513326642527,444.819867113936,48.9031239675973));
#43639=CARTESIAN_POINT('Ctrl Pts',(75.5560000011943,444.957436477261,48.0380240162099));
#43640=CARTESIAN_POINT('Ctrl Pts',(73.1248777909117,445.095005840587,48.364512543824));
#43641=CARTESIAN_POINT('Ctrl Pts',(71.1391136830664,445.232575203912,49.8045440948628));
#43642=CARTESIAN_POINT('Ctrl Pts',(70.07339469223,445.370144567237,52.0138863029791));
#43643=CARTESIAN_POINT('Ctrl Pts',(70.1824756324979,445.507713930562,54.4644069228604));
#43644=CARTESIAN_POINT('Ctrl Pts',(71.4402812486687,445.645283293887,56.5703212116962));
#43645=CARTESIAN_POINT('Ctrl Pts',(73.5461393760615,445.782852657213,57.8282208528788));
#43646=CARTESIAN_POINT('Ctrl Pts',(75.9966551231817,445.920422020538,57.9374112055169));
#43647=CARTESIAN_POINT('Ctrl Pts',(78.206044912028,446.057991383863,56.8717908599269));
#43648=CARTESIAN_POINT('Ctrl Pts',(79.6461651233516,446.195560747188,54.8860910495501));
#43649=CARTESIAN_POINT('Ctrl Pts',(79.9727621970059,446.333130110513,52.4549834189681));
#43650=CARTESIAN_POINT('Ctrl Pts',(79.1077647300243,446.470699473838,50.159612132638));
#43651=CARTESIAN_POINT('Ctrl Pts',(77.2579460564552,446.608268837164,48.5486742583212));
#43652=CARTESIAN_POINT('Ctrl Pts',(74.8654961122459,446.745838200489,48.0072564672885));
#43653=CARTESIAN_POINT('Ctrl Pts',(72.5023181345641,446.883407563814,48.6647819845069));
#43654=CARTESIAN_POINT('Ctrl Pts',(70.7333180428463,447.020976927139,50.3640726116498));
#43655=CARTESIAN_POINT('Ctrl Pts',(69.9813664937813,447.158546290464,52.6989213921604));
#43656=CARTESIAN_POINT('Ctrl Pts',(70.4262137580673,447.29611565379,55.1111943600169));
#43657=CARTESIAN_POINT('Ctrl Pts',(71.9615213139283,447.433685017115,57.0242496830301));
#43658=CARTESIAN_POINT('Ctrl Pts',(74.2202815408413,447.57125438044,57.9807810193227));
#43659=CARTESIAN_POINT('Ctrl Pts',(76.6625490623592,447.708823743765,57.7521343195162));
#43660=CARTESIAN_POINT('Ctrl Pts',(78.7045119977084,447.84639310709,56.3929664378131));
#43661=CARTESIAN_POINT('Ctrl Pts',(79.8580492826516,447.983962470415,54.2281796833637));
#43662=CARTESIAN_POINT('Ctrl Pts',(79.8474135775007,448.121531833741,51.775255542309));
#43663=CARTESIAN_POINT('Ctrl Pts',(78.6751472945723,448.259101197066,49.6205533072187));
#43664=CARTESIAN_POINT('Ctrl Pts',(76.6214748471931,448.396670560391,48.2791438101341));
#43665=CARTESIAN_POINT('Ctrl Pts',(74.1773164001007,448.534239923716,48.0716843068553));
#43666=CARTESIAN_POINT('Ctrl Pts',(71.9269358504046,448.671809287042,49.0477669578345));
#43667=CARTESIAN_POINT('Ctrl Pts',(70.4082754544702,448.809378650367,50.9740640693451));
#43668=CARTESIAN_POINT('Ctrl Pts',(69.9843634121962,448.946948013692,53.3901039159554));
#43669=CARTESIAN_POINT('Ctrl Pts',(70.7565337848602,449.084517377017,55.7183442118813));
#43670=CARTESIAN_POINT('Ctrl Pts',(72.5402030927367,449.222086740342,57.4022307164097));
#43671=CARTESIAN_POINT('Ctrl Pts',(74.9089940761134,449.359656103667,58.0392387517333));
#43672=CARTESIAN_POINT('Ctrl Pts',(77.2966590545129,449.497225466993,57.4770947213303));
#43673=CARTESIAN_POINT('Ctrl Pts',(79.1324386130003,449.634794830318,55.8501763544067));
#43674=CARTESIAN_POINT('Ctrl Pts',(79.9774987961291,449.772364193643,53.5473903793574));
#43675=CARTESIAN_POINT('Ctrl Pts',(79.6298321782047,449.909933556968,51.1192063083334));
#43676=CARTESIAN_POINT('Ctrl Pts',(78.1725467317586,450.047502920293,49.1460694434481));
#43677=CARTESIAN_POINT('Ctrl Pts',(75.9539992808559,450.185072283618,48.0996483197667));
#43678=CARTESIAN_POINT('Ctrl Pts',(73.5045225382257,450.322641646944,48.2300846924063));
#43679=CARTESIAN_POINT('Ctrl Pts',(71.4096517130236,450.460211010268,49.5061983964745));
#43680=CARTESIAN_POINT('Ctrl Pts',(70.1701552369073,450.597780373594,51.6229408101112));
#43681=CARTESIAN_POINT('Ctrl Pts',(70.0823285658649,450.735349736919,54.0743152074334));
#43682=CARTESIAN_POINT('Ctrl Pts',(71.1671662279536,450.872919100245,56.2743327543879));
#43683=CARTESIAN_POINT('Ctrl Pts',(73.1653431859865,451.01048846357,57.6970902194464));
#43684=CARTESIAN_POINT('Ctrl Pts',(75.5992051954103,451.148057826895,58.0024845204358));
#43685=CARTESIAN_POINT('Ctrl Pts',(77.8869496712317,451.28562719022,57.1175126715371));
#43686=CARTESIAN_POINT('Ctrl Pts',(79.4817026967351,451.423196553545,55.2537227832616));
#43687=CARTESIAN_POINT('Ctrl Pts',(80.0022465081079,451.56076591687,52.8566445408086));
#43688=CARTESIAN_POINT('Ctrl Pts',(79.3241477011989,451.698335280195,50.4992875529827));
#43689=CARTESIAN_POINT('Ctrl Pts',(77.6095024167226,451.835904643521,48.7451662605903));
#43690=CARTESIAN_POINT('Ctrl Pts',(75.268188065539,451.973474006846,48.0135946175118));
#43691=CARTESIAN_POINT('Ctrl Pts',(72.8598841761585,452.111043370171,48.4794511794175));
#43692=CARTESIAN_POINT('Ctrl Pts',(70.9602837922551,452.248612733496,50.0313752567566));
#43693=CARTESIAN_POINT('Ctrl Pts',(70.0234769197435,452.386182096821,52.2983871320682));
#43694=CARTESIAN_POINT('Ctrl Pts',(70.2734025728211,452.523751460147,54.7385689140928));
#43695=CARTESIAN_POINT('Ctrl Pts',(71.6503172704237,452.661320823472,56.768607306331));
#43696=CARTESIAN_POINT('Ctrl Pts',(73.8250764135404,452.798890186797,57.9032317501341));
#43697=CARTESIAN_POINT('Ctrl Pts',(76.2778146704519,452.936459550122,57.8712159196889));
#43698=CARTESIAN_POINT('Ctrl Pts',(78.4222171738024,453.074028913447,56.6802130540946));
#43699=CARTESIAN_POINT('Ctrl Pts',(79.7456752114561,453.211598276772,54.6149264217687));
#43700=CARTESIAN_POINT('Ctrl Pts',(79.9318226886387,453.349167640098,52.1690525697788));
#43701=CARTESIAN_POINT('Ctrl Pts',(78.9361620760772,453.486737003423,49.9272653015586));
#43702=CARTESIAN_POINT('Ctrl Pts',(76.9967008584153,453.624306366748,48.4254530263665));
#43703=CARTESIAN_POINT('Ctrl Pts',(74.5770580405339,453.761875730073,48.0226157475833));
#43704=CARTESIAN_POINT('Ctrl Pts',(72.2556360896412,453.899445093398,48.8150513185195));
#43705=CARTESIAN_POINT('Ctrl Pts',(70.5873615618629,454.037014456724,50.6133284028548));
#43706=CARTESIAN_POINT('Ctrl Pts',(69.9710218005993,454.174583820049,52.9875855721569));
#43707=CARTESIAN_POINT('Ctrl Pts',(70.5539601059199,454.312153183374,55.370251255858));
#43708=CARTESIAN_POINT('Ctrl Pts',(72.1968012676347,454.449722546699,57.1917983514602));
#43709=CARTESIAN_POINT('Ctrl Pts',(74.5068799898513,454.587291910024,58.0167116789214));
#43710=CARTESIAN_POINT('Ctrl Pts',(76.9318483449357,454.724861273349,57.6479786853993));
#43711=CARTESIAN_POINT('Ctrl Pts',(78.8922444243951,454.862430636675,56.1733372178574));
#43712=CARTESIAN_POINT('Ctrl Pts',(79.5765523475053,454.954143545558,54.6885613368712));
#43713=CARTESIAN_POINT('Ctrl Pts',(79.7224664050908,455.,53.9090580914826));
#43714=CARTESIAN_POINT('Ctrl Pts',(75.8135940020368,437.960932631785,48.2430127973331));
#43715=CARTESIAN_POINT('Ctrl Pts',(75.0266354662385,438.006789086226,48.1070765808929));
#43716=CARTESIAN_POINT('Ctrl Pts',(73.3849945813404,438.09850199511,48.2317055207262));
#43717=CARTESIAN_POINT('Ctrl Pts',(71.304928020805,438.236071358435,49.5643263928294));
#43718=CARTESIAN_POINT('Ctrl Pts',(70.1055762011968,438.37364072176,51.7236799266913));
#43719=CARTESIAN_POINT('Ctrl Pts',(70.0731796833828,438.511210085085,54.1936435470669));
#43720=CARTESIAN_POINT('Ctrl Pts',(71.2156989535025,438.648779448411,56.3837200195998));
#43721=CARTESIAN_POINT('Ctrl Pts',(73.2599249889687,438.786348811736,57.7703982087559));
#43722=CARTESIAN_POINT('Ctrl Pts',(75.7172402848071,438.923918175061,58.0221874695656));
#43723=CARTESIAN_POINT('Ctrl Pts',(78.0002159723868,439.061487538386,57.0789025568467));
#43724=CARTESIAN_POINT('Ctrl Pts',(79.5631272874079,439.199056901711,55.1660286806199));
#43725=CARTESIAN_POINT('Ctrl Pts',(80.0323639316109,439.336626265037,52.7408296412398));
#43726=CARTESIAN_POINT('Ctrl Pts',(79.2957591253323,439.474195628362,50.3830367191764));
#43727=CARTESIAN_POINT('Ctrl Pts',(77.5293937176552,439.611764991687,48.6562687436809));
#43728=CARTESIAN_POINT('Ctrl Pts',(75.1555089508019,439.749334355012,47.973300901065));
#43729=CARTESIAN_POINT('Ctrl Pts',(72.741569970467,439.886903718337,48.4973932892262));
#43730=CARTESIAN_POINT('Ctrl Pts',(70.8646169423356,440.024473081663,50.1032642154267));
#43731=CARTESIAN_POINT('Ctrl Pts',(69.9733260975992,440.162042444988,52.4070382452052));
#43732=CARTESIAN_POINT('Ctrl Pts',(70.2807560881215,440.299611808313,54.8580096729639));
#43733=CARTESIAN_POINT('Ctrl Pts',(71.7134172989717,440.437181171638,56.8702859942152));
#43734=CARTESIAN_POINT('Ctrl Pts',(73.9288392103963,440.574750534963,57.9628425810889));
#43735=CARTESIAN_POINT('Ctrl Pts',(76.3974362527121,440.712319898288,57.8745092262476));
#43736=CARTESIAN_POINT('Ctrl Pts',(78.5291026051286,440.849889261614,56.6264015778208));
#43737=CARTESIAN_POINT('Ctrl Pts',(79.8142740482362,440.987458624939,54.5168735497005));
#43738=CARTESIAN_POINT('Ctrl Pts',(79.9457367529441,441.125027988264,52.0501973048284));
#43739=CARTESIAN_POINT('Ctrl Pts',(78.892065214725,441.262597351589,49.8160195076783));
#43740=CARTESIAN_POINT('Ctrl Pts',(76.9051343641921,441.400166714914,48.3484092273538));
#43741=CARTESIAN_POINT('Ctrl Pts',(74.459910119928,441.53773607824,47.9981913880117));
#43742=CARTESIAN_POINT('Ctrl Pts',(72.1409111525511,441.675305441565,48.8490838189484));
#43743=CARTESIAN_POINT('Ctrl Pts',(70.5024826092334,441.81287480489,50.6976849246948));
#43744=CARTESIAN_POINT('Ctrl Pts',(69.9362826686808,441.950444168215,53.1020958228239));
#43745=CARTESIAN_POINT('Ctrl Pts',(70.5776586052088,442.08801353154,55.4875540697372));
#43746=CARTESIAN_POINT('Ctrl Pts',(72.2732926972788,442.225582894866,57.2838277586649));
#43747=CARTESIAN_POINT('Ctrl Pts',(74.6178520648221,442.363152258191,58.0615266154141));
#43748=CARTESIAN_POINT('Ctrl Pts',(77.0508814743759,442.500721621516,57.6347456036881));
#43749=CARTESIAN_POINT('Ctrl Pts',(78.9907773697968,442.638290984841,56.1055045976158));
#43750=CARTESIAN_POINT('Ctrl Pts',(79.9738173041241,442.775860348166,53.8393610392238));
#43751=CARTESIAN_POINT('Ctrl Pts',(79.7650104797166,442.913429711491,51.3780252535568));
#43752=CARTESIAN_POINT('Ctrl Pts',(78.4142711274279,443.050999074817,49.3098672949128));
#43753=CARTESIAN_POINT('Ctrl Pts',(76.2444867584528,443.188568438142,48.1292700173134));
#43754=CARTESIAN_POINT('Ctrl Pts',(73.7743335137805,443.326137801467,48.1184493168465));
#43755=CARTESIAN_POINT('Ctrl Pts',(71.5942892173451,443.463707164792,49.2799918280372));
#43756=CARTESIAN_POINT('Ctrl Pts',(70.2254825946682,443.601276528117,51.3362366017546));
#43757=CARTESIAN_POINT('Ctrl Pts',(69.9951200478985,443.738845891443,53.795648571468));
#43758=CARTESIAN_POINT('Ctrl Pts',(70.9582685959045,443.876415254768,56.0703175614966));
#43759=CARTESIAN_POINT('Ctrl Pts',(72.8846923778225,444.013984618093,57.6164952848467));
#43760=CARTESIAN_POINT('Ctrl Pts',(75.3138893882913,444.151553981418,58.064575661625));
#43761=CARTESIAN_POINT('Ctrl Pts',(77.6651721870708,444.289123344743,57.3074473106253));
#43762=CARTESIAN_POINT('Ctrl Pts',(79.3764783379654,444.426692708068,55.5260979912513));
#43763=CARTESIAN_POINT('Ctrl Pts',(80.038728633341,444.564262071394,53.1463503815249));
#43764=CARTESIAN_POINT('Ctrl Pts',(79.493615440197,444.701831434719,50.7370712888534));
#43765=CARTESIAN_POINT('Ctrl Pts',(77.8714453509601,444.839400798044,48.8741868744816));
#43766=CARTESIAN_POINT('Ctrl Pts',(75.5599900419058,444.976970161369,48.003010374587));
#43767=CARTESIAN_POINT('Ctrl Pts',(73.1117913862783,445.114539524694,48.3317921902448));
#43768=CARTESIAN_POINT('Ctrl Pts',(71.112079072904,445.25210888802,49.7819386667991));
#43769=CARTESIAN_POINT('Ctrl Pts',(70.0388743653796,445.389678251345,52.0067995153628));
#43770=CARTESIAN_POINT('Ctrl Pts',(70.1487215010723,445.52724761467,54.4745328369565));
#43771=CARTESIAN_POINT('Ctrl Pts',(71.4153620695824,445.664816977995,56.5952392781992));
#43772=CARTESIAN_POINT('Ctrl Pts',(73.5360119548985,445.80238634132,57.8619745321622));
#43773=CARTESIAN_POINT('Ctrl Pts',(76.0037403695044,445.939955704645,57.9719318487485));
#43774=CARTESIAN_POINT('Ctrl Pts',(78.2286491330098,446.07752506797,56.8988264793647));
#43775=CARTESIAN_POINT('Ctrl Pts',(79.6788848926077,446.215094431296,54.8991789150905));
#43776=CARTESIAN_POINT('Ctrl Pts',(80.0077760167439,446.352663794621,52.4509949415729));
#43777=CARTESIAN_POINT('Ctrl Pts',(79.1367027211158,446.490233157946,50.1395007379533));
#43778=CARTESIAN_POINT('Ctrl Pts',(77.2738907363328,446.627802521271,48.5172474750277));
#43779=CARTESIAN_POINT('Ctrl Pts',(74.8646359846401,446.765371884597,47.9720267113274));
#43780=CARTESIAN_POINT('Ctrl Pts',(72.4848588086928,446.902941247922,48.6341707534847));
#43781=CARTESIAN_POINT('Ctrl Pts',(70.7034330835562,447.040510611247,50.3453973678012));
#43782=CARTESIAN_POINT('Ctrl Pts',(69.9461997516687,447.178079974572,52.6966463594655));
#43783=CARTESIAN_POINT('Ctrl Pts',(70.3941716675923,447.315649337897,55.1258633737044));
#43784=CARTESIAN_POINT('Ctrl Pts',(71.9402633771475,447.453218701222,57.0523561884764));
#43785=CARTESIAN_POINT('Ctrl Pts',(74.2148893616102,447.590788064548,58.0156062964603));
#43786=CARTESIAN_POINT('Ctrl Pts',(76.6743116142528,447.728357427873,57.785353559386));
#43787=CARTESIAN_POINT('Ctrl Pts',(78.7306175013115,447.865926791198,56.4166387466614));
#43788=CARTESIAN_POINT('Ctrl Pts',(79.892257347416,448.003496154523,54.2366463137236));
#43789=CARTESIAN_POINT('Ctrl Pts',(79.8815469360093,448.141065517849,51.7664925883836));
#43790=CARTESIAN_POINT('Ctrl Pts',(78.7010465375661,448.278634881173,49.5966555094766));
#43791=CARTESIAN_POINT('Ctrl Pts',(76.6329488896949,448.416204244499,48.2458238180386));
#43792=CARTESIAN_POINT('Ctrl Pts',(74.1716224294276,448.553773607824,48.0369070984776));
#43793=CARTESIAN_POINT('Ctrl Pts',(71.9054349818719,448.691342971149,49.0198458515363));
#43794=CARTESIAN_POINT('Ctrl Pts',(70.3761073635582,448.828912334474,50.9596734664513));
#43795=CARTESIAN_POINT('Ctrl Pts',(69.9492177207381,448.9664816978,53.3926838183768));
#43796=CARTESIAN_POINT('Ctrl Pts',(70.7268118952619,449.104051061125,55.7372779068002));
#43797=CARTESIAN_POINT('Ctrl Pts',(72.5230098745974,449.24162042445,57.4329921984057));
#43798=CARTESIAN_POINT('Ctrl Pts',(74.9084394825524,449.379189787775,58.074474641825));
#43799=CARTESIAN_POINT('Ctrl Pts',(77.3128756583575,449.5167591511,57.508382055578));
#43800=CARTESIAN_POINT('Ctrl Pts',(79.1615499159115,449.654328514426,55.8700360514686));
#43801=CARTESIAN_POINT('Ctrl Pts',(80.0125458862126,449.791897877751,53.5510750776152));
#43802=CARTESIAN_POINT('Ctrl Pts',(79.6624372232219,449.929467241076,51.1058351990302));
#43803=CARTESIAN_POINT('Ctrl Pts',(78.1949156581748,450.067036604401,49.1188388236321));
#43804=CARTESIAN_POINT('Ctrl Pts',(75.9607849082795,450.204605967726,48.06506753341));
#43805=CARTESIAN_POINT('Ctrl Pts',(73.4941027962351,450.342175331051,48.1964201041654));
#43806=CARTESIAN_POINT('Ctrl Pts',(71.3845173890182,450.479744694376,49.4814973584119));
#43807=CARTESIAN_POINT('Ctrl Pts',(70.1363145657919,450.617314057702,51.6131079822862));
#43808=CARTESIAN_POINT('Ctrl Pts',(70.0478709914357,450.754883421027,54.0817010783388));
#43809=CARTESIAN_POINT('Ctrl Pts',(71.1403286616697,450.892452784352,56.2971717683888));
#43810=CARTESIAN_POINT('Ctrl Pts',(73.1525410143319,451.030022147677,57.7299228240568));
#43811=CARTESIAN_POINT('Ctrl Pts',(75.6034987137235,451.167591511002,58.0374622451341));
#43812=CARTESIAN_POINT('Ctrl Pts',(77.9073125353553,451.305160874328,57.1462742655343));
#43813=CARTESIAN_POINT('Ctrl Pts',(79.513267265472,451.442730237653,55.2693929308367));
#43814=CARTESIAN_POINT('Ctrl Pts',(80.0374674285935,451.580299600978,52.8554773712709));
#43815=CARTESIAN_POINT('Ctrl Pts',(79.3546055879029,451.717868964303,50.4815620723939));
#43816=CARTESIAN_POINT('Ctrl Pts',(77.6279164636054,451.855438327628,48.7151196567561));
#43817=CARTESIAN_POINT('Ctrl Pts',(75.2701564864537,451.993007690953,47.9784093813513));
#43818=CARTESIAN_POINT('Ctrl Pts',(72.8449364298946,452.130577054279,48.4475381663004));
#43819=CARTESIAN_POINT('Ctrl Pts',(70.9319930630693,452.268146417604,50.0103631134411));
#43820=CARTESIAN_POINT('Ctrl Pts',(69.9886059654709,452.405715780929,52.2932987067053));
#43821=CARTESIAN_POINT('Ctrl Pts',(70.2402871213106,452.543285144254,54.750620569412));
#43822=CARTESIAN_POINT('Ctrl Pts',(71.626873405343,452.68085450758,56.7949181541772));
#43823=CARTESIAN_POINT('Ctrl Pts',(73.8169082740026,452.818423870904,57.9375123134555));
#43824=CARTESIAN_POINT('Ctrl Pts',(76.2868748095306,452.95599323423,57.905271600618));
#43825=CARTESIAN_POINT('Ctrl Pts',(78.4463398103528,453.093562597555,56.7059030118799));
#43826=CARTESIAN_POINT('Ctrl Pts',(79.779093949515,453.23113196088,54.6261095998664));
#43827=CARTESIAN_POINT('Ctrl Pts',(79.9665489451789,453.368701324205,52.1630556855262));
#43828=CARTESIAN_POINT('Ctrl Pts',(78.9638947129792,453.50627068753,49.9055218795142));
#43829=CARTESIAN_POINT('Ctrl Pts',(77.0108105259159,453.643840050856,48.3931607248264));
#43830=CARTESIAN_POINT('Ctrl Pts',(74.574171895089,453.781409414181,47.9874938767418));
#43831=CARTESIAN_POINT('Ctrl Pts',(72.2364440444356,453.918978777506,48.7854955943157));
#43832=CARTESIAN_POINT('Ctrl Pts',(70.5564513896651,454.056548140831,50.5964039565915));
#43833=CARTESIAN_POINT('Ctrl Pts',(69.935782396328,454.194117504156,52.9873381455081));
#43834=CARTESIAN_POINT('Ctrl Pts',(70.5228153185577,454.331686867482,55.3867399110692));
#43835=CARTESIAN_POINT('Ctrl Pts',(72.17719596076,454.469256230807,57.2210817354965));
#43836=CARTESIAN_POINT('Ctrl Pts',(74.5035009067655,454.606825594132,58.0517893366026));
#43837=CARTESIAN_POINT('Ctrl Pts',(76.945502481901,454.744394957457,57.6804663256868));
#43838=CARTESIAN_POINT('Ctrl Pts',(78.9196685793232,454.881964320782,56.1954668291174));
#43839=CARTESIAN_POINT('Ctrl Pts',(79.6087831496676,454.973677229666,54.7002617339708));
#43840=CARTESIAN_POINT('Ctrl Pts',(79.7557221221745,455.019533684108,53.9152831798916));
#43841=CARTESIAN_POINT('Ctrl Pts',(75.8193529572743,437.980466315892,48.20967319807));
#43842=CARTESIAN_POINT('Ctrl Pts',(75.0269053022029,438.026322770334,48.0727888120991));
#43843=CARTESIAN_POINT('Ctrl Pts',(73.3738137979759,438.118035679217,48.1982870520092));
#43844=CARTESIAN_POINT('Ctrl Pts',(71.279238552513,438.255605042543,49.5402030960689));
#43845=CARTESIAN_POINT('Ctrl Pts',(70.0715211267274,438.393174405868,51.7146183499088));
#43846=CARTESIAN_POINT('Ctrl Pts',(70.0388986397648,438.530743769193,54.2018102285672));
#43847=CARTESIAN_POINT('Ctrl Pts',(71.189387103,438.668313132518,56.4071627168346));
#43848=CARTESIAN_POINT('Ctrl Pts',(73.2478718319292,438.805882495844,57.8035131334684));
#43849=CARTESIAN_POINT('Ctrl Pts',(75.7223271626451,438.943451859169,58.0570586510839));
#43850=CARTESIAN_POINT('Ctrl Pts',(78.0212268478395,439.081021222494,57.1071942260285));
#43851=CARTESIAN_POINT('Ctrl Pts',(79.5950396350873,439.218590585819,55.1809778515842));
#43852=CARTESIAN_POINT('Ctrl Pts',(80.0675492546636,439.356159949144,52.7388627916225));
#43853=CARTESIAN_POINT('Ctrl Pts',(79.325806551717,439.493729312469,50.3646240137967));
#43854=CARTESIAN_POINT('Ctrl Pts',(77.5471205579331,439.631298675795,48.6258116484846));
#43855=CARTESIAN_POINT('Ctrl Pts',(75.1566776929928,439.76886803912,47.9380800327125));
#43856=CARTESIAN_POINT('Ctrl Pts',(72.7259012321828,439.906437402445,48.4658280208805));
#43857=CARTESIAN_POINT('Ctrl Pts',(70.8358562575599,440.04400676577,50.0829000671532));
#43858=CARTESIAN_POINT('Ctrl Pts',(69.9383485646273,440.181576129095,52.4027431651896));
#43859=CARTESIAN_POINT('Ctrl Pts',(70.2479229119477,440.319145492421,54.870810378673));
#43860=CARTESIAN_POINT('Ctrl Pts',(71.6905770867303,440.456714855746,56.8971225407413));
#43861=CARTESIAN_POINT('Ctrl Pts',(73.9214518010143,440.594284219071,57.9972998257143));
#43862=CARTESIAN_POINT('Ctrl Pts',(76.4072675695861,440.731853582396,57.908350336352));
#43863=CARTESIAN_POINT('Ctrl Pts',(78.5538025209526,440.869422945721,56.6515370046695));
#43864=CARTESIAN_POINT('Ctrl Pts',(79.8479381712158,441.006992309046,54.5272947947597));
#43865=CARTESIAN_POINT('Ctrl Pts',(79.9803178422356,441.144561672372,52.0434132213975));
#43866=CARTESIAN_POINT('Ctrl Pts',(78.9192968332566,441.282131035697,49.7936517970953));
#43867=CARTESIAN_POINT('Ctrl Pts',(76.9185069292538,441.419700399022,48.3158047793713));
#43868=CARTESIAN_POINT('Ctrl Pts',(74.4562269864796,441.557269762347,47.9631441334462));
#43869=CARTESIAN_POINT('Ctrl Pts',(72.1210527552898,441.694839125672,48.8199716293573));
#43870=CARTESIAN_POINT('Ctrl Pts',(70.4711959990666,441.832408488998,50.6814669239287));
#43871=CARTESIAN_POINT('Ctrl Pts',(69.9010467538623,441.969977852323,53.1026488431487));
#43872=CARTESIAN_POINT('Ctrl Pts',(70.5468963555892,442.107547215648,55.5047459144002));
#43873=CARTESIAN_POINT('Ctrl Pts',(72.254357675336,442.245116578973,57.3135488028693));
#43874=CARTESIAN_POINT('Ctrl Pts',(74.6152705931949,442.382685942298,58.096672191648));
#43875=CARTESIAN_POINT('Ctrl Pts',(77.065270640993,442.520255305623,57.6669143370894));
#43876=CARTESIAN_POINT('Ctrl Pts',(79.018697516082,442.657824668949,56.1270067127672));
#43877=CARTESIAN_POINT('Ctrl Pts',(80.008594258239,442.795394032274,53.8450565626472));
#43878=CARTESIAN_POINT('Ctrl Pts',(79.7983309840795,442.932963395599,51.3665526987597));
#43879=CARTESIAN_POINT('Ctrl Pts',(78.4381700815129,443.070532758924,49.2839691189496));
#43880=CARTESIAN_POINT('Ctrl Pts',(76.2532512363784,443.208102122249,48.095137050093));
#43881=CARTESIAN_POINT('Ctrl Pts',(73.7658684107736,443.345671485574,48.0842408740924));
#43882=CARTESIAN_POINT('Ctrl Pts',(71.5706180740964,443.4832408489,49.2538852675232));
#43883=CARTESIAN_POINT('Ctrl Pts',(70.1922638800138,443.620810212225,51.3244725666779));
#43884=CARTESIAN_POINT('Ctrl Pts',(69.9602945300419,443.75837957555,53.8010391957915));
#43885=CARTESIAN_POINT('Ctrl Pts',(70.9301611413476,443.895948938875,56.0915742433382));
#43886=CARTESIAN_POINT('Ctrl Pts',(72.870021933513,444.0335183022,57.648536720338));
#43887=CARTESIAN_POINT('Ctrl Pts',(75.3161628508358,444.171087665526,58.0997425052797));
#43888=CARTESIAN_POINT('Ctrl Pts',(77.6838460965772,444.308657028851,57.3373331037104));
#43889=CARTESIAN_POINT('Ctrl Pts',(79.4070887894214,444.446226392176,55.5435586838559));
#43890=CARTESIAN_POINT('Ctrl Pts',(80.0739583508635,444.583795755501,53.1472120820915));
#43891=CARTESIAN_POINT('Ctrl Pts',(79.5250429353678,444.721365118826,50.7211280121556));
#43892=CARTESIAN_POINT('Ctrl Pts',(77.8915580376675,444.858934482152,48.8452497813659));
#43893=CARTESIAN_POINT('Ctrl Pts',(75.5639800826174,444.996503845477,47.9679967329641));
#43894=CARTESIAN_POINT('Ctrl Pts',(73.098704981645,445.134073208802,48.2990718366656));
#43895=CARTESIAN_POINT('Ctrl Pts',(71.0850444627416,445.271642572127,49.7593332387354));
#43896=CARTESIAN_POINT('Ctrl Pts',(70.0043540385292,445.409211935453,51.9997127277465));
#43897=CARTESIAN_POINT('Ctrl Pts',(70.1149673696467,445.546781298777,54.4846587510525));
#43898=CARTESIAN_POINT('Ctrl Pts',(71.3904428904962,445.684350662103,56.6201573447021));
#43899=CARTESIAN_POINT('Ctrl Pts',(73.5258845337356,445.821920025428,57.8957282114455));
#43900=CARTESIAN_POINT('Ctrl Pts',(76.010825615827,445.959489388753,58.0064524919801));
#43901=CARTESIAN_POINT('Ctrl Pts',(78.2512533539917,446.097058752078,56.9258620988023));
#43902=CARTESIAN_POINT('Ctrl Pts',(79.7116046618638,446.234628115403,54.9122667806309));
#43903=CARTESIAN_POINT('Ctrl Pts',(80.0427898364819,446.372197478728,52.4470064641778));
#43904=CARTESIAN_POINT('Ctrl Pts',(79.1656407122073,446.509766842054,50.1193893432686));
#43905=CARTESIAN_POINT('Ctrl Pts',(77.2898354162105,446.647336205379,48.4858206917342));
#43906=CARTESIAN_POINT('Ctrl Pts',(74.8637758570342,446.784905568704,47.9367969553663));
#43907=CARTESIAN_POINT('Ctrl Pts',(72.4673994828215,446.922474932029,48.6035595224625));
#43908=CARTESIAN_POINT('Ctrl Pts',(70.6735481242661,447.060044295355,50.3267221239526));
#43909=CARTESIAN_POINT('Ctrl Pts',(69.9110330095561,447.19761365868,52.6943713267705));
#43910=CARTESIAN_POINT('Ctrl Pts',(70.3621295771172,447.335183022005,55.1405323873919));
#43911=CARTESIAN_POINT('Ctrl Pts',(71.9190054403667,447.47275238533,57.0804626939226));
#43912=CARTESIAN_POINT('Ctrl Pts',(74.2094971823791,447.610321748655,58.050431573598));
#43913=CARTESIAN_POINT('Ctrl Pts',(76.6860741661464,447.747891111981,57.8185727992557));
#43914=CARTESIAN_POINT('Ctrl Pts',(78.7567230049145,447.885460475306,56.4403110555097));
#43915=CARTESIAN_POINT('Ctrl Pts',(79.9264654121804,448.023029838631,54.2451129440834));
#43916=CARTESIAN_POINT('Ctrl Pts',(79.9156802945179,448.160599201956,51.7577296344582));
#43917=CARTESIAN_POINT('Ctrl Pts',(78.7269457805599,448.298168565281,49.5727577117345));
#43918=CARTESIAN_POINT('Ctrl Pts',(76.6444229321967,448.435737928606,48.2125038259431));
#43919=CARTESIAN_POINT('Ctrl Pts',(74.1659284587545,448.573307291932,48.0021298900998));
#43920=CARTESIAN_POINT('Ctrl Pts',(71.8839341133392,448.710876655257,48.9919247452381));
#43921=CARTESIAN_POINT('Ctrl Pts',(70.3439392726461,448.848446018582,50.9452828635574));
#43922=CARTESIAN_POINT('Ctrl Pts',(69.9140720292799,448.986015381907,53.3952637207982));
#43923=CARTESIAN_POINT('Ctrl Pts',(70.6970900056636,449.123584745232,55.7562116017192));
#43924=CARTESIAN_POINT('Ctrl Pts',(72.5058166564581,449.261154108558,57.4637536804017));
#43925=CARTESIAN_POINT('Ctrl Pts',(74.9078848889915,449.398723471882,58.1097105319168));
#43926=CARTESIAN_POINT('Ctrl Pts',(77.329092262202,449.536292835208,57.5396693898256));
#43927=CARTESIAN_POINT('Ctrl Pts',(79.1906612188226,449.673862198533,55.8898957485305));
#43928=CARTESIAN_POINT('Ctrl Pts',(80.0475929762962,449.811431561858,53.5547597758731));
#43929=CARTESIAN_POINT('Ctrl Pts',(79.6950422682392,449.949000925183,51.0924640897269));
#43930=CARTESIAN_POINT('Ctrl Pts',(78.217284584591,450.086570288509,49.0916082038161));
#43931=CARTESIAN_POINT('Ctrl Pts',(75.9675705357031,450.224139651834,48.0304867470534));
#43932=CARTESIAN_POINT('Ctrl Pts',(73.4836830542445,450.361709015159,48.1627555159246));
#43933=CARTESIAN_POINT('Ctrl Pts',(71.3593830650128,450.499278378484,49.4567963203493));
#43934=CARTESIAN_POINT('Ctrl Pts',(70.1024738946765,450.63684774181,51.6032751544611));
#43935=CARTESIAN_POINT('Ctrl Pts',(70.0134134170065,450.774417105134,54.0890869492442));
#43936=CARTESIAN_POINT('Ctrl Pts',(71.1134910953859,450.91198646846,56.3200107823898));
#43937=CARTESIAN_POINT('Ctrl Pts',(73.1397388426772,451.049555831785,57.7627554286672));
#43938=CARTESIAN_POINT('Ctrl Pts',(75.6077922320367,451.18712519511,58.0724399698325));
#43939=CARTESIAN_POINT('Ctrl Pts',(77.9276753994789,451.324694558435,57.1750358595316));
#43940=CARTESIAN_POINT('Ctrl Pts',(79.544831834209,451.46226392176,55.2850630784119));
#43941=CARTESIAN_POINT('Ctrl Pts',(80.072688349079,451.599833285086,52.8543102017332));
#43942=CARTESIAN_POINT('Ctrl Pts',(79.3850634746068,451.737402648411,50.4638365918052));
#43943=CARTESIAN_POINT('Ctrl Pts',(77.6463305104883,451.874972011736,48.6850730529218));
#43944=CARTESIAN_POINT('Ctrl Pts',(75.2721249073685,452.012541375061,47.9432241451907));
#43945=CARTESIAN_POINT('Ctrl Pts',(72.8299886836307,452.150110738386,48.4156251531833));
#43946=CARTESIAN_POINT('Ctrl Pts',(70.9037023338835,452.287680101711,49.9893509701255));
#43947=CARTESIAN_POINT('Ctrl Pts',(69.9537350111984,452.425249465037,52.2882102813424));
#43948=CARTESIAN_POINT('Ctrl Pts',(70.2071716698,452.562818828362,54.7626722247312));
#43949=CARTESIAN_POINT('Ctrl Pts',(71.6034295402623,452.700388191687,56.8212290020234));
#43950=CARTESIAN_POINT('Ctrl Pts',(73.8087401344649,452.837957555012,57.971792876777));
#43951=CARTESIAN_POINT('Ctrl Pts',(76.2959349486093,452.975526918338,57.9393272815472));
#43952=CARTESIAN_POINT('Ctrl Pts',(78.4704624469033,453.113096281663,56.7315929696652));
#43953=CARTESIAN_POINT('Ctrl Pts',(79.8125126875738,453.250665644988,54.637292777964));
#43954=CARTESIAN_POINT('Ctrl Pts',(80.0012752017191,453.388235008313,52.1570588012735));
#43955=CARTESIAN_POINT('Ctrl Pts',(78.9916273498813,453.525804371638,49.8837784574698));
#43956=CARTESIAN_POINT('Ctrl Pts',(77.0249201934165,453.663373734963,48.3608684232863));
#43957=CARTESIAN_POINT('Ctrl Pts',(74.5712857496441,453.800943098289,47.9523720059004));
#43958=CARTESIAN_POINT('Ctrl Pts',(72.21725199923,453.938512461614,48.7559398701119));
#43959=CARTESIAN_POINT('Ctrl Pts',(70.5255412174673,454.076081824939,50.5794795103282));
#43960=CARTESIAN_POINT('Ctrl Pts',(69.9005429920568,454.213651188264,52.9870907188594));
#43961=CARTESIAN_POINT('Ctrl Pts',(70.4916705311956,454.351220551589,55.4032285662804));
#43962=CARTESIAN_POINT('Ctrl Pts',(72.1575906538854,454.488789914914,57.2503651195328));
#43963=CARTESIAN_POINT('Ctrl Pts',(74.5001218236798,454.62635927824,58.0868669942838));
#43964=CARTESIAN_POINT('Ctrl Pts',(76.9591566188663,454.763928641565,57.7129539659744));
#43965=CARTESIAN_POINT('Ctrl Pts',(78.9470927342512,454.90149800489,56.2175964403774));
#43966=CARTESIAN_POINT('Ctrl Pts',(79.6410139518298,454.993210913773,54.7119621310705));
#43967=CARTESIAN_POINT('Ctrl Pts',(79.7889778392583,455.039067368215,53.9215082683005));
#43968=CARTESIAN_POINT('Ctrl Pts',(75.8251119125118,438.,48.1763335988069));
#43969=CARTESIAN_POINT('Ctrl Pts',(75.0271751381672,438.045856454442,48.0385010433052));
#43970=CARTESIAN_POINT('Ctrl Pts',(73.3626330146115,438.137569363325,48.1648685832922));
#43971=CARTESIAN_POINT('Ctrl Pts',(71.2535490842209,438.275138726651,49.5160797993085));
#43972=CARTESIAN_POINT('Ctrl Pts',(70.0374660522581,438.412708089975,51.7055567731262));
#43973=CARTESIAN_POINT('Ctrl Pts',(70.0046175961469,438.550277453301,54.2099769100676));
#43974=CARTESIAN_POINT('Ctrl Pts',(71.1630752524974,438.687846816626,56.4306054140694));
#43975=CARTESIAN_POINT('Ctrl Pts',(73.2358186748897,438.825416179951,57.836628058181));
#43976=CARTESIAN_POINT('Ctrl Pts',(75.7274140404831,438.962985543276,58.0919298326021));
#43977=CARTESIAN_POINT('Ctrl Pts',(78.0422377232922,439.100554906601,57.1354858952104));
#43978=CARTESIAN_POINT('Ctrl Pts',(79.6269519827668,439.238124269927,55.1959270225485));
#43979=CARTESIAN_POINT('Ctrl Pts',(80.1027345777162,439.375693633252,52.7368959420052));
#43980=CARTESIAN_POINT('Ctrl Pts',(79.3558539781017,439.513262996577,50.346211308417));
#43981=CARTESIAN_POINT('Ctrl Pts',(77.564847398211,439.650832359902,48.5953545532883));
#43982=CARTESIAN_POINT('Ctrl Pts',(75.1578464351838,439.788401723227,47.90285916436));
#43983=CARTESIAN_POINT('Ctrl Pts',(72.7102324938985,439.925971086553,48.4342627525347));
#43984=CARTESIAN_POINT('Ctrl Pts',(70.8070955727843,440.063540449878,50.0625359188796));
#43985=CARTESIAN_POINT('Ctrl Pts',(69.9033710316553,440.201109813203,52.398448085174));
#43986=CARTESIAN_POINT('Ctrl Pts',(70.2150897357739,440.338679176528,54.8836110843821));
#43987=CARTESIAN_POINT('Ctrl Pts',(71.6677368744888,440.476248539853,56.9239590872673));
#43988=CARTESIAN_POINT('Ctrl Pts',(73.9140643916323,440.613817903178,58.0317570703397));
#43989=CARTESIAN_POINT('Ctrl Pts',(76.4170988864601,440.751387266504,57.9421914464564));
#43990=CARTESIAN_POINT('Ctrl Pts',(78.5785024367767,440.888956629829,56.6766724315182));
#43991=CARTESIAN_POINT('Ctrl Pts',(79.8816022941954,441.026525993154,54.5377160398189));
#43992=CARTESIAN_POINT('Ctrl Pts',(80.014898931527,441.164095356479,52.0366291379667));
#43993=CARTESIAN_POINT('Ctrl Pts',(78.9465284517881,441.301664719805,49.7712840865122));
#43994=CARTESIAN_POINT('Ctrl Pts',(76.9318794943156,441.43923408313,48.2832003313887));
#43995=CARTESIAN_POINT('Ctrl Pts',(74.4525438530313,441.576803446455,47.9280968788807));
#43996=CARTESIAN_POINT('Ctrl Pts',(72.1011943580286,441.71437280978,48.7908594397661));
#43997=CARTESIAN_POINT('Ctrl Pts',(70.4399093888999,441.851942173105,50.6652489231625));
#43998=CARTESIAN_POINT('Ctrl Pts',(69.8658108390438,441.989511536431,53.1032018634736));
#43999=CARTESIAN_POINT('Ctrl Pts',(70.5161341059696,442.127080899755,55.5219377590632));
#44000=CARTESIAN_POINT('Ctrl Pts',(72.2354226533932,442.264650263081,57.3432698470737));
#44001=CARTESIAN_POINT('Ctrl Pts',(74.6126891215678,442.402219626406,58.1318177678819));
#44002=CARTESIAN_POINT('Ctrl Pts',(77.0796598076102,442.539788989731,57.6990830704906));
#44003=CARTESIAN_POINT('Ctrl Pts',(79.0466176623673,442.677358353056,56.1485088279186));
#44004=CARTESIAN_POINT('Ctrl Pts',(80.0433712123539,442.814927716381,53.8507520860707));
#44005=CARTESIAN_POINT('Ctrl Pts',(79.8316514884425,442.952497079707,51.3550801439626));
#44006=CARTESIAN_POINT('Ctrl Pts',(78.4620690355979,443.090066443032,49.2580709429864));
#44007=CARTESIAN_POINT('Ctrl Pts',(76.2620157143041,443.227635806357,48.0610040828726));
#44008=CARTESIAN_POINT('Ctrl Pts',(73.7574033077667,443.365205169682,48.0500324313384));
#44009=CARTESIAN_POINT('Ctrl Pts',(71.5469469308476,443.502774533007,49.2277787070091));
#44010=CARTESIAN_POINT('Ctrl Pts',(70.1590451653594,443.640343896333,51.3127085316012));
#44011=CARTESIAN_POINT('Ctrl Pts',(69.9254690121854,443.777913259658,53.806429820115));
#44012=CARTESIAN_POINT('Ctrl Pts',(70.9020536867909,443.915482622983,56.1128309251798));
#44013=CARTESIAN_POINT('Ctrl Pts',(72.8553514892035,444.053051986308,57.6805781558292));
#44014=CARTESIAN_POINT('Ctrl Pts',(75.3184363133803,444.190621349633,58.1349093489344));
#44015=CARTESIAN_POINT('Ctrl Pts',(77.7025200060835,444.328190712959,57.3672188967954));
#44016=CARTESIAN_POINT('Ctrl Pts',(79.4376992408775,444.465760076284,55.5610193764604));
#44017=CARTESIAN_POINT('Ctrl Pts',(80.1091880683859,444.603329439609,53.1480737826581));
#44018=CARTESIAN_POINT('Ctrl Pts',(79.5564704305387,444.740898802934,50.7051847354578));
#44019=CARTESIAN_POINT('Ctrl Pts',(77.9116707243749,444.878468166259,48.8163126882502));
#44020=CARTESIAN_POINT('Ctrl Pts',(75.567970123329,445.016037529584,47.9329830913412));
#44021=CARTESIAN_POINT('Ctrl Pts',(73.0856185770117,445.15360689291,48.2663514830863));
#44022=CARTESIAN_POINT('Ctrl Pts',(71.0580098525792,445.291176256235,49.7367278106718));
#44023=CARTESIAN_POINT('Ctrl Pts',(69.9698337116788,445.42874561956,51.9926259401302));
#44024=CARTESIAN_POINT('Ctrl Pts',(70.0812132382212,445.566314982885,54.4947846651486));
#44025=CARTESIAN_POINT('Ctrl Pts',(71.3655237114099,445.70388434621,56.6450754112051));
#44026=CARTESIAN_POINT('Ctrl Pts',(73.5157571125727,445.841453709536,57.9294818907289));
#44027=CARTESIAN_POINT('Ctrl Pts',(76.0179108621497,445.979023072861,58.0409731352117));
#44028=CARTESIAN_POINT('Ctrl Pts',(78.2738575749735,446.116592436186,56.95289771824));
#44029=CARTESIAN_POINT('Ctrl Pts',(79.7443244311198,446.254161799511,54.9253546461714));
#44030=CARTESIAN_POINT('Ctrl Pts',(80.0778036562199,446.391731162836,52.4430179867826));
#44031=CARTESIAN_POINT('Ctrl Pts',(79.1945787032988,446.529300526162,50.0992779485839));
#44032=CARTESIAN_POINT('Ctrl Pts',(77.3057800960881,446.666869889487,48.4543939084407));
#44033=CARTESIAN_POINT('Ctrl Pts',(74.8629157294284,446.804439252812,47.9015671994052));
#44034=CARTESIAN_POINT('Ctrl Pts',(72.4499401569502,446.942008616137,48.5729482914402));
#44035=CARTESIAN_POINT('Ctrl Pts',(70.643663164976,447.079577979463,50.308046880104));
#44036=CARTESIAN_POINT('Ctrl Pts',(69.8758662674435,447.217147342787,52.6920962940756));
#44037=CARTESIAN_POINT('Ctrl Pts',(70.3300874866422,447.354716706113,55.1552014010794));
#44038=CARTESIAN_POINT('Ctrl Pts',(71.8977475035859,447.492286069438,57.1085691993689));
#44039=CARTESIAN_POINT('Ctrl Pts',(74.204105003148,447.629855432763,58.0852568507357));
#44040=CARTESIAN_POINT('Ctrl Pts',(76.6978367180401,447.767424796088,57.8517920391255));
#44041=CARTESIAN_POINT('Ctrl Pts',(78.7828285085176,447.904994159413,56.463983364358));
#44042=CARTESIAN_POINT('Ctrl Pts',(79.9606734769448,448.042563522738,54.2535795744433));
#44043=CARTESIAN_POINT('Ctrl Pts',(79.9498136530265,448.180132886064,51.7489666805328));
#44044=CARTESIAN_POINT('Ctrl Pts',(78.7528450235537,448.317702249389,49.5488599139924));
#44045=CARTESIAN_POINT('Ctrl Pts',(76.6558969746985,448.455271612714,48.1791838338476));
#44046=CARTESIAN_POINT('Ctrl Pts',(74.1602344880813,448.592840976039,47.9673526817221));
#44047=CARTESIAN_POINT('Ctrl Pts',(71.8624332448065,448.730410339365,48.9640036389398));
#44048=CARTESIAN_POINT('Ctrl Pts',(70.311771181734,448.867979702689,50.9308922606635));
#44049=CARTESIAN_POINT('Ctrl Pts',(69.8789263378217,449.005549066015,53.3978436232196));
#44050=CARTESIAN_POINT('Ctrl Pts',(70.6673681160653,449.14311842934,55.7751452966382));
#44051=CARTESIAN_POINT('Ctrl Pts',(72.4886234383188,449.280687792665,57.4945151623977));
#44052=CARTESIAN_POINT('Ctrl Pts',(74.9073302954306,449.41825715599,58.1449464220086));
#44053=CARTESIAN_POINT('Ctrl Pts',(77.3453088660466,449.555826519316,57.5709567240733));
#44054=CARTESIAN_POINT('Ctrl Pts',(79.2197725217338,449.693395882641,55.9097554455925));
#44055=CARTESIAN_POINT('Ctrl Pts',(80.0826400663797,449.830965245966,53.5584444741309));
#44056=CARTESIAN_POINT('Ctrl Pts',(79.7276473132564,449.968534609291,51.0790929804237));
#44057=CARTESIAN_POINT('Ctrl Pts',(78.2396535110072,450.106103972616,49.0643775840001));
#44058=CARTESIAN_POINT('Ctrl Pts',(75.9743561631267,450.243673335941,47.9959059606967));
#44059=CARTESIAN_POINT('Ctrl Pts',(73.4732633122539,450.381242699267,48.1290909276837));
#44060=CARTESIAN_POINT('Ctrl Pts',(71.3342487410075,450.518812062591,49.4320952822867));
#44061=CARTESIAN_POINT('Ctrl Pts',(70.0686332235611,450.656381425917,51.5934423266361));
#44062=CARTESIAN_POINT('Ctrl Pts',(69.9789558425772,450.793950789242,54.0964728201495));
#44063=CARTESIAN_POINT('Ctrl Pts',(71.0866535291021,450.931520152567,56.3428497963907));
#44064=CARTESIAN_POINT('Ctrl Pts',(73.1269366710226,451.069089515892,57.7955880332776));
#44065=CARTESIAN_POINT('Ctrl Pts',(75.6120857503499,451.206658879218,58.1074176945308));
#44066=CARTESIAN_POINT('Ctrl Pts',(77.9480382636025,451.344228242543,57.2037974535288));
#44067=CARTESIAN_POINT('Ctrl Pts',(79.5763964029459,451.481797605868,55.300733225987));
#44068=CARTESIAN_POINT('Ctrl Pts',(80.1079092695645,451.619366969193,52.8531430321954));
#44069=CARTESIAN_POINT('Ctrl Pts',(79.4155213613108,451.756936332518,50.4461111112164));
#44070=CARTESIAN_POINT('Ctrl Pts',(77.6647445573712,451.894505695844,48.6550264490875));
#44071=CARTESIAN_POINT('Ctrl Pts',(75.2740933282832,452.032075059169,47.9080389090301));
#44072=CARTESIAN_POINT('Ctrl Pts',(72.8150409373668,452.169644422494,48.3837121400662));
#44073=CARTESIAN_POINT('Ctrl Pts',(70.8754116046977,452.307213785819,49.96833882681));
#44074=CARTESIAN_POINT('Ctrl Pts',(69.9188640569258,452.444783149145,52.2831218559795));
#44075=CARTESIAN_POINT('Ctrl Pts',(70.1740562182895,452.582352512469,54.7747238800505));
#44076=CARTESIAN_POINT('Ctrl Pts',(71.5799856751815,452.719921875795,56.8475398498696));
#44077=CARTESIAN_POINT('Ctrl Pts',(73.8005719949271,452.85749123912,58.0060734400985));
#44078=CARTESIAN_POINT('Ctrl Pts',(76.304995087688,452.995060602445,57.9733829624763));
#44079=CARTESIAN_POINT('Ctrl Pts',(78.4945850834537,453.13262996577,56.7572829274506));
#44080=CARTESIAN_POINT('Ctrl Pts',(79.8459314256328,453.270199329095,54.6484759560617));
#44081=CARTESIAN_POINT('Ctrl Pts',(80.0360014582592,453.407768692421,52.1510619170208));
#44082=CARTESIAN_POINT('Ctrl Pts',(79.0193599867834,453.545338055746,49.8620350354254));
#44083=CARTESIAN_POINT('Ctrl Pts',(77.0390298609172,453.682907419071,48.3285761217461));
#44084=CARTESIAN_POINT('Ctrl Pts',(74.5683996041992,453.820476782396,47.9172501350589));
#44085=CARTESIAN_POINT('Ctrl Pts',(72.1980599540245,453.958046145721,48.726384145908));
#44086=CARTESIAN_POINT('Ctrl Pts',(70.4946310452694,454.095615509047,50.562555064065));
#44087=CARTESIAN_POINT('Ctrl Pts',(69.8653035877856,454.233184872372,52.9868432922107));
#44088=CARTESIAN_POINT('Ctrl Pts',(70.4605257438334,454.370754235697,55.4197172214916));
#44089=CARTESIAN_POINT('Ctrl Pts',(72.1379853470107,454.508323599022,57.2796485035691));
#44090=CARTESIAN_POINT('Ctrl Pts',(74.4967427405941,454.645892962347,58.121944651965));
#44091=CARTESIAN_POINT('Ctrl Pts',(76.9728107558315,454.783462325672,57.745441606262));
#44092=CARTESIAN_POINT('Ctrl Pts',(78.9745168891792,454.921031688998,56.2397260516373));
#44093=CARTESIAN_POINT('Ctrl Pts',(79.673244753992,455.012744597881,54.7236625281701));
#44094=CARTESIAN_POINT('Ctrl Pts',(79.822233556342,455.058601052323,53.9277333567095));
#44095=CARTESIAN_POINT('',(75.8251119125118,438.,48.1763335988071));
#44096=CARTESIAN_POINT('Ctrl Pts',(75.8251119125118,438.,48.1763335988069));
#44097=CARTESIAN_POINT('Ctrl Pts',(75.0271751381672,438.045856454442,48.0385010433052));
#44098=CARTESIAN_POINT('Ctrl Pts',(73.3626330146115,438.137569363325,48.1648685832922));
#44099=CARTESIAN_POINT('Ctrl Pts',(71.2535490842209,438.275138726651,49.5160797993085));
#44100=CARTESIAN_POINT('Ctrl Pts',(70.2293979957942,438.390995793545,51.3599960179249));
#44101=CARTESIAN_POINT('Ctrl Pts',(70.0701468767135,438.460996405998,52.5964026908782));
#44102=CARTESIAN_POINT('Ctrl Pts',(70.0700845742477,438.485140564009,53.0228422002615));
#44103=CARTESIAN_POINT('Ctrl Pts',(79.722466405091,455.,53.9090580914827));
#44104=CARTESIAN_POINT('Ctrl Pts',(79.5765523475055,454.954143545558,54.6885613368713));
#44105=CARTESIAN_POINT('Ctrl Pts',(79.2343983859504,454.908287091117,55.4309492773644));
#44106=CARTESIAN_POINT('Ctrl Pts',(78.736588725263,454.862430636675,56.0479168255346));
#44107=CARTESIAN_POINT('Ctrl Pts',(78.2387790645755,454.816574182233,56.6648843737049));
#44108=CARTESIAN_POINT('Ctrl Pts',(77.5853137047556,454.770717727791,57.1564315295522));
#44109=CARTESIAN_POINT('Ctrl Pts',(76.8544196323316,454.72486127335,57.4636606063962));
#44110=CARTESIAN_POINT('Ctrl Pts',(76.1235255599076,454.679004818908,57.7708896832402));
#44111=CARTESIAN_POINT('Ctrl Pts',(75.3152027748794,454.633148364466,57.8938006810809));
#44112=CARTESIAN_POINT('Ctrl Pts',(74.5260282619959,454.587291910025,57.8177706254244));
#44113=CARTESIAN_POINT('Ctrl Pts',(73.7368537491124,454.541435455583,57.7417405697679));
#44114=CARTESIAN_POINT('Ctrl Pts',(72.9668275083734,454.495579001141,57.4667694606141));
#44115=CARTESIAN_POINT('Ctrl Pts',(72.3080075277182,454.449722546699,57.0256927234369));
#44116=CARTESIAN_POINT('Ctrl Pts',(71.6491875470629,454.403866092258,56.5846159862597));
#44117=CARTESIAN_POINT('Ctrl Pts',(71.1015738264913,454.358009637816,55.9774336210589));
#44118=CARTESIAN_POINT('Ctrl Pts',(70.7306105819854,454.312153183374,55.2767314911749));
#44119=CARTESIAN_POINT('Ctrl Pts',(70.3649209659794,454.266948626145,54.5859905711328));
#44120=CARTESIAN_POINT('Ctrl Pts',(70.170894985723,454.221744068916,53.8043699479757));
#44121=CARTESIAN_POINT('Ctrl Pts',(70.170785177935,454.176539511687,53.0227998720929));
#44122=CARTESIAN_POINT('Ctrl Pts',(74.7983630544219,438.,48.2104548970641));
#44123=CARTESIAN_POINT('Ctrl Pts',(74.9465799254592,438.,48.1896568984132));
#44124=CARTESIAN_POINT('Ctrl Pts',(75.0957540366303,438.,48.1757286123456));
#44125=CARTESIAN_POINT('Ctrl Pts',(75.2453698829481,438.,48.1687204856835));
#44126=CARTESIAN_POINT('Ctrl Pts',(75.3943109611245,438.,48.1617439657043));
#44127=CARTESIAN_POINT('Ctrl Pts',(75.5436906225955,438.,48.161625107134));
#44128=CARTESIAN_POINT('Ctrl Pts',(75.6930137380414,438.,48.1684631220341));
#44129=CARTESIAN_POINT('Ctrl Pts',(75.7370555516977,438.,48.1704799469384));
#44130=CARTESIAN_POINT('Ctrl Pts',(75.7810924905272,438.,48.1731023005458));
#44131=CARTESIAN_POINT('Ctrl Pts',(75.8251119125118,438.,48.1763335988071));
#44132=CARTESIAN_POINT('Origin',(74.9879498948689,438.,53.0228109606356));
#44133=CARTESIAN_POINT('',(70.6773963296588,438.,50.6560254819444));
#44134=CARTESIAN_POINT('Ctrl Pts',(70.6773963296589,438.,50.6560254819442));
#44135=CARTESIAN_POINT('Ctrl Pts',(70.7621366228395,438.,50.5320627139349));
#44136=CARTESIAN_POINT('Ctrl Pts',(70.8523397873687,438.,50.4122232081957));
#44137=CARTESIAN_POINT('Ctrl Pts',(70.9477495550052,438.,50.2969251560475));
#44138=CARTESIAN_POINT('Ctrl Pts',(71.0421808602021,438.,50.1828095280492));
#44139=CARTESIAN_POINT('Ctrl Pts',(71.141713099239,438.,50.0731421574764));
#44140=CARTESIAN_POINT('Ctrl Pts',(71.2461307971266,438.,49.9683670778037));
#44141=CARTESIAN_POINT('Ctrl Pts',(71.278010555787,438.,49.9363782069402));
#44142=CARTESIAN_POINT('Ctrl Pts',(71.3103459100883,438.,49.9048456707748));
#44143=CARTESIAN_POINT('Ctrl Pts',(71.3431312258736,438.,49.8737829466856));
#44144=CARTESIAN_POINT('Origin',(74.9879498948689,438.,53.0228109606356));
#44145=CARTESIAN_POINT('Origin',(74.9879498948689,433.764859435991,53.0228109606356));
#44146=CARTESIAN_POINT('Ctrl Pts',(70.6773963296586,438.,50.6560254819443));
#44147=CARTESIAN_POINT('Ctrl Pts',(70.4537513653296,438.026322786249,51.0635801320965));
#44148=CARTESIAN_POINT('Ctrl Pts',(70.1589582985954,438.072942598246,51.8409980362099));
#44149=CARTESIAN_POINT('Ctrl Pts',(70.0700718391714,438.119562410242,52.6643217470763));
#44150=CARTESIAN_POINT('Ctrl Pts',(70.0701612938333,438.139859435991,53.0228096632581));
#44151=CARTESIAN_POINT('Ctrl Pts',(71.2663265142102,437.941398947677,49.8074256843371));
#44152=CARTESIAN_POINT('Ctrl Pts',(70.7369368452775,437.987255418033,50.4201637546089));
#44153=CARTESIAN_POINT('Ctrl Pts',(69.9872801539104,438.078968358746,51.9117019039279));
#44154=CARTESIAN_POINT('Ctrl Pts',(70.0581083962177,438.216537769815,54.4154980042378));
#44155=CARTESIAN_POINT('Ctrl Pts',(71.3075510106673,438.354107180884,56.586112001967));
#44156=CARTESIAN_POINT('Ctrl Pts',(73.4367474201414,438.491676591953,57.9050989515375));
#44157=CARTESIAN_POINT('Ctrl Pts',(75.9367802424272,438.629246003022,58.0569396214243));
#44158=CARTESIAN_POINT('Ctrl Pts',(78.2099924611958,438.766815414091,57.0054284326608));
#44159=CARTESIAN_POINT('Ctrl Pts',(79.7129963873825,438.90438482516,55.0018790181383));
#44160=CARTESIAN_POINT('Ctrl Pts',(80.0864990188232,439.041954236229,52.5252494404828));
#44161=CARTESIAN_POINT('Ctrl Pts',(79.2412191183861,439.179523647298,50.1675568417403));
#44162=CARTESIAN_POINT('Ctrl Pts',(77.3792153333098,439.317093058367,48.492400302215));
#44163=CARTESIAN_POINT('Ctrl Pts',(74.9455912824701,439.454662469436,47.9002160217303));
#44164=CARTESIAN_POINT('Ctrl Pts',(72.5220927714855,439.592231880505,48.5325636389322));
#44165=CARTESIAN_POINT('Ctrl Pts',(70.6880455611049,439.729801291574,50.2382831133303));
#44166=CARTESIAN_POINT('Ctrl Pts',(69.8818697359254,439.867370702643,52.6096306023301));
#44167=CARTESIAN_POINT('Ctrl Pts',(70.2962777667704,440.004940113712,55.0797468393278));
#44168=CARTESIAN_POINT('Ctrl Pts',(71.8322073992925,440.142509524781,57.0581624818043));
#44169=CARTESIAN_POINT('Ctrl Pts',(74.1225020644475,440.28007893585,58.0719467909454));
#44170=CARTESIAN_POINT('Ctrl Pts',(76.6196778606811,440.417648346919,57.8787595222969));
#44171=CARTESIAN_POINT('Ctrl Pts',(78.7267969530214,440.555217757988,56.5247811576843));
#44172=CARTESIAN_POINT('Ctrl Pts',(79.9401626795821,440.692787169057,54.3336736996951));
#44173=CARTESIAN_POINT('Ctrl Pts',(79.969725812863,440.830356580126,51.8292108229069));
#44174=CARTESIAN_POINT('Ctrl Pts',(78.8084194282583,440.967925991195,49.6100723052293));
#44175=CARTESIAN_POINT('Ctrl Pts',(76.7338482188175,441.105495402264,48.2067325114984));
#44176=CARTESIAN_POINT('Ctrl Pts',(74.2419284313758,441.243064813333,47.9546530544782));
#44177=CARTESIAN_POINT('Ctrl Pts',(71.928341478485,441.380634224401,48.9140923131546));
#44178=CARTESIAN_POINT('Ctrl Pts',(70.346139168261,441.518203635471,50.8557009578655));
#44179=CARTESIAN_POINT('Ctrl Pts',(69.8735393357385,441.655773046539,53.3153468018811));
#44180=CARTESIAN_POINT('Ctrl Pts',(70.6235146926476,441.793342457608,55.7050633632576));
#44181=CARTESIAN_POINT('Ctrl Pts',(72.4167872452805,441.930911868677,57.4536004179581));
#44182=CARTESIAN_POINT('Ctrl Pts',(74.8246838346499,442.068481279746,58.1429786121231));
#44183=CARTESIAN_POINT('Ctrl Pts',(77.2716083886679,442.206050690815,57.608405411681));
#44184=CARTESIAN_POINT('Ctrl Pts',(79.1726353884369,442.343620101884,55.9776679632129));
#44185=CARTESIAN_POINT('Ctrl Pts',(80.0733334938275,442.481189512953,53.6405861925782));
#44186=CARTESIAN_POINT('Ctrl Pts',(79.7583951646866,442.618758924023,51.1558282308192));
#44187=CARTESIAN_POINT('Ctrl Pts',(78.3031048903914,442.756328335091,49.1173634905726));
#44188=CARTESIAN_POINT('Ctrl Pts',(76.0553427955826,442.89389774616,48.0124771412913));
#44189=CARTESIAN_POINT('Ctrl Pts',(73.5524255733744,443.031467157229,48.1052869385125));
#44190=CARTESIAN_POINT('Ctrl Pts',(71.3926635200745,443.169036568298,49.3736071476132));
#44191=CARTESIAN_POINT('Ctrl Pts',(70.0923373430908,443.306605979367,51.5142519367218));
#44192=CARTESIAN_POINT('Ctrl Pts',(69.9622837466277,443.444175390436,54.0155104882782));
#44193=CARTESIAN_POINT('Ctrl Pts',(71.0335914159785,443.581744801505,56.279469003198));
#44194=CARTESIAN_POINT('Ctrl Pts',(73.0501694171724,443.719314212574,57.7649391122166));
#44195=CARTESIAN_POINT('Ctrl Pts',(75.5299645002191,443.856883623643,58.1168263466887));
#44196=CARTESIAN_POINT('Ctrl Pts',(77.8801936047136,443.994453034712,57.2510137595351));
#44197=CARTESIAN_POINT('Ctrl Pts',(79.5390457928333,444.132022445781,55.3744696759449));
#44198=CARTESIAN_POINT('Ctrl Pts',(80.1099804457359,444.26959185685,52.9357729129582));
#44199=CARTESIAN_POINT('Ctrl Pts',(79.4565183869152,444.407161267919,50.5178821756897));
#44200=CARTESIAN_POINT('Ctrl Pts',(77.7348665714272,444.544730678988,48.6987825891046));
#44201=CARTESIAN_POINT('Ctrl Pts',(75.3565775663022,444.682300090057,47.9133211401532));
#44202=CARTESIAN_POINT('Ctrl Pts',(72.8901698933421,444.819869501126,48.3492586017812));
#44203=CARTESIAN_POINT('Ctrl Pts',(70.9252264171065,444.957438912195,49.9023862252835));
#44204=CARTESIAN_POINT('Ctrl Pts',(69.9314574033058,445.095008323264,52.2014363393299));
#44205=CARTESIAN_POINT('Ctrl Pts',(70.1464185440873,445.232577734333,54.6968320970487));
#44206=CARTESIAN_POINT('Ctrl Pts',(71.5187244149973,445.370147145402,56.7920611719599));
#44207=CARTESIAN_POINT('Ctrl Pts',(73.7203319129862,445.507716556471,57.9862691540494));
#44208=CARTESIAN_POINT('Ctrl Pts',(76.2249573788151,445.64528596754,57.9939863820444));
#44209=CARTESIAN_POINT('Ctrl Pts',(78.4338821687736,445.782855378609,56.813368089795));
#44210=CARTESIAN_POINT('Ctrl Pts',(79.8190734602514,445.920424789678,54.7266353887282));
#44211=CARTESIAN_POINT('Ctrl Pts',(80.0494079525281,446.057994200747,52.2326116716488));
#44212=CARTESIAN_POINT('Ctrl Pts',(79.0698252955847,446.195563611816,49.927481285336));
#44213=CARTESIAN_POINT('Ctrl Pts',(77.1144900013488,446.333133022885,48.3622745364359));
#44214=CARTESIAN_POINT('Ctrl Pts',(74.6508155459415,446.470702433954,47.9111465529761));
#44215=CARTESIAN_POINT('Ctrl Pts',(72.2677314314422,446.608271845023,48.6819373046774));
#44216=CARTESIAN_POINT('Ctrl Pts',(70.5349024274333,446.745841256092,50.4903929780497));
#44217=CARTESIAN_POINT('Ctrl Pts',(69.8665529539796,446.883410667161,52.9042109622857));
#44218=CARTESIAN_POINT('Ctrl Pts',(70.4224487308386,447.02098007823,55.3463797043995));
#44219=CARTESIAN_POINT('Ctrl Pts',(72.069705552325,447.158549489299,57.2331105394031));
#44220=CARTESIAN_POINT('Ctrl Pts',(74.4145546160935,447.296118900368,58.1133895564375));
#44221=CARTESIAN_POINT('Ctrl Pts',(76.8964710571215,447.433688311437,57.7767902999883));
#44222=CARTESIAN_POINT('Ctrl Pts',(78.9221647146049,447.571257722506,56.3037751996861));
#44223=CARTESIAN_POINT('Ctrl Pts',(80.0074032848607,447.708827133575,54.0464614143837));
#44224=CARTESIAN_POINT('Ctrl Pts',(79.8927657192128,447.846396544644,51.5444489227623));
#44225=CARTESIAN_POINT('Ctrl Pts',(78.605655575103,447.983965955713,49.3958317496446));
#44226=CARTESIAN_POINT('Ctrl Pts',(76.4537503277871,448.121535366782,48.1142264725559));
#44227=CARTESIAN_POINT('Ctrl Pts',(73.9514525530772,448.259104777851,48.0059946548279));
#44228=CARTESIAN_POINT('Ctrl Pts',(71.6969244713428,448.39667418892,49.0970085907417));
#44229=CARTESIAN_POINT('Ctrl Pts',(70.2291001522561,448.534243599989,51.1264666583019));
#44230=CARTESIAN_POINT('Ctrl Pts',(69.8988559234434,448.671813011058,53.6092366897432));
#44231=CARTESIAN_POINT('Ctrl Pts',(70.7851350758139,448.809382422127,55.9518244775881));
#44232=CARTESIAN_POINT('Ctrl Pts',(72.6760768504256,448.946951833196,57.594245703923));
#44233=CARTESIAN_POINT('Ctrl Pts',(75.1196607316056,449.084521244265,58.1438874921126));
#44234=CARTESIAN_POINT('Ctrl Pts',(77.5317597721941,449.222090655334,57.469360622315));
#44235=CARTESIAN_POINT('Ctrl Pts',(79.3357733243977,449.359660066403,55.7319074911046));
#44236=CARTESIAN_POINT('Ctrl Pts',(80.1004606450606,449.497229477472,53.3468578938625));
#44237=CARTESIAN_POINT('Ctrl Pts',(79.6430269164599,449.634798888541,50.8843464393459));
#44238=CARTESIAN_POINT('Ctrl Pts',(78.0728194662947,449.77236829961,48.9330246198776));
#44239=CARTESIAN_POINT('Ctrl Pts',(75.7651888161234,449.909937710679,47.9593465097831));
#44240=CARTESIAN_POINT('Ctrl Pts',(73.2717629486147,450.047507121747,48.1960651675296));
#44241=CARTESIAN_POINT('Ctrl Pts',(71.1885832974899,450.185076532817,49.586594139118));
#44242=CARTESIAN_POINT('Ctrl Pts',(70.013623916093,450.322645943885,51.7985341771286));
#44243=CARTESIAN_POINT('Ctrl Pts',(70.0277531804915,450.460215354954,54.3031316784399));
#44244=CARTESIAN_POINT('Ctrl Pts',(71.2275935581432,450.597784766023,56.5016746841243));
#44245=CARTESIAN_POINT('Ctrl Pts',(73.326328990768,450.735354177093,57.8686120870556));
#44246=CARTESIAN_POINT('Ctrl Pts',(75.8222668904432,450.872923588161,58.0771840905751));
#44247=CARTESIAN_POINT('Ctrl Pts',(78.1187653342674,451.01049299923,57.0775325626919));
#44248=CARTESIAN_POINT('Ctrl Pts',(79.6668574398354,451.148062410299,55.1086193821872));
#44249=CARTESIAN_POINT('Ctrl Pts',(80.096479252104,451.285631821368,52.6411037534401));
#44250=CARTESIAN_POINT('Ctrl Pts',(79.304931747903,451.423201232437,50.2648333925011));
#44251=CARTESIAN_POINT('Ctrl Pts',(77.4814305423453,451.560770643506,48.547844274008));
#44252=CARTESIAN_POINT('Ctrl Pts',(75.0618748081809,451.698340054575,47.9005743697575));
#44253=CARTESIAN_POINT('Ctrl Pts',(72.6246476798502,451.835909465644,48.4777504300927));
#44254=CARTESIAN_POINT('Ctrl Pts',(70.7523565534021,451.973478876713,50.1414013001772));
#44255=CARTESIAN_POINT('Ctrl Pts',(69.8925635969428,452.111048287782,52.493839259314));
#44256=CARTESIAN_POINT('Ctrl Pts',(70.2507981720304,452.248617698851,54.9727253537667));
#44257=CARTESIAN_POINT('Ctrl Pts',(71.7414260302598,452.38618710992,56.9854938121638));
#44258=CARTESIAN_POINT('Ctrl Pts',(74.0081197682281,452.523756520989,58.0510020380353));
#44259=CARTESIAN_POINT('Ctrl Pts',(76.509037174062,452.661325932058,57.9145454249311));
#44260=CARTESIAN_POINT('Ctrl Pts',(78.646345999496,452.798895343127,56.6087432716859));
#44261=CARTESIAN_POINT('Ctrl Pts',(79.9091328695011,452.936464754196,54.4457412810724));
#44262=CARTESIAN_POINT('Ctrl Pts',(79.9955346778371,453.074034165265,51.9425946677425));
#44263=CARTESIAN_POINT('Ctrl Pts',(78.884897471774,453.211603576334,49.6976685283788));
#44264=CARTESIAN_POINT('Ctrl Pts',(76.842713757919,453.349172987403,48.2476017112594));
#44265=CARTESIAN_POINT('Ctrl Pts',(74.357157626194,453.486742398472,47.9390255330312));
#44266=CARTESIAN_POINT('Ctrl Pts',(72.0223894626918,453.624311809541,48.8457040127446));
#44267=CARTESIAN_POINT('Ctrl Pts',(70.3965239417743,453.76188122061,50.7508992351417));
#44268=CARTESIAN_POINT('Ctrl Pts',(69.8682172124607,453.899450631679,53.1991852682697));
#44269=CARTESIAN_POINT('Ctrl Pts',(70.5637564965961,454.037020042748,55.6053073318474));
#44270=CARTESIAN_POINT('Ctrl Pts',(72.3168804345463,454.174589453817,57.394102321988));
#44271=CARTESIAN_POINT('Ctrl Pts',(74.708503577028,454.312158864886,58.1379492928087));
#44272=CARTESIAN_POINT('Ctrl Pts',(77.1669384806062,454.449728275955,57.6590781969942));
#44273=CARTESIAN_POINT('Ctrl Pts',(79.104460246599,454.587297687024,56.0718752075947));
#44274=CARTESIAN_POINT('Ctrl Pts',(80.0579990258397,454.724867098093,53.7559659325096));
#44275=CARTESIAN_POINT('Ctrl Pts',(79.7993737921405,454.862436509162,51.264555781545));
#44276=CARTESIAN_POINT('Ctrl Pts',(78.8603172683709,454.954149449875,49.8843949028968));
#44277=CARTESIAN_POINT('Ctrl Pts',(78.2550383520211,455.000005920231,49.3464926833852));
#44278=CARTESIAN_POINT('Ctrl Pts',(71.2919280847647,437.960932631785,49.8295447717866));
#44279=CARTESIAN_POINT('Ctrl Pts',(70.7661801618051,438.006789102141,50.4380677307123));
#44280=CARTESIAN_POINT('Ctrl Pts',(70.0216804642315,438.098502042854,51.9193453793684));
#44281=CARTESIAN_POINT('Ctrl Pts',(70.0920214691003,438.236071453923,54.4059175142311));
#44282=CARTESIAN_POINT('Ctrl Pts',(71.3328689921139,438.373640864992,56.5615995530474));
#44283=CARTESIAN_POINT('Ctrl Pts',(73.4474183600886,438.51121027606,57.8715130059215));
#44284=CARTESIAN_POINT('Ctrl Pts',(75.9302531050459,438.64877968713,58.0223091424889));
#44285=CARTESIAN_POINT('Ctrl Pts',(78.187827577312,438.786349098198,56.9780314470519));
#44286=CARTESIAN_POINT('Ctrl Pts',(79.6804921281445,438.923918509268,54.9882647306826));
#44287=CARTESIAN_POINT('Ctrl Pts',(80.0514253824632,439.061487920337,52.5286722361449));
#44288=CARTESIAN_POINT('Ctrl Pts',(79.2119602813209,439.199057331405,50.1871985363179));
#44289=CARTESIAN_POINT('Ctrl Pts',(77.3627654821092,439.336626742474,48.5235656341814));
#44290=CARTESIAN_POINT('Ctrl Pts',(74.945882673321,439.474196153543,47.9354550726326));
#44291=CARTESIAN_POINT('Ctrl Pts',(72.5390557493757,439.611765564612,48.5634526816578));
#44292=CARTESIAN_POINT('Ctrl Pts',(70.7176252076512,439.749334975681,50.2574382719404));
#44293=CARTESIAN_POINT('Ctrl Pts',(69.9169951793341,439.88690438675,52.6124729281146));
#44294=CARTESIAN_POINT('Ctrl Pts',(70.3285524390626,440.024473797819,55.0655968881807));
#44295=CARTESIAN_POINT('Ctrl Pts',(71.8539161956667,440.162043208888,57.0304027312562));
#44296=CARTESIAN_POINT('Ctrl Pts',(74.1284556017685,440.299612619957,58.0372130755806));
#44297=CARTESIAN_POINT('Ctrl Pts',(76.6084529745575,440.437182031026,57.8453547693184));
#44298=CARTESIAN_POINT('Ctrl Pts',(78.7010768983675,440.574751442095,56.5006906122666));
#44299=CARTESIAN_POINT('Ctrl Pts',(79.9060957114769,440.712320853164,54.3246560905852));
#44300=CARTESIAN_POINT('Ctrl Pts',(79.9354554758069,440.849890264234,51.8374217660934));
#44301=CARTESIAN_POINT('Ctrl Pts',(78.7821378811198,440.987459675302,49.6335490143246));
#44302=CARTESIAN_POINT('Ctrl Pts',(76.7218379387462,441.125029086371,48.2398629923665));
#44303=CARTESIAN_POINT('Ctrl Pts',(74.2470604179255,441.26259849744,47.9895176253775));
#44304=CARTESIAN_POINT('Ctrl Pts',(71.9493889550104,441.400167908509,48.9423567664812));
#44305=CARTESIAN_POINT('Ctrl Pts',(70.3780708369611,441.537737319578,50.8706088123044));
#44306=CARTESIAN_POINT('Ctrl Pts',(69.9087220851415,441.675306730647,53.313334406694));
#44307=CARTESIAN_POINT('Ctrl Pts',(70.6535382561121,441.812876141716,55.686611771813));
#44308=CARTESIAN_POINT('Ctrl Pts',(72.434474634693,441.950445552785,57.4231203942423));
#44309=CARTESIAN_POINT('Ctrl Pts',(74.8258069648359,442.088014963854,58.1077562588723));
#44310=CARTESIAN_POINT('Ctrl Pts',(77.2558987807707,442.225584374923,57.5768604626454));
#44311=CARTESIAN_POINT('Ctrl Pts',(79.1438483484939,442.363153785992,55.9573410863927));
#44312=CARTESIAN_POINT('Ctrl Pts',(80.0383504249652,442.500723197061,53.6363364298888));
#44313=CARTESIAN_POINT('Ctrl Pts',(79.7255786008758,442.63829260813,51.1686714675448));
#44314=CARTESIAN_POINT('Ctrl Pts',(78.2802994730141,442.775862019199,49.1442296128866));
#44315=CARTESIAN_POINT('Ctrl Pts',(76.0480000497264,442.913431430268,48.0469439321665));
#44316=CARTESIAN_POINT('Ctrl Pts',(73.5623007470393,443.051000841337,48.1391152777421));
#44317=CARTESIAN_POINT('Ctrl Pts',(71.4173960006007,443.188570252406,49.3987105337786));
#44318=CARTESIAN_POINT('Ctrl Pts',(70.1260149502347,443.326139663475,51.5246295263745));
#44319=CARTESIAN_POINT('Ctrl Pts',(69.9968560107494,443.463709074544,54.0086815686384));
#44320=CARTESIAN_POINT('Ctrl Pts',(71.0607940039999,443.601278485613,56.2570659945857));
#44321=CARTESIAN_POINT('Ctrl Pts',(73.0634996815609,443.738847896682,57.7323173458439));
#44322=CARTESIAN_POINT('Ctrl Pts',(75.5262359055331,443.876417307751,58.0817838985492));
#44323=CARTESIAN_POINT('Ctrl Pts',(77.8602974535386,444.01398671882,57.2219273579296));
#44324=CARTESIAN_POINT('Ctrl Pts',(79.5077381641954,444.151556129889,55.358292284962));
#44325=CARTESIAN_POINT('Ctrl Pts',(80.0747452773383,444.289125540958,52.936371659927));
#44326=CARTESIAN_POINT('Ctrl Pts',(79.4257784759072,444.426694952027,50.5351139330338));
#44327=CARTESIAN_POINT('Ctrl Pts',(77.7159701453494,444.564264363096,48.7285281882989));
#44328=CARTESIAN_POINT('Ctrl Pts',(75.3540417247156,444.701833774165,47.9484700391031));
#44329=CARTESIAN_POINT('Ctrl Pts',(72.9046008169535,444.839403185234,48.3814086256329));
#44330=CARTESIAN_POINT('Ctrl Pts',(70.9531744631929,444.976972596303,49.9238520658189));
#44331=CARTESIAN_POINT('Ctrl Pts',(69.9662417261778,445.114542007372,52.2070866908481));
#44332=CARTESIAN_POINT('Ctrl Pts',(70.1797241190449,445.252111418441,54.6853162702576));
#44333=CARTESIAN_POINT('Ctrl Pts',(71.5425897049011,445.38968082951,56.7661319697402));
#44334=CARTESIAN_POINT('Ctrl Pts',(73.7290520353306,445.527250240579,57.9521248271964));
#44335=CARTESIAN_POINT('Ctrl Pts',(76.2164478303903,445.664819651648,57.959788967295));
#44336=CARTESIAN_POINT('Ctrl Pts',(78.410177116109,445.802389062717,56.7872923142914));
#44337=CARTESIAN_POINT('Ctrl Pts',(79.785839481913,445.939958473786,54.7149145409028));
#44338=CARTESIAN_POINT('Ctrl Pts',(80.0145894708287,446.077527884854,52.2380475636723));
#44339=CARTESIAN_POINT('Ctrl Pts',(79.0417455007272,446.215097295924,49.9487744934246));
#44340=CARTESIAN_POINT('Ctrl Pts',(77.0998612329313,446.352666706993,48.3943350218429));
#44341=CARTESIAN_POINT('Ctrl Pts',(74.6531347405342,446.490236118061,47.946310411217));
#44342=CARTESIAN_POINT('Ctrl Pts',(72.2864441967577,446.627805529131,48.711798784952));
#44343=CARTESIAN_POINT('Ctrl Pts',(70.5655355671304,446.7653749402,50.5078138374498));
#44344=CARTESIAN_POINT('Ctrl Pts',(69.9017837636851,446.902944351269,52.9050268283514));
#44345=CARTESIAN_POINT('Ctrl Pts',(70.4538554553274,447.040513762338,55.3303955482807));
#44346=CARTESIAN_POINT('Ctrl Pts',(72.0897805655085,447.178083173406,57.2041472965662));
#44347=CARTESIAN_POINT('Ctrl Pts',(74.4184990828446,447.315652584475,58.0783707504614));
#44348=CARTESIAN_POINT('Ctrl Pts',(76.8833420716781,447.453221995544,57.7440870076285));
#44349=CARTESIAN_POINT('Ctrl Pts',(78.8951006976473,447.590791406614,56.2812049853304));
#44350=CARTESIAN_POINT('Ctrl Pts',(79.9728737591767,447.728360817682,54.039419578971));
#44351=CARTESIAN_POINT('Ctrl Pts',(79.8590248014627,447.865930228751,51.5546187831019));
#44352=CARTESIAN_POINT('Ctrl Pts',(78.5807688690222,448.00349963982,49.4207822496474));
#44353=CARTESIAN_POINT('Ctrl Pts',(76.4436668804944,448.141069050889,48.1479933154738));
#44354=CARTESIAN_POINT('Ctrl Pts',(73.9585827640392,448.278638461958,48.040506039639));
#44355=CARTESIAN_POINT('Ctrl Pts',(71.7195638980013,448.416207873027,49.1240147372739));
#44356=CARTESIAN_POINT('Ctrl Pts',(70.2618369488048,448.553777284096,51.1395118774135));
#44357=CARTESIAN_POINT('Ctrl Pts',(69.9338645164797,448.691346695165,53.6052025846919));
#44358=CARTESIAN_POINT('Ctrl Pts',(70.8140468299362,448.828916106234,55.9316753817396));
#44359=CARTESIAN_POINT('Ctrl Pts',(72.6919805501841,448.966485517303,57.5627981615082));
#44360=CARTESIAN_POINT('Ctrl Pts',(75.1187546742391,449.104054928372,58.1086588865485));
#44361=CARTESIAN_POINT('Ctrl Pts',(77.5142605463483,449.241624339441,57.4387721819374));
#44362=CARTESIAN_POINT('Ctrl Pts',(79.3058640356535,449.37919375051,55.7132712351298));
#44363=CARTESIAN_POINT('Ctrl Pts',(80.0652909647104,449.516763161579,53.3446287294427));
#44364=CARTESIAN_POINT('Ctrl Pts',(79.6110039870512,449.654332572648,50.8990572374897));
#44365=CARTESIAN_POINT('Ctrl Pts',(78.0515982147316,449.791901983717,48.9611588352041));
#44366=CARTESIAN_POINT('Ctrl Pts',(75.7598420802921,449.929471394786,47.9941787937435));
#44367=CARTESIAN_POINT('Ctrl Pts',(73.2835688399409,450.067040805855,48.229269030557));
#44368=CARTESIAN_POINT('Ctrl Pts',(71.2147196745641,450.204610216924,49.6102323578195));
#44369=CARTESIAN_POINT('Ctrl Pts',(70.0478430039696,450.342179627993,51.806956149275));
#44370=CARTESIAN_POINT('Ctrl Pts',(70.0618750711716,450.479749039062,54.2943241721889));
#44371=CARTESIAN_POINT('Ctrl Pts',(71.2534615781489,450.617318450131,56.4777430913874));
#44372=CARTESIAN_POINT('Ctrl Pts',(73.3377595146173,450.7548878612,57.835277139711));
#44373=CARTESIAN_POINT('Ctrl Pts',(75.8165275065125,450.892457272269,58.0424143470898));
#44374=CARTESIAN_POINT('Ctrl Pts',(78.0972280146179,451.030026683338,57.0496395626336));
#44375=CARTESIAN_POINT('Ctrl Pts',(79.6346705769054,451.167596094407,55.0942708127578));
#44376=CARTESIAN_POINT('Ctrl Pts',(80.0613369603159,451.305165505476,52.6437295709924));
#44377=CARTESIAN_POINT('Ctrl Pts',(79.2752346227003,451.442734916545,50.2838059080074));
#44378=CARTESIAN_POINT('Ctrl Pts',(77.4642775383486,451.580304327614,48.5786281990962));
#44379=CARTESIAN_POINT('Ctrl Pts',(75.0613662683072,451.717873738683,47.9358109555334));
#44380=CARTESIAN_POINT('Ctrl Pts',(72.6409051681049,451.855443149752,48.5090165405895));
#44381=CARTESIAN_POINT('Ctrl Pts',(70.7814937955892,451.993012560821,50.1612229224031));
#44382=CARTESIAN_POINT('Ctrl Pts',(69.9276154757779,452.13058197189,52.4974781300291));
#44383=CARTESIAN_POINT('Ctrl Pts',(70.28338570485,452.268151382959,54.9593116184677));
#44384=CARTESIAN_POINT('Ctrl Pts',(71.7637593244369,452.405720794028,56.9582339596125));
#44385=CARTESIAN_POINT('Ctrl Pts',(74.0148601574488,452.543290205097,58.0164124045709));
#44386=CARTESIAN_POINT('Ctrl Pts',(76.4985734007796,452.680859616166,57.8808944956963));
#44387=CARTESIAN_POINT('Ctrl Pts',(78.6211793782641,452.818429027235,56.5840751390796));
#44388=CARTESIAN_POINT('Ctrl Pts',(79.8752793598227,452.955998438304,54.4359527433117));
#44389=CARTESIAN_POINT('Ctrl Pts',(79.9610867979697,453.093567849373,51.9500256275167));
#44390=CARTESIAN_POINT('Ctrl Pts',(78.8580898214202,453.231137260442,49.7205426507378));
#44391=CARTESIAN_POINT('Ctrl Pts',(76.829954576496,453.368706671511,48.2804510471555));
#44392=CARTESIAN_POINT('Ctrl Pts',(74.3614969349096,453.50627608258,47.9739976078481));
#44393=CARTESIAN_POINT('Ctrl Pts',(72.0427899699093,453.643845493649,48.8744389188063));
#44394=CARTESIAN_POINT('Ctrl Pts',(70.4281090065325,453.781414904718,50.7665280353679));
#44395=CARTESIAN_POINT('Ctrl Pts',(69.9034365734981,453.918984315787,53.1979719646065));
#44396=CARTESIAN_POINT('Ctrl Pts',(70.5941911450941,454.056553726855,55.5875419761702));
#44397=CARTESIAN_POINT('Ctrl Pts',(72.3352550969583,454.194123137925,57.3640315940408));
#44398=CARTESIAN_POINT('Ctrl Pts',(74.710425927543,454.331692548993,58.1027615369526));
#44399=CARTESIAN_POINT('Ctrl Pts',(77.1519489117248,454.469261960063,57.627184662743));
#44400=CARTESIAN_POINT('Ctrl Pts',(79.0761421930432,454.606831371131,56.0509002658933));
#44401=CARTESIAN_POINT('Ctrl Pts',(80.023121444939,454.744400782201,53.7509224563649));
#44402=CARTESIAN_POINT('Ctrl Pts',(79.7662753305892,454.881970193269,51.2766510661603));
#44403=CARTESIAN_POINT('Ctrl Pts',(78.8336787086927,454.973683133982,49.9059845082687));
#44404=CARTESIAN_POINT('Ctrl Pts',(78.2325635911202,455.019539604339,49.3717825937627));
#44405=CARTESIAN_POINT('Ctrl Pts',(71.3175296553191,437.980466315892,49.8516638592361));
#44406=CARTESIAN_POINT('Ctrl Pts',(70.7954234783326,438.026322786249,50.4559717068158));
#44407=CARTESIAN_POINT('Ctrl Pts',(70.0560807745525,438.118035726961,51.9269888548089));
#44408=CARTESIAN_POINT('Ctrl Pts',(70.125934541983,438.25560513803,54.3963370242244));
#44409=CARTESIAN_POINT('Ctrl Pts',(71.3581869735604,438.393174549099,56.5370871041277));
#44410=CARTESIAN_POINT('Ctrl Pts',(73.4580893000358,438.530743960168,57.8379270603054));
#44411=CARTESIAN_POINT('Ctrl Pts',(75.9237259676645,438.668313371237,57.9876786635535));
#44412=CARTESIAN_POINT('Ctrl Pts',(78.1656626934283,438.805882782306,56.9506344614431));
#44413=CARTESIAN_POINT('Ctrl Pts',(79.6479878689065,438.943452193375,54.9746504432268));
#44414=CARTESIAN_POINT('Ctrl Pts',(80.0163517461031,439.081021604444,52.5320950318071));
#44415=CARTESIAN_POINT('Ctrl Pts',(79.1827014442556,439.218591015513,50.2068402308956));
#44416=CARTESIAN_POINT('Ctrl Pts',(77.3463156309085,439.356160426582,48.5547309661478));
#44417=CARTESIAN_POINT('Ctrl Pts',(74.946174064172,439.493729837651,47.9706941235349));
#44418=CARTESIAN_POINT('Ctrl Pts',(72.5560187272658,439.63129924872,48.5943417243833));
#44419=CARTESIAN_POINT('Ctrl Pts',(70.7472048541975,439.768868659789,50.2765934305506));
#44420=CARTESIAN_POINT('Ctrl Pts',(69.9521206227429,439.906438070858,52.615315253899));
#44421=CARTESIAN_POINT('Ctrl Pts',(70.3608271113549,440.044007481927,55.0514469370336));
#44422=CARTESIAN_POINT('Ctrl Pts',(71.8756249920409,440.181576892996,57.002642980708));
#44423=CARTESIAN_POINT('Ctrl Pts',(74.1344091390896,440.319146304065,58.0024793602158));
#44424=CARTESIAN_POINT('Ctrl Pts',(76.597228088434,440.456715715134,57.8119500163398));
#44425=CARTESIAN_POINT('Ctrl Pts',(78.6753568437137,440.594285126203,56.4766000668489));
#44426=CARTESIAN_POINT('Ctrl Pts',(79.8720287433716,440.731854537272,54.3156384814752));
#44427=CARTESIAN_POINT('Ctrl Pts',(79.9011851387508,440.869423948341,51.8456327092798));
#44428=CARTESIAN_POINT('Ctrl Pts',(78.7558563339814,441.00699335941,49.65702572342));
#44429=CARTESIAN_POINT('Ctrl Pts',(76.709827658675,441.144562770479,48.2729934732346));
#44430=CARTESIAN_POINT('Ctrl Pts',(74.2521924044753,441.282132181548,48.0243821962769));
#44431=CARTESIAN_POINT('Ctrl Pts',(71.9704364315359,441.419701592617,48.9706212198079));
#44432=CARTESIAN_POINT('Ctrl Pts',(70.4100025056612,441.557271003686,50.8855166667433));
#44433=CARTESIAN_POINT('Ctrl Pts',(69.9439048345445,441.694840414755,53.311322011507));
#44434=CARTESIAN_POINT('Ctrl Pts',(70.6835618195766,441.832409825824,55.6681601803684));
#44435=CARTESIAN_POINT('Ctrl Pts',(72.4521620241055,441.969979236893,57.3926403705265));
#44436=CARTESIAN_POINT('Ctrl Pts',(74.8269300950219,442.107548647962,58.0725339056214));
#44437=CARTESIAN_POINT('Ctrl Pts',(77.2401891728734,442.245118059031,57.5453155136098));
#44438=CARTESIAN_POINT('Ctrl Pts',(79.1150613085509,442.3826874701,55.9370142095725));
#44439=CARTESIAN_POINT('Ctrl Pts',(80.0033673561028,442.520256881169,53.6320866671993));
#44440=CARTESIAN_POINT('Ctrl Pts',(79.6927620370649,442.657826292238,51.1815147042704));
#44441=CARTESIAN_POINT('Ctrl Pts',(78.2574940556369,442.795395703307,49.1710957352006));
#44442=CARTESIAN_POINT('Ctrl Pts',(76.0406573038701,442.932965114376,48.0814107230417));
#44443=CARTESIAN_POINT('Ctrl Pts',(73.5721759207042,443.070534525445,48.1729436169717));
#44444=CARTESIAN_POINT('Ctrl Pts',(71.4421284811268,443.208103936514,49.4238139199439));
#44445=CARTESIAN_POINT('Ctrl Pts',(70.1596925573787,443.345673347583,51.5350071160272));
#44446=CARTESIAN_POINT('Ctrl Pts',(70.031428274871,443.483242758652,54.0018526489985));
#44447=CARTESIAN_POINT('Ctrl Pts',(71.0879965920213,443.620812169721,56.2346629859735));
#44448=CARTESIAN_POINT('Ctrl Pts',(73.0768299459495,443.75838158079,57.6996955794712));
#44449=CARTESIAN_POINT('Ctrl Pts',(75.5225073108471,443.895950991858,58.0467414504097));
#44450=CARTESIAN_POINT('Ctrl Pts',(77.8404013023635,444.033520402927,57.192840956324));
#44451=CARTESIAN_POINT('Ctrl Pts',(79.4764305355575,444.171089813996,55.3421148939791));
#44452=CARTESIAN_POINT('Ctrl Pts',(80.0395101089407,444.308659225066,52.936970406896));
#44453=CARTESIAN_POINT('Ctrl Pts',(79.3950385648993,444.446228636135,50.5523456903779));
#44454=CARTESIAN_POINT('Ctrl Pts',(77.6970737192715,444.583798047203,48.7582737874932));
#44455=CARTESIAN_POINT('Ctrl Pts',(75.3515058831289,444.721367458273,47.983618938053));
#44456=CARTESIAN_POINT('Ctrl Pts',(72.919031740565,444.858936869342,48.4135586494846));
#44457=CARTESIAN_POINT('Ctrl Pts',(70.9811225092794,444.99650628041,49.9453179063543));
#44458=CARTESIAN_POINT('Ctrl Pts',(70.0010260490498,445.13407569148,52.2127370423663));
#44459=CARTESIAN_POINT('Ctrl Pts',(70.2130296940026,445.271645102548,54.6738004434664));
#44460=CARTESIAN_POINT('Ctrl Pts',(71.5664549948049,445.409214513617,56.7402027675205));
#44461=CARTESIAN_POINT('Ctrl Pts',(73.7377721576751,445.546783924686,57.9179805003435));
#44462=CARTESIAN_POINT('Ctrl Pts',(76.2079382819655,445.684353335755,57.9255915525455));
#44463=CARTESIAN_POINT('Ctrl Pts',(78.3864720634444,445.821922746824,56.7612165387878));
#44464=CARTESIAN_POINT('Ctrl Pts',(79.7526055035746,445.959492157893,54.7031936930774));
#44465=CARTESIAN_POINT('Ctrl Pts',(79.9797709891293,446.097061568962,52.2434834556957));
#44466=CARTESIAN_POINT('Ctrl Pts',(79.0136657058697,446.234630980031,49.9700677015131));
#44467=CARTESIAN_POINT('Ctrl Pts',(77.0852324645138,446.3722003911,48.4263955072499));
#44468=CARTESIAN_POINT('Ctrl Pts',(74.6554539351268,446.509769802169,47.9814742694579));
#44469=CARTESIAN_POINT('Ctrl Pts',(72.3051569620732,446.647339213238,48.7416602652266));
#44470=CARTESIAN_POINT('Ctrl Pts',(70.5961687068276,446.784908624307,50.5252346968499));
#44471=CARTESIAN_POINT('Ctrl Pts',(69.9370145733906,446.922478035376,52.9058426944171));
#44472=CARTESIAN_POINT('Ctrl Pts',(70.4852621798161,447.060047446445,55.314411392162));
#44473=CARTESIAN_POINT('Ctrl Pts',(72.109855578692,447.197616857514,57.1751840537294));
#44474=CARTESIAN_POINT('Ctrl Pts',(74.4224435495957,447.335186268583,58.0433519444853));
#44475=CARTESIAN_POINT('Ctrl Pts',(76.8702130862349,447.472755679652,57.7113837152687));
#44476=CARTESIAN_POINT('Ctrl Pts',(78.8680366806898,447.610325090721,56.2586347709747));
#44477=CARTESIAN_POINT('Ctrl Pts',(79.9383442334927,447.74789450179,54.0323777435583));
#44478=CARTESIAN_POINT('Ctrl Pts',(79.8252838837127,447.885463912859,51.5647886434414));
#44479=CARTESIAN_POINT('Ctrl Pts',(78.5558821629415,448.023033323928,49.4457327496502));
#44480=CARTESIAN_POINT('Ctrl Pts',(76.4335834332017,448.160602734997,48.1817601583917));
#44481=CARTESIAN_POINT('Ctrl Pts',(73.9657129750013,448.298172146066,48.0750174244501));
#44482=CARTESIAN_POINT('Ctrl Pts',(71.7422033246598,448.435741557135,49.1510208838061));
#44483=CARTESIAN_POINT('Ctrl Pts',(70.2945737453536,448.573310968204,51.1525570965252));
#44484=CARTESIAN_POINT('Ctrl Pts',(69.9688731095159,448.710880379273,53.6011684796407));
#44485=CARTESIAN_POINT('Ctrl Pts',(70.8429585840585,448.848449790342,55.911526285891));
#44486=CARTESIAN_POINT('Ctrl Pts',(72.7078842499427,448.986019201411,57.5313506190933));
#44487=CARTESIAN_POINT('Ctrl Pts',(75.1178486168725,449.12358861248,58.0734302809844));
#44488=CARTESIAN_POINT('Ctrl Pts',(77.4967613205024,449.261158023549,57.4081837415597));
#44489=CARTESIAN_POINT('Ctrl Pts',(79.2759547469092,449.398727434618,55.694634979155));
#44490=CARTESIAN_POINT('Ctrl Pts',(80.0301212843603,449.536296845687,53.342399565023));
#44491=CARTESIAN_POINT('Ctrl Pts',(79.5789810576424,449.673866256756,50.9137680356334));
#44492=CARTESIAN_POINT('Ctrl Pts',(78.0303769631685,449.811435667825,48.9892930505306));
#44493=CARTESIAN_POINT('Ctrl Pts',(75.7544953444607,449.949005078894,48.0290110777038));
#44494=CARTESIAN_POINT('Ctrl Pts',(73.2953747312671,450.086574489963,48.2624728935843));
#44495=CARTESIAN_POINT('Ctrl Pts',(71.2408560516383,450.224143901032,49.633870576521));
#44496=CARTESIAN_POINT('Ctrl Pts',(70.0820620918462,450.361713312101,51.8153781214214));
#44497=CARTESIAN_POINT('Ctrl Pts',(70.0959969618516,450.49928272317,54.2855166659378));
#44498=CARTESIAN_POINT('Ctrl Pts',(71.2793295981546,450.636852134239,56.4538114986504));
#44499=CARTESIAN_POINT('Ctrl Pts',(73.3491900384668,450.774421545308,57.8019421923663));
#44500=CARTESIAN_POINT('Ctrl Pts',(75.8107881225818,450.911990956377,58.0076446036044));
#44501=CARTESIAN_POINT('Ctrl Pts',(78.0756906949682,451.049560367446,57.0217465625752));
#44502=CARTESIAN_POINT('Ctrl Pts',(79.6024837139754,451.187129778515,55.0799222433284));
#44503=CARTESIAN_POINT('Ctrl Pts',(80.0261946685277,451.324699189584,52.6463553885448));
#44504=CARTESIAN_POINT('Ctrl Pts',(79.2455374974976,451.462268600653,50.3027784235138));
#44505=CARTESIAN_POINT('Ctrl Pts',(77.4471245343519,451.599838011722,48.6094121241844));
#44506=CARTESIAN_POINT('Ctrl Pts',(75.0608577284335,451.737407422791,47.9710475413092));
#44507=CARTESIAN_POINT('Ctrl Pts',(72.6571626563595,451.874976833859,48.5402826510862));
#44508=CARTESIAN_POINT('Ctrl Pts',(70.8106310377763,452.012546244929,50.181044544629));
#44509=CARTESIAN_POINT('Ctrl Pts',(69.962667354613,452.150115655997,52.5011170007442));
#44510=CARTESIAN_POINT('Ctrl Pts',(70.3159732376696,452.287685067066,54.9458978831686));
#44511=CARTESIAN_POINT('Ctrl Pts',(71.7860926186139,452.425254478135,56.9309741070612));
#44512=CARTESIAN_POINT('Ctrl Pts',(74.0216005466695,452.562823889204,57.9818227711066));
#44513=CARTESIAN_POINT('Ctrl Pts',(76.4881096274971,452.700393300274,57.8472435664614));
#44514=CARTESIAN_POINT('Ctrl Pts',(78.5960127570322,452.837962711342,56.5594070064733));
#44515=CARTESIAN_POINT('Ctrl Pts',(79.8414258501443,452.975532122412,54.4261642055509));
#44516=CARTESIAN_POINT('Ctrl Pts',(79.9266389181023,453.113101533481,51.957456587291));
#44517=CARTESIAN_POINT('Ctrl Pts',(78.8312821710664,453.250670944549,49.7434167730967));
#44518=CARTESIAN_POINT('Ctrl Pts',(76.8171953950731,453.388240355619,48.3133003830516));
#44519=CARTESIAN_POINT('Ctrl Pts',(74.3658362436251,453.525809766687,48.0089696826649));
#44520=CARTESIAN_POINT('Ctrl Pts',(72.0631904771268,453.663379177756,48.9031738248679));
#44521=CARTESIAN_POINT('Ctrl Pts',(70.4596940712907,453.800948588825,50.7821568355942));
#44522=CARTESIAN_POINT('Ctrl Pts',(69.9386559345355,453.938517999894,53.1967586609433));
#44523=CARTESIAN_POINT('Ctrl Pts',(70.6246257935922,454.076087410963,55.5697766204929));
#44524=CARTESIAN_POINT('Ctrl Pts',(72.3536297593703,454.213656822032,57.3339608660936));
#44525=CARTESIAN_POINT('Ctrl Pts',(74.712348278058,454.351226233101,58.0675737810965));
#44526=CARTESIAN_POINT('Ctrl Pts',(77.1369593428433,454.48879564417,57.5952911284919));
#44527=CARTESIAN_POINT('Ctrl Pts',(79.0478241394874,454.626365055239,56.029925324192));
#44528=CARTESIAN_POINT('Ctrl Pts',(79.9882438640382,454.763934466308,53.7458789802202));
#44529=CARTESIAN_POINT('Ctrl Pts',(79.7331768690378,454.901503877377,51.2887463507757));
#44530=CARTESIAN_POINT('Ctrl Pts',(78.8070401490145,454.99321681809,49.9275741136407));
#44531=CARTESIAN_POINT('Ctrl Pts',(78.2100888302193,455.039073288446,49.3970725041402));
#44532=CARTESIAN_POINT('Ctrl Pts',(71.3431312258736,438.,49.8737829466856));
#44533=CARTESIAN_POINT('Ctrl Pts',(70.8246667948602,438.045856470356,50.4738756829193));
#44534=CARTESIAN_POINT('Ctrl Pts',(70.0904810848736,438.137569411069,51.9346323302495));
#44535=CARTESIAN_POINT('Ctrl Pts',(70.1598476148656,438.275138822138,54.3867565342177));
#44536=CARTESIAN_POINT('Ctrl Pts',(71.3835049550069,438.412708233207,56.5125746552081));
#44537=CARTESIAN_POINT('Ctrl Pts',(73.4687602399829,438.550277644276,57.8043411146894));
#44538=CARTESIAN_POINT('Ctrl Pts',(75.9171988302832,438.687847055345,57.9530481846181));
#44539=CARTESIAN_POINT('Ctrl Pts',(78.1434978095446,438.825416466414,56.9232374758342));
#44540=CARTESIAN_POINT('Ctrl Pts',(79.6154836096685,438.962985877483,54.9610361557711));
#44541=CARTESIAN_POINT('Ctrl Pts',(79.9812781097431,439.100555288552,52.5355178274692));
#44542=CARTESIAN_POINT('Ctrl Pts',(79.1534426071904,439.238124699621,50.2264819254732));
#44543=CARTESIAN_POINT('Ctrl Pts',(77.3298657797079,439.37569411069,48.5858962981143));
#44544=CARTESIAN_POINT('Ctrl Pts',(74.946465455023,439.513263521759,48.0059331744372));
#44545=CARTESIAN_POINT('Ctrl Pts',(72.5729817051559,439.650832932828,48.6252307671089));
#44546=CARTESIAN_POINT('Ctrl Pts',(70.7767845007438,439.788402343897,50.2957485891607));
#44547=CARTESIAN_POINT('Ctrl Pts',(69.9872460661516,439.925971754966,52.6181575796835));
#44548=CARTESIAN_POINT('Ctrl Pts',(70.3931017836471,440.063541166035,55.0372969858864));
#44549=CARTESIAN_POINT('Ctrl Pts',(71.8973337884151,440.201110577104,56.9748832301599));
#44550=CARTESIAN_POINT('Ctrl Pts',(74.1403626764107,440.338679988173,57.967745644851));
#44551=CARTESIAN_POINT('Ctrl Pts',(76.5860032023106,440.476249399242,57.7785452633612));
#44552=CARTESIAN_POINT('Ctrl Pts',(78.6496367890598,440.613818810311,56.4525095214311));
#44553=CARTESIAN_POINT('Ctrl Pts',(79.8379617752664,440.75138822138,54.3066208723653));
#44554=CARTESIAN_POINT('Ctrl Pts',(79.8669148016947,440.888957632449,51.8538436524662));
#44555=CARTESIAN_POINT('Ctrl Pts',(78.729574786843,441.026527043518,49.6805024325154));
#44556=CARTESIAN_POINT('Ctrl Pts',(76.6978173786037,441.164096454587,48.3061239541028));
#44557=CARTESIAN_POINT('Ctrl Pts',(74.257324391025,441.301665865656,48.0592467671762));
#44558=CARTESIAN_POINT('Ctrl Pts',(71.9914839080614,441.439235276725,48.9988856731345));
#44559=CARTESIAN_POINT('Ctrl Pts',(70.4419341743612,441.576804687793,50.9004245211821));
#44560=CARTESIAN_POINT('Ctrl Pts',(69.9790875839475,441.714374098863,53.3093096163199));
#44561=CARTESIAN_POINT('Ctrl Pts',(70.713585383041,441.851943509931,55.6497085889238));
#44562=CARTESIAN_POINT('Ctrl Pts',(72.4698494135181,441.989512921,57.3621603468108));
#44563=CARTESIAN_POINT('Ctrl Pts',(74.828053225208,442.127082332069,58.0373115523705));
#44564=CARTESIAN_POINT('Ctrl Pts',(77.2244795649762,442.264651743138,57.5137705645742));
#44565=CARTESIAN_POINT('Ctrl Pts',(79.0862742686079,442.402221154207,55.9166873327523));
#44566=CARTESIAN_POINT('Ctrl Pts',(79.9683842872405,442.539790565276,53.6278369045098));
#44567=CARTESIAN_POINT('Ctrl Pts',(79.6599454732541,442.677359976345,51.194357940996));
#44568=CARTESIAN_POINT('Ctrl Pts',(78.2346886382596,442.814929387414,49.1979618575147));
#44569=CARTESIAN_POINT('Ctrl Pts',(76.0333145580138,442.952498798483,48.1158775139168));
#44570=CARTESIAN_POINT('Ctrl Pts',(73.5820510943691,443.090068209552,48.2067719562013));
#44571=CARTESIAN_POINT('Ctrl Pts',(71.466860961653,443.227637620621,49.4489173061093));
#44572=CARTESIAN_POINT('Ctrl Pts',(70.1933701645227,443.36520703169,51.5453847056798));
#44573=CARTESIAN_POINT('Ctrl Pts',(70.0660005389926,443.502776442759,53.9950237293587));
#44574=CARTESIAN_POINT('Ctrl Pts',(71.1151991800427,443.640345853828,56.2122599773613));
#44575=CARTESIAN_POINT('Ctrl Pts',(73.090160210338,443.777915264897,57.6670738130985));
#44576=CARTESIAN_POINT('Ctrl Pts',(75.5187787161611,443.915484675966,58.0116990022701));
#44577=CARTESIAN_POINT('Ctrl Pts',(77.8205051511885,444.053054087035,57.1637545547184));
#44578=CARTESIAN_POINT('Ctrl Pts',(79.4451229069195,444.190623498104,55.3259375029962));
#44579=CARTESIAN_POINT('Ctrl Pts',(80.004274940543,444.328192909173,52.9375691538648));
#44580=CARTESIAN_POINT('Ctrl Pts',(79.3642986538913,444.465762320242,50.569577447722));
#44581=CARTESIAN_POINT('Ctrl Pts',(77.6781772931937,444.603331731311,48.7880193866875));
#44582=CARTESIAN_POINT('Ctrl Pts',(75.3489700415422,444.74090114238,48.0187678370029));
#44583=CARTESIAN_POINT('Ctrl Pts',(72.9334626641764,444.878470553449,48.4457086733363));
#44584=CARTESIAN_POINT('Ctrl Pts',(71.0090705553659,445.016039964518,49.9667837468897));
#44585=CARTESIAN_POINT('Ctrl Pts',(70.0358103719218,445.153609375587,52.2183873938844));
#44586=CARTESIAN_POINT('Ctrl Pts',(70.2463352689603,445.291178786656,54.6622846166753));
#44587=CARTESIAN_POINT('Ctrl Pts',(71.5903202847087,445.428748197725,56.7142735653008));
#44588=CARTESIAN_POINT('Ctrl Pts',(73.7464922800195,445.566317608794,57.8838361734905));
#44589=CARTESIAN_POINT('Ctrl Pts',(76.1994287335407,445.703887019863,57.891394137796));
#44590=CARTESIAN_POINT('Ctrl Pts',(78.3627670107798,445.841456430932,56.7351407632842));
#44591=CARTESIAN_POINT('Ctrl Pts',(79.7193715252362,445.979025842001,54.691472845252));
#44592=CARTESIAN_POINT('Ctrl Pts',(79.9449525074299,446.11659525307,52.2489193477191));
#44593=CARTESIAN_POINT('Ctrl Pts',(78.9855859110121,446.254164664139,49.9913609096016));
#44594=CARTESIAN_POINT('Ctrl Pts',(77.0706036960962,446.391734075208,48.4584559926568));
#44595=CARTESIAN_POINT('Ctrl Pts',(74.6577731297195,446.529303486277,48.0166381276987));
#44596=CARTESIAN_POINT('Ctrl Pts',(72.3238697273887,446.666872897346,48.7715217455012));
#44597=CARTESIAN_POINT('Ctrl Pts',(70.6268018465247,446.804442308415,50.54265555625));
#44598=CARTESIAN_POINT('Ctrl Pts',(69.9722453830961,446.942011719484,52.9066585604828));
#44599=CARTESIAN_POINT('Ctrl Pts',(70.5166689043049,447.079581130553,55.2984272360433));
#44600=CARTESIAN_POINT('Ctrl Pts',(72.1299305918756,447.217150541622,57.1462208108926));
#44601=CARTESIAN_POINT('Ctrl Pts',(74.4263880163468,447.354719952691,58.0083331385092));
#44602=CARTESIAN_POINT('Ctrl Pts',(76.8570841007916,447.49228936376,57.6786804229088));
#44603=CARTESIAN_POINT('Ctrl Pts',(78.8409726637322,447.629858774829,56.236064556619));
#44604=CARTESIAN_POINT('Ctrl Pts',(79.9038147078087,447.767428185898,54.0253359081455));
#44605=CARTESIAN_POINT('Ctrl Pts',(79.7915429659626,447.904997596967,51.5749585037809));
#44606=CARTESIAN_POINT('Ctrl Pts',(78.5309954568607,448.042567008036,49.4706832496531));
#44607=CARTESIAN_POINT('Ctrl Pts',(76.423499985909,448.180136419105,48.2155270013095));
#44608=CARTESIAN_POINT('Ctrl Pts',(73.9728431859633,448.317705830174,48.1095288092612));
#44609=CARTESIAN_POINT('Ctrl Pts',(71.7648427513183,448.455275241243,49.1780270303383));
#44610=CARTESIAN_POINT('Ctrl Pts',(70.3273105419023,448.592844652312,51.1656023156368));
#44611=CARTESIAN_POINT('Ctrl Pts',(70.0038817025521,448.730414063381,53.5971343745895));
#44612=CARTESIAN_POINT('Ctrl Pts',(70.8718703381808,448.86798347445,55.8913771900424));
#44613=CARTESIAN_POINT('Ctrl Pts',(72.7237879497012,449.005552885519,57.4999030766785));
#44614=CARTESIAN_POINT('Ctrl Pts',(75.116942559506,449.143122296588,58.0382016754203));
#44615=CARTESIAN_POINT('Ctrl Pts',(77.4792620946565,449.280691707657,57.377595301182));
#44616=CARTESIAN_POINT('Ctrl Pts',(79.246045458165,449.418261118726,55.6759987231803));
#44617=CARTESIAN_POINT('Ctrl Pts',(79.9949516040101,449.555830529795,53.3401704006032));
#44618=CARTESIAN_POINT('Ctrl Pts',(79.5469581282337,449.693399940864,50.9284788337772));
#44619=CARTESIAN_POINT('Ctrl Pts',(78.0091557116053,449.830969351933,49.0174272658571));
#44620=CARTESIAN_POINT('Ctrl Pts',(75.7491486086294,449.968538763002,48.0638433616641));
#44621=CARTESIAN_POINT('Ctrl Pts',(73.3071806225934,450.10610817407,48.2956767566116));
#44622=CARTESIAN_POINT('Ctrl Pts',(71.2669924287125,450.24367758514,49.6575087952225));
#44623=CARTESIAN_POINT('Ctrl Pts',(70.1162811797229,450.381246996208,51.8238000935677));
#44624=CARTESIAN_POINT('Ctrl Pts',(70.1301188525317,450.518816407277,54.2767091596868));
#44625=CARTESIAN_POINT('Ctrl Pts',(71.3051976181603,450.656385818346,56.4298799059135));
#44626=CARTESIAN_POINT('Ctrl Pts',(73.3606205623162,450.793955229416,57.7686072450216));
#44627=CARTESIAN_POINT('Ctrl Pts',(75.8050487386511,450.931524640484,57.972874860119));
#44628=CARTESIAN_POINT('Ctrl Pts',(78.0541533753186,451.069094051554,56.9938535625169));
#44629=CARTESIAN_POINT('Ctrl Pts',(79.5702968510455,451.206663462622,55.065573673899));
#44630=CARTESIAN_POINT('Ctrl Pts',(79.9910523767396,451.344232873691,52.6489812060971));
#44631=CARTESIAN_POINT('Ctrl Pts',(79.2158403722948,451.48180228476,50.3217509390201));
#44632=CARTESIAN_POINT('Ctrl Pts',(77.4299715303552,451.619371695829,48.6401960492725));
#44633=CARTESIAN_POINT('Ctrl Pts',(75.0603491885598,451.756941106898,48.0062841270851));
#44634=CARTESIAN_POINT('Ctrl Pts',(72.6734201446142,451.894510517967,48.571548761583));
#44635=CARTESIAN_POINT('Ctrl Pts',(70.8397682799635,452.032079929036,50.2008661668549));
#44636=CARTESIAN_POINT('Ctrl Pts',(69.997719233448,452.169649340105,52.5047558714594));
#44637=CARTESIAN_POINT('Ctrl Pts',(70.3485607704892,452.307218751174,54.9324841478696));
#44638=CARTESIAN_POINT('Ctrl Pts',(71.808425912791,452.444788162243,56.9037142545098));
#44639=CARTESIAN_POINT('Ctrl Pts',(74.0283409358903,452.582357573312,57.9472331376422));
#44640=CARTESIAN_POINT('Ctrl Pts',(76.4776458542147,452.719926984381,57.8135926372266));
#44641=CARTESIAN_POINT('Ctrl Pts',(78.5708461358004,452.85749639545,56.5347388738669));
#44642=CARTESIAN_POINT('Ctrl Pts',(79.8075723404659,452.995065806519,54.4163756677902));
#44643=CARTESIAN_POINT('Ctrl Pts',(79.8921910382349,453.132635217588,51.9648875470652));
#44644=CARTESIAN_POINT('Ctrl Pts',(78.8044745207126,453.270204628657,49.7662908954556));
#44645=CARTESIAN_POINT('Ctrl Pts',(76.8044362136501,453.407774039726,48.3461497189478));
#44646=CARTESIAN_POINT('Ctrl Pts',(74.3701755523407,453.545343450795,48.0439417574817));
#44647=CARTESIAN_POINT('Ctrl Pts',(72.0835909843443,453.682912861864,48.9319087309295));
#44648=CARTESIAN_POINT('Ctrl Pts',(70.4912791360489,453.820482272933,50.7977856358205));
#44649=CARTESIAN_POINT('Ctrl Pts',(69.9738752955729,453.958051684002,53.19554535728));
#44650=CARTESIAN_POINT('Ctrl Pts',(70.6550604420902,454.095621095071,55.5520112648156));
#44651=CARTESIAN_POINT('Ctrl Pts',(72.3720044217823,454.23319050614,57.3038901381464));
#44652=CARTESIAN_POINT('Ctrl Pts',(74.714270628573,454.370759917209,58.0323860252404));
#44653=CARTESIAN_POINT('Ctrl Pts',(77.1219697739619,454.508329328278,57.5633975942407));
#44654=CARTESIAN_POINT('Ctrl Pts',(79.0195060859316,454.645898739347,56.0089503824907));
#44655=CARTESIAN_POINT('Ctrl Pts',(79.9533662831374,454.783468150416,53.7408355040756));
#44656=CARTESIAN_POINT('Ctrl Pts',(79.7000784074864,454.921037561485,51.3008416353911));
#44657=CARTESIAN_POINT('Ctrl Pts',(78.7804015893363,455.012750502198,49.9491637190126));
#44658=CARTESIAN_POINT('Ctrl Pts',(78.1876140693184,455.058606972554,49.4223624145177));
#44659=CARTESIAN_POINT('Origin',(74.9879498948689,416.,53.0228109606356));
#44660=CARTESIAN_POINT('Origin',(74.9879498948689,416.,53.0228109606356));
#44661=CARTESIAN_POINT('Ctrl Pts',(79.8830110631999,416.,55.8460953909448));
#44662=CARTESIAN_POINT('Ctrl Pts',(79.9838735321605,416.,55.7696158752547));
#44663=CARTESIAN_POINT('Ctrl Pts',(80.0818868713731,416.,55.68934340634));
#44664=CARTESIAN_POINT('Ctrl Pts',(80.1769367937531,416.,55.6056077868176));
#44665=CARTESIAN_POINT('Ctrl Pts',(80.2608081582141,416.,55.5317200814152));
#44666=CARTESIAN_POINT('Ctrl Pts',(80.3423725986366,416.,55.455135757001));
#44667=CARTESIAN_POINT('Ctrl Pts',(80.4215638414298,416.,55.376071154289));
#44668=CARTESIAN_POINT('Ctrl Pts',(80.4575782080312,416.,55.3401143807011));
#44669=CARTESIAN_POINT('Ctrl Pts',(80.4930951080665,416.,55.3036512767701));
#44670=CARTESIAN_POINT('Ctrl Pts',(80.5281101864556,416.,55.2667013119425));
#44671=CARTESIAN_POINT('Ctrl Pts',(80.57650767122,416.,55.2156294468473));
#44672=CARTESIAN_POINT('Ctrl Pts',(80.6239470702437,416.,55.1636271224708));
#44673=CARTESIAN_POINT('Ctrl Pts',(80.6704271942508,416.,55.1107322929466));
#44674=CARTESIAN_POINT('Ctrl Pts',(80.7785625890765,416.,54.9876731704287));
#44675=CARTESIAN_POINT('Ctrl Pts',(80.8814898413737,416.,54.8598021724764));
#44676=CARTESIAN_POINT('Ctrl Pts',(80.9790755347001,416.,54.7276983390789));
#44677=CARTESIAN_POINT('Ctrl Pts',(81.0522648046949,416.,54.6286204640308));
#44678=CARTESIAN_POINT('Ctrl Pts',(81.1224501122421,416.,54.5271604110985));
#44679=CARTESIAN_POINT('Ctrl Pts',(81.1895813378797,416.,54.4235414927863));
#44680=CARTESIAN_POINT('Ctrl Pts',(81.2246388416095,416.,54.3694292584168));
#44681=CARTESIAN_POINT('Ctrl Pts',(81.2588635076428,416.,54.3147279697757));
#44682=CARTESIAN_POINT('Ctrl Pts',(81.2922484633112,416.,54.2594675418588));
#44683=CARTESIAN_POINT('Ctrl Pts',(81.3126684070658,416.,54.2256674421632));
#44684=CARTESIAN_POINT('Ctrl Pts',(81.3327776128819,416.,54.1916520339595));
#44685=CARTESIAN_POINT('Ctrl Pts',(81.3525561249044,416.,54.1574603450589));
#44686=CARTESIAN_POINT('Ctrl Pts',(81.4319376986157,416.,54.0202311101349));
#44687=CARTESIAN_POINT('Ctrl Pts',(81.5060371326813,416.,53.8800954269512));
#44688=CARTESIAN_POINT('Ctrl Pts',(81.5748188145443,416.,53.7375264352072));
#44689=CARTESIAN_POINT('Ctrl Pts',(81.6218375223006,416.,53.6400672051279));
#44690=CARTESIAN_POINT('Ctrl Pts',(81.6663714865911,416.,53.541469744288));
#44691=CARTESIAN_POINT('Ctrl Pts',(81.7084103241663,416.,53.4418712821641));
#44692=CARTESIAN_POINT('Ctrl Pts',(81.7726557132268,416.,53.2896610328314));
#44693=CARTESIAN_POINT('Ctrl Pts',(81.8310745560022,416.,53.1351152483158));
#44694=CARTESIAN_POINT('Ctrl Pts',(81.8837208336072,416.,52.9786103674316));
#44695=CARTESIAN_POINT('Ctrl Pts',(81.9370199527937,416.,52.8201647435625));
#44696=CARTESIAN_POINT('Ctrl Pts',(81.9844030717354,416.,52.6597108152884));
#44697=CARTESIAN_POINT('Ctrl Pts',(82.0259096346253,416.,52.4975874466145));
#44698=CARTESIAN_POINT('Ctrl Pts',(82.0553577168838,416.,52.3825641354963));
#44699=CARTESIAN_POINT('Ctrl Pts',(82.0818474251191,416.,52.2666993851232));
#44700=CARTESIAN_POINT('Ctrl Pts',(82.1053853897379,416.,52.1501002183919));
#44701=CARTESIAN_POINT('Ctrl Pts',(82.1113952199384,416.,52.1203295391966));
#44702=CARTESIAN_POINT('Ctrl Pts',(82.1172128280547,416.,52.0905092581177));
#44703=CARTESIAN_POINT('Ctrl Pts',(82.1228344363168,416.,52.0606624486299));
#44704=CARTESIAN_POINT('Ctrl Pts',(82.1554961379767,416.,51.8872516484573));
#44705=CARTESIAN_POINT('Ctrl Pts',(82.1815754911756,416.,51.7127917293179));
#44706=CARTESIAN_POINT('Ctrl Pts',(82.201164328218,416.,51.5377077735356));
#44707=CARTESIAN_POINT('Ctrl Pts',(82.22123206082,416.,51.3583434753921));
#44708=CARTESIAN_POINT('Ctrl Pts',(82.2344886373556,416.,51.178323981131));
#44709=CARTESIAN_POINT('Ctrl Pts',(82.2410141947413,416.,50.998054756671));
#44710=CARTESIAN_POINT('Ctrl Pts',(82.2476113248581,416.,50.8158083278175));
#44711=CARTESIAN_POINT('Ctrl Pts',(82.247329519956,416.,50.6333061826993));
#44712=CARTESIAN_POINT('Ctrl Pts',(82.2402241682398,416.,50.4509211223708));
#44713=CARTESIAN_POINT('Ctrl Pts',(82.2330496544919,416.,50.2667607633897));
#44714=CARTESIAN_POINT('Ctrl Pts',(82.2189186386138,416.,50.0827192120228));
#44715=CARTESIAN_POINT('Ctrl Pts',(82.1978521894802,416.,49.8991414119943));
#44716=CARTESIAN_POINT('Ctrl Pts',(82.1889738216336,416.,49.8217733075366));
#44717=CARTESIAN_POINT('Ctrl Pts',(82.1788631247121,416.,49.7444871533955));
#44718=CARTESIAN_POINT('Ctrl Pts',(82.1675194498641,416.,49.6673071229107));
#44719=CARTESIAN_POINT('Ctrl Pts',(80.1006187634621,416.611326082532,50.6333111614898));
#44720=CARTESIAN_POINT('Ctrl Pts',(80.4987738037364,416.505248077756,51.4852195316062));
#44721=CARTESIAN_POINT('Ctrl Pts',(80.8500414041054,416.293092068204,53.3832855022525));
#44722=CARTESIAN_POINT('Ctrl Pts',(79.6907686422404,415.868780049099,57.1038140873438));
#44723=CARTESIAN_POINT('Ctrl Pts',(75.0514316659349,415.338390025218,59.6975379999433));
#44724=CARTESIAN_POINT('Ctrl Pts',(69.3998575284373,414.701921996561,56.6778047341864));
#44725=CARTESIAN_POINT('Ctrl Pts',(68.8933949361463,414.065453967904,50.30071708643));
#44726=CARTESIAN_POINT('Ctrl Pts',(73.9883328942991,413.428985939247,46.4204917324893));
#44727=CARTESIAN_POINT('Ctrl Pts',(78.9900558741506,412.898595915367,48.2517506338942));
#44728=CARTESIAN_POINT('Ctrl Pts',(80.7106490634504,412.474283896262,51.7314515919306));
#44729=CARTESIAN_POINT('Ctrl Pts',(80.6505859354663,412.049971877158,55.6129833562453));
#44730=CARTESIAN_POINT('Ctrl Pts',(76.922041457819,411.519581853277,59.4142434298776));
#44731=CARTESIAN_POINT('Ctrl Pts',(70.6502604163708,410.88311382462,58.0990212603595));
#44732=CARTESIAN_POINT('Ctrl Pts',(68.3768445575805,410.246645795963,52.120585584734));
#44733=CARTESIAN_POINT('Ctrl Pts',(72.1690405094426,409.610177767306,46.9698855255472));
#44734=CARTESIAN_POINT('Ctrl Pts',(78.5640475947216,408.973709738649,47.3834241974277));
#44735=CARTESIAN_POINT('Ctrl Pts',(81.1373488053079,408.443319714768,52.0445771336779));
#44736=CARTESIAN_POINT('Ctrl Pts',(80.1556395568995,408.019007695663,55.8005301909727));
#44737=CARTESIAN_POINT('Ctrl Pts',(77.5645627245594,407.594695676559,58.6914128709184));
#44738=CARTESIAN_POINT('Ctrl Pts',(72.2572669003642,407.064305652677,59.1166316929431));
#44739=CARTESIAN_POINT('Ctrl Pts',(68.3843315795067,406.427837624022,54.0109585396062));
#44740=CARTESIAN_POINT('Ctrl Pts',(70.5882295550609,405.791369595364,48.0065658313019));
#44741=CARTESIAN_POINT('Ctrl Pts',(76.8287342059321,405.154901566707,46.6044208685245));
#44742=CARTESIAN_POINT('Ctrl Pts',(81.3858076212758,404.51843353805,51.1100412325878));
#44743=CARTESIAN_POINT('Ctrl Pts',(80.2721801274972,403.988043514169,56.3165759506076));
#44744=CARTESIAN_POINT('Ctrl Pts',(77.0681164794659,403.563731495065,58.5085806146201));
#44745=CARTESIAN_POINT('Ctrl Pts',(73.2162245052195,403.13941947596,58.9921464057559));
#44746=CARTESIAN_POINT('Ctrl Pts',(68.9304046244017,402.609029452079,55.8330454857165));
#44747=CARTESIAN_POINT('Ctrl Pts',(69.3542790093376,401.972561423423,49.4386835020307));
#44748=CARTESIAN_POINT('Ctrl Pts',(74.9554640876222,401.336093394765,46.3505401944445));
#44749=CARTESIAN_POINT('Ctrl Pts',(80.5864538842716,400.699625366109,49.3839965362696));
#44750=CARTESIAN_POINT('Ctrl Pts',(81.0725721437252,400.063157337451,55.7739279658411));
#44751=CARTESIAN_POINT('Ctrl Pts',(76.817716662541,399.53276731357,58.9746115424238));
#44752=CARTESIAN_POINT('Ctrl Pts',(72.9612986351318,399.108455294466,58.5285757956383));
#44753=CARTESIAN_POINT('Ctrl Pts',(69.7360426834167,398.684143275361,56.3678740736957));
#44754=CARTESIAN_POINT('Ctrl Pts',(68.5717701362819,398.153753251481,51.1724299186502));
#44755=CARTESIAN_POINT('Ctrl Pts',(73.0847550464725,397.517285222823,46.622649502512));
#44756=CARTESIAN_POINT('Ctrl Pts',(79.3386165734188,396.880817194168,47.96396208343));
#44757=CARTESIAN_POINT('Ctrl Pts',(81.6008775563583,396.244349165509,53.9466102164501));
#44758=CARTESIAN_POINT('Ctrl Pts',(77.7778399493888,395.607881136854,59.0897530386598));
#44759=CARTESIAN_POINT('Ctrl Pts',(72.4666579798875,395.077491112972,58.7162338035805));
#44760=CARTESIAN_POINT('Ctrl Pts',(69.8475504599716,394.653179093868,55.8507175000904));
#44761=CARTESIAN_POINT('Ctrl Pts',(68.8293227947622,394.228867074763,52.1045033700332));
#44762=CARTESIAN_POINT('Ctrl Pts',(71.3570971813203,393.698477050882,47.4185107128847));
#44763=CARTESIAN_POINT('Ctrl Pts',(77.7478064874976,393.062009022225,46.942727991698));
#44764=CARTESIAN_POINT('Ctrl Pts',(81.5899196973729,392.425540993568,52.0562463030878));
#44765=CARTESIAN_POINT('Ctrl Pts',(79.3749321908379,391.789072964911,58.056557443713));
#44766=CARTESIAN_POINT('Ctrl Pts',(73.1160470792531,391.152604936255,59.4327448560289));
#44767=CARTESIAN_POINT('Ctrl Pts',(69.3510454836729,390.622214912373,55.6680491820767));
#44768=CARTESIAN_POINT('Ctrl Pts',(69.2526248134902,390.197902893269,51.7871702535196));
#44769=CARTESIAN_POINT('Ctrl Pts',(70.9403623007099,389.773590874164,48.2911081744554));
#44770=CARTESIAN_POINT('Ctrl Pts',(75.9215609897948,389.243200850283,46.4107278533347));
#44771=CARTESIAN_POINT('Ctrl Pts',(81.0585138063054,388.606732821626,50.2420788415338));
#44772=CARTESIAN_POINT('Ctrl Pts',(80.6062231907216,387.97026479297,56.6221522453024));
#44773=CARTESIAN_POINT('Ctrl Pts',(74.9993426234548,387.333796764312,59.6999426447327));
#44774=CARTESIAN_POINT('Ctrl Pts',(69.3714963501972,386.697328735656,56.6348356387029));
#44775=CARTESIAN_POINT('Ctrl Pts',(68.9975455437743,386.166938711775,51.323684037913));
#44776=CARTESIAN_POINT('Ctrl Pts',(71.4680383649468,385.742626692671,48.3290933969452));
#44777=CARTESIAN_POINT('Ctrl Pts',(75.0347408347962,385.318314673565,46.7962720185687));
#44778=CARTESIAN_POINT('Ctrl Pts',(80.0285504932429,384.787924649685,48.6429001964653));
#44779=CARTESIAN_POINT('Ctrl Pts',(81.3946131522726,384.151456621028,54.9040029304442));
#44780=CARTESIAN_POINT('Ctrl Pts',(76.8695434714302,383.514988592372,59.4243621885054));
#44781=CARTESIAN_POINT('Ctrl Pts',(70.6181705596548,382.878520563713,58.0714985012323));
#44782=CARTESIAN_POINT('Ctrl Pts',(68.3790371462131,382.242052535058,52.0670154934588));
#44783=CARTESIAN_POINT('Ctrl Pts',(71.5793749741399,381.711662511176,47.8118999463395));
#44784=CARTESIAN_POINT('Ctrl Pts',(75.4082269213871,381.287350492072,47.1709626229601));
#44785=CARTESIAN_POINT('Ctrl Pts',(79.1061915643167,380.863038472967,48.3524724138965));
#44786=CARTESIAN_POINT('Ctrl Pts',(81.6656194182121,380.332648449087,53.0212516540086));
#44787=CARTESIAN_POINT('Ctrl Pts',(78.5914140932141,379.696180420429,58.6441331442757));
#44788=CARTESIAN_POINT('Ctrl Pts',(72.2108730876569,379.059712391772,59.0897786478119));
#44789=CARTESIAN_POINT('Ctrl Pts',(68.3782131572467,378.423244363116,53.9691711353926));
#44790=CARTESIAN_POINT('Ctrl Pts',(70.6249796526406,377.786776334458,47.9675401113284));
#44791=CARTESIAN_POINT('Ctrl Pts',(75.8314238903965,377.256386310578,46.8534894251665));
#44792=CARTESIAN_POINT('Ctrl Pts',(79.1424775432099,376.832074291473,48.8802680501344));
#44793=CARTESIAN_POINT('Ctrl Pts',(81.1596824003675,376.407762272369,52.1971630515926));
#44794=CARTESIAN_POINT('Ctrl Pts',(80.0305954546256,375.877372248488,57.4003671799305));
#44795=CARTESIAN_POINT('Ctrl Pts',(74.0224987859417,375.240904219831,59.6297861745523));
#44796=CARTESIAN_POINT('Ctrl Pts',(68.9129848210706,374.604436191174,55.7823493029185));
#44797=CARTESIAN_POINT('Ctrl Pts',(69.3770612241408,373.967968162517,49.4031223489269));
#44798=CARTESIAN_POINT('Ctrl Pts',(75.0088003293896,373.331500133859,46.3451738071356));
#44799=CARTESIAN_POINT('Ctrl Pts',(79.6701661503711,372.80111010998,48.9180786276028));
#44800=CARTESIAN_POINT('Ctrl Pts',(80.8409879526845,372.376798090874,52.6194411056188));
#44801=CARTESIAN_POINT('Ctrl Pts',(80.1889921249218,371.95248607177,56.446425470235));
#44802=CARTESIAN_POINT('Ctrl Pts',(75.9246488708189,371.422096047889,59.6344573307068));
#44803=CARTESIAN_POINT('Ctrl Pts',(69.926659556592,370.785628019232,57.377986896543));
#44804=CARTESIAN_POINT('Ctrl Pts',(68.5918611198335,370.149159990575,51.1227317801111));
#44805=CARTESIAN_POINT('Ctrl Pts',(73.125273998855,369.512691961918,46.610739857829));
#44806=CARTESIAN_POINT('Ctrl Pts',(79.3824041844943,368.876223933261,47.9948845301062));
#44807=CARTESIAN_POINT('Ctrl Pts',(81.2145980287447,368.345833909381,52.9940080782184));
#44808=CARTESIAN_POINT('Ctrl Pts',(79.6714791919269,367.921521890276,56.5562674935186));
#44809=CARTESIAN_POINT('Ctrl Pts',(76.6697640348178,367.497209871172,59.0180989260132));
#44810=CARTESIAN_POINT('Ctrl Pts',(71.359714904182,366.96681984729,58.6288062823227));
#44811=CARTESIAN_POINT('Ctrl Pts',(68.3108789861652,366.330351818634,52.9921286989546));
#44812=CARTESIAN_POINT('Ctrl Pts',(71.4048542721186,365.693883789976,47.3941629641248));
#44813=CARTESIAN_POINT('Ctrl Pts',(77.7862076759328,365.05741576132,46.9603056442045));
#44814=CARTESIAN_POINT('Ctrl Pts',(81.602702521873,364.420947732662,52.10830542322));
#44815=CARTESIAN_POINT('Ctrl Pts',(79.7079398513482,363.890557708783,57.0840510914171));
#44816=CARTESIAN_POINT('Ctrl Pts',(76.2070166523586,363.466245689677,58.7616817543507));
#44817=CARTESIAN_POINT('Ctrl Pts',(72.3264382459639,363.041933670573,58.6520500150618));
#44818=CARTESIAN_POINT('Ctrl Pts',(68.572635003179,362.511543646692,54.8761882926657));
#44819=CARTESIAN_POINT('Ctrl Pts',(69.9668979799986,361.875075618035,48.6213049695892));
#44820=CARTESIAN_POINT('Ctrl Pts',(75.9735829643599,361.238607589378,46.4236610182017));
#44821=CARTESIAN_POINT('Ctrl Pts',(81.0759804481833,360.602139560721,50.2805306498451));
#44822=CARTESIAN_POINT('Ctrl Pts',(80.5817375779959,359.965671532064,56.6698387985494));
#44823=CARTESIAN_POINT('Ctrl Pts',(75.8884619818927,359.435281508183,59.184065262339));
#44824=CARTESIAN_POINT('Ctrl Pts',(72.1452050445395,359.010969489079,58.1550193997093));
#44825=CARTESIAN_POINT('Ctrl Pts',(69.2872670440879,358.586657469974,55.5276446125861));
#44826=CARTESIAN_POINT('Ctrl Pts',(68.9290928531176,358.056267446094,50.2154057454868));
#44827=CARTESIAN_POINT('Ctrl Pts',(74.0832585954538,357.419799417435,46.4072421284185));
#44828=CARTESIAN_POINT('Ctrl Pts',(80.0593463127588,356.78333138878,48.6867769567317));
#44829=CARTESIAN_POINT('Ctrl Pts',(81.3825865019895,356.146863360122,54.9444873079725));
#44830=CARTESIAN_POINT('Ctrl Pts',(76.8197874993998,355.510395331466,59.4443095151045));
#44831=CARTESIAN_POINT('Ctrl Pts',(71.6277284938853,354.980005307585,58.2650326962652));
#44832=CARTESIAN_POINT('Ctrl Pts',(69.4763532374749,354.55569328848,55.0335481469374));
#44833=CARTESIAN_POINT('Ctrl Pts',(69.0414601665085,354.131381269376,51.175857658671));
#44834=CARTESIAN_POINT('Ctrl Pts',(72.2544222487035,353.600991245494,46.9302663935378));
#44835=CARTESIAN_POINT('Ctrl Pts',(78.6429226653259,352.964523216838,47.4348425133144));
#44836=CARTESIAN_POINT('Ctrl Pts',(81.6600989705247,352.32805518818,53.0745721683392));
#44837=CARTESIAN_POINT('Ctrl Pts',(78.5557872721241,351.691587159524,58.6668125349179));
#44838=CARTESIAN_POINT('Ctrl Pts',(72.1602274420798,351.055119130866,59.0722124537102));
#44839=CARTESIAN_POINT('Ctrl Pts',(69.0135210149437,350.524729106987,54.7772841430609));
#44840=CARTESIAN_POINT('Ctrl Pts',(69.5082125339175,350.100417087881,50.9268051874641));
#44841=CARTESIAN_POINT('Ctrl Pts',(71.7094642650518,349.676105068777,47.7290874540463));
#44842=CARTESIAN_POINT('Ctrl Pts',(76.9191944454673,349.145715044897,46.6305056503264));
#44843=CARTESIAN_POINT('Ctrl Pts',(81.4116310180472,348.509247016239,51.2005765770387));
#44844=CARTESIAN_POINT('Ctrl Pts',(79.9914637878894,347.872778987582,57.437004118252));
#44845=CARTESIAN_POINT('Ctrl Pts',(73.9807291221626,347.236310958925,59.6235475586274));
#44846=CARTESIAN_POINT('Ctrl Pts',(68.8862661323819,346.599842930268,55.7358771148282));
#44847=CARTESIAN_POINT('Ctrl Pts',(69.326814842086,346.069452906387,50.4298345813976));
#44848=CARTESIAN_POINT('Ctrl Pts',(72.2251717124735,345.645140887283,47.8471159869094));
#44849=CARTESIAN_POINT('Ctrl Pts',(75.9839434185608,345.220828868178,46.8762693728891));
#44850=CARTESIAN_POINT('Ctrl Pts',(80.6376467415555,344.690438844298,49.4630078431919));
#44851=CARTESIAN_POINT('Ctrl Pts',(81.0327021227699,344.05397081564,55.8592149911513));
#44852=CARTESIAN_POINT('Ctrl Pts',(75.8710807057947,343.417502786984,59.6364584021908));
#44853=CARTESIAN_POINT('Ctrl Pts',(69.8992144031925,342.781034758326,57.3458872283867));
#44854=CARTESIAN_POINT('Ctrl Pts',(68.6021616848208,342.14456672967,51.0701252125357));
#44855=CARTESIAN_POINT('Ctrl Pts',(72.4140943662755,341.614176705789,47.3529569671835));
#44856=CARTESIAN_POINT('Ctrl Pts',(76.2959066074933,341.189864686684,47.3035443132344));
#44857=CARTESIAN_POINT('Ctrl Pts',(79.7703805516423,340.765552667579,49.0352887221662));
#44858=CARTESIAN_POINT('Ctrl Pts',(81.5877181212305,340.2351626437,54.0398321269494));
#44859=CARTESIAN_POINT('Ctrl Pts',(77.6918131141847,339.598694615041,59.1280006392838));
#44860=CARTESIAN_POINT('Ctrl Pts',(71.3179589210744,338.962226586385,58.5951909515068));
#44861=CARTESIAN_POINT('Ctrl Pts',(68.3112066114293,338.325758557728,52.9498969833543));
#44862=CARTESIAN_POINT('Ctrl Pts',(71.4471267602236,337.689290529071,47.3611995095039));
#44863=CARTESIAN_POINT('Ctrl Pts',(76.762576521389,337.158900505191,47.0543373764116));
#44864=CARTESIAN_POINT('Ctrl Pts',(79.7257358927106,336.734588486085,49.5624431211091));
#44865=CARTESIAN_POINT('Ctrl Pts',(81.2134017239108,336.310276466981,53.1482147620699));
#44866=CARTESIAN_POINT('Ctrl Pts',(79.3038686541036,335.7798864431,58.1183107357417));
#44867=CARTESIAN_POINT('Ctrl Pts',(73.0260170282693,335.143418414444,59.4052115080782));
#44868=CARTESIAN_POINT('Ctrl Pts',(68.5631518514559,334.506950385786,54.8234282469443));
#44869=CARTESIAN_POINT('Ctrl Pts',(69.9948378458387,333.87048235713,48.5896349674149));
#44870=CARTESIAN_POINT('Ctrl Pts',(76.0271136359725,333.234014328472,46.4264929411948));
#44871=CARTESIAN_POINT('Ctrl Pts',(80.2414823753424,332.703624304592,49.6803009657747));
#44872=CARTESIAN_POINT('Ctrl Pts',(80.8340253328005,332.279312285487,53.5169402151704));
#44873=CARTESIAN_POINT('Ctrl Pts',(79.605919036016,331.855000266382,57.199692285326));
#44874=CARTESIAN_POINT('Ctrl Pts',(74.9051964886825,331.324610242502,59.6999678831728));
#44875=CARTESIAN_POINT('Ctrl Pts',(69.3215782779007,330.688142213844,56.5550128262509));
#44876=CARTESIAN_POINT('Ctrl Pts',(68.9565293265754,330.051674185188,50.1693536823915));
#44877=CARTESIAN_POINT('Ctrl Pts',(74.1251200219098,329.415206156531,46.4016523058858));
#44878=CARTESIAN_POINT('Ctrl Pts',(80.0979048596417,328.778738127874,48.7240166003043));
#44879=CARTESIAN_POINT('Ctrl Pts',(81.1461299182097,328.248348103993,53.9441118828436));
#44880=CARTESIAN_POINT('Ctrl Pts',(79.0777073227094,327.824036084888,57.2293113977682));
#44881=CARTESIAN_POINT('Ctrl Pts',(75.7356073875843,327.399724065784,59.2044761782546));
#44882=CARTESIAN_POINT('Ctrl Pts',(70.5470739238278,326.869334041903,58.0097833191163));
#44883=CARTESIAN_POINT('Ctrl Pts',(68.3936911683374,326.232866013246,51.97401681086));
#44884=CARTESIAN_POINT('Ctrl Pts',(72.3053343322745,325.596397984589,46.9134880641335));
#44885=CARTESIAN_POINT('Ctrl Pts',(78.6781933351392,324.959929955932,47.4580719126135));
#44886=CARTESIAN_POINT('Ctrl Pts',(81.6647915036336,324.323461927275,53.1279719129468));
#44887=CARTESIAN_POINT('Ctrl Pts',(79.0332371365105,323.793071903394,57.7564805437124));
#44888=CARTESIAN_POINT('Ctrl Pts',(75.3173868460731,323.36875988429,58.8804754304867));
#44889=CARTESIAN_POINT('Ctrl Pts',(71.4989396689043,322.944447865185,58.1802118789516));
#44890=CARTESIAN_POINT('Ctrl Pts',(68.3650037426683,322.414057841304,53.8759562937844));
#44891=CARTESIAN_POINT('Ctrl Pts',(70.6970252219288,321.777589812648,47.9069353980174));
#44892=CARTESIAN_POINT('Ctrl Pts',(76.9686349527099,321.14112178399,46.6512225235155));
#44893=CARTESIAN_POINT('Ctrl Pts',(81.423028119083,320.504653755334,51.2412426713785));
#44894=CARTESIAN_POINT('Ctrl Pts',(79.9599909415306,319.868185726676,57.4803978105727));
#44895=CARTESIAN_POINT('Ctrl Pts',(74.9381325114026,319.337795702796,59.2493264241543));
#44896=CARTESIAN_POINT('Ctrl Pts',(71.3956405454282,318.913483683691,57.6613533269502));
#44897=CARTESIAN_POINT('Ctrl Pts',(68.9719051551272,318.489171664587,54.6287942353181));
#44898=CARTESIAN_POINT('Ctrl Pts',(69.4282117128379,317.958781640705,49.3240836063029));
#44899=CARTESIAN_POINT('Ctrl Pts',(75.1029347411933,317.322313612049,46.3466596886709));
#44900=CARTESIAN_POINT('Ctrl Pts',(80.6613895661029,316.685845583392,49.511068543079));
#44901=CARTESIAN_POINT('Ctrl Pts',(81.014641016088,316.049377554735,55.8973911822435));
#44902=CARTESIAN_POINT('Ctrl Pts',(75.8188643388059,315.412909526078,59.6485829067018));
#44903=CARTESIAN_POINT('Ctrl Pts',(70.8674386639765,314.882519502197,57.6911472579929));
#44904=CARTESIAN_POINT('Ctrl Pts',(69.2341445588646,314.458207483093,54.1693212752611));
#44905=CARTESIAN_POINT('Ctrl Pts',(69.3927639357589,314.033895463987,50.2904364123513));
#44906=CARTESIAN_POINT('Ctrl Pts',(73.2157203846311,313.503505440107,46.5846066102391));
#44907=CARTESIAN_POINT('Ctrl Pts',(79.452501086146,312.86703741145,48.0577329167871));
#44908=CARTESIAN_POINT('Ctrl Pts',(81.5741291552425,312.230569382793,54.0916866599676));
#44909=CARTESIAN_POINT('Ctrl Pts',(77.6531438362427,311.594101354136,59.1449803944151));
#44910=CARTESIAN_POINT('Ctrl Pts',(71.2705853255733,310.95763332548,58.5701051977721));
#44911=CARTESIAN_POINT('Ctrl Pts',(68.8158168069635,310.427243301598,53.8454589621013));
#44912=CARTESIAN_POINT('Ctrl Pts',(69.8920431913756,310.002931282494,50.1154931906856));
#44913=CARTESIAN_POINT('Ctrl Pts',(72.5552930136327,309.578619263389,47.2909563665877));
#44914=CARTESIAN_POINT('Ctrl Pts',(77.8716307581055,309.048229239508,46.9998833192451));
#44915=CARTESIAN_POINT('Ctrl Pts',(81.6144140660285,308.411761210852,52.2017202778367));
#44916=CARTESIAN_POINT('Ctrl Pts',(79.2596065617769,307.775293182194,58.1485501103052));
#44917=CARTESIAN_POINT('Ctrl Pts',(72.985687726908,307.138825153538,59.39267465869));
#44918=CARTESIAN_POINT('Ctrl Pts',(68.5438343362777,306.50235712488,54.7734243851087));
#44919=CARTESIAN_POINT('Ctrl Pts',(69.7885723489147,305.971967101,49.5966688556199));
#44920=CARTESIAN_POINT('Ctrl Pts',(73.0469626822795,305.547655081895,47.4862659742077));
#44921=CARTESIAN_POINT('Ctrl Pts',(76.909836648915,305.123343062791,47.1001149618732));
#44922=CARTESIAN_POINT('Ctrl Pts',(81.1145224710317,304.59295303891,50.3664259803601));
#44923=CARTESIAN_POINT('Ctrl Pts',(80.5293250469464,303.956485010253,56.7480463552083));
#44924=CARTESIAN_POINT('Ctrl Pts',(74.8519499260711,303.320016981596,59.6937746480561));
#44925=CARTESIAN_POINT('Ctrl Pts',(69.2993505210926,302.683548952939,56.5191024939194));
#44926=CARTESIAN_POINT('Ctrl Pts',(68.9747335748927,302.047080924282,50.1189338655102));
#44927=CARTESIAN_POINT('Ctrl Pts',(73.3090500016354,301.516690900401,47.0267062469374));
#44928=CARTESIAN_POINT('Ctrl Pts',(77.1529760290398,301.092378881297,47.569974672562));
#44929=CARTESIAN_POINT('Ctrl Pts',(80.3226457526307,300.668066862192,49.8114254817008));
#44930=CARTESIAN_POINT('Ctrl Pts',(81.355361673332,300.137676838312,55.0346111340902));
#44931=CARTESIAN_POINT('Ctrl Pts',(76.728933306676,299.501208809654,59.4689876632131));
#44932=CARTESIAN_POINT('Ctrl Pts',(70.5109339842768,298.864740780998,57.9701921918225));
#44933=CARTESIAN_POINT('Ctrl Pts',(68.40045667283,298.22827275234,51.9323292456896));
#44934=CARTESIAN_POINT('Ctrl Pts',(72.3521401674818,297.591804723684,46.8873582654032));
#44935=CARTESIAN_POINT('Ctrl Pts',(77.6521973570184,297.061414699802,47.3948662159206));
#44936=CARTESIAN_POINT('Ctrl Pts',(80.1981152800705,296.637102680698,50.3256015870383));
#44937=CARTESIAN_POINT('Ctrl Pts',(81.1214260671454,296.212790661593,54.0963316326538));
#44938=CARTESIAN_POINT('Ctrl Pts',(78.4761358999726,295.682400637713,58.717003711871));
#44939=CARTESIAN_POINT('Ctrl Pts',(72.0754506158946,295.045932609055,59.0312687720055));
#44940=CARTESIAN_POINT('Ctrl Pts',(68.3636791850171,294.409464580399,53.8223671331437));
#44941=CARTESIAN_POINT('Ctrl Pts',(70.7294688552404,293.772996551742,47.8798977243302));
#44942=CARTESIAN_POINT('Ctrl Pts',(77.0211072714768,293.136528523085,46.6621864805733));
#44943=CARTESIAN_POINT('Ctrl Pts',(80.6898495626673,292.606138499204,50.5207484579202));
#44944=CARTESIAN_POINT('Ctrl Pts',(80.6902463228452,292.181826480099,54.4028751597447));
#44945=CARTESIAN_POINT('Ctrl Pts',(78.9147710729384,291.757514460995,57.8552070562179));
#44946=CARTESIAN_POINT('Ctrl Pts',(73.8876807942301,291.227124437114,59.6092121479762));
#44947=CARTESIAN_POINT('Ctrl Pts',(68.849107759653,290.590656408457,55.6493742208554));
#44948=CARTESIAN_POINT('Ctrl Pts',(69.4623515772426,289.9541883798,49.2827553804812));
#44949=CARTESIAN_POINT('Ctrl Pts',(75.145158953817,289.317720351143,46.3475205075674));
#44950=CARTESIAN_POINT('Ctrl Pts',(80.6938166586057,288.681252322486,49.5537538597928));
#44951=CARTESIAN_POINT('Ctrl Pts',(80.9335411973356,288.150862298606,54.8726543737833));
#44952=CARTESIAN_POINT('Ctrl Pts',(78.3882223800832,287.726550279501,57.8039100782516));
#44953=CARTESIAN_POINT('Ctrl Pts',(74.7839532242394,287.302238260396,59.246183193397));
#44954=CARTESIAN_POINT('Ctrl Pts',(69.8383632853863,286.771848236515,57.2740496561053));
#44955=CARTESIAN_POINT('Ctrl Pts',(68.6308295619551,286.135380207858,50.9804499754289));
#44956=CARTESIAN_POINT('Ctrl Pts',(73.268595959504,285.498912179202,46.5757903654038));
#44957=CARTESIAN_POINT('Ctrl Pts',(79.4838157937093,284.862444150545,48.086070422519));
#44958=CARTESIAN_POINT('Ctrl Pts',(81.5706215770567,284.225976121887,54.1451773085559));
#44959=CARTESIAN_POINT('Ctrl Pts',(78.2638620892544,283.695586098007,58.3181273708052));
#44960=CARTESIAN_POINT('Ctrl Pts',(74.4200471881275,283.271274078902,58.8621814970761));
#44961=CARTESIAN_POINT('Ctrl Pts',(70.7530948079326,282.846962059797,57.5876744834349));
#44962=CARTESIAN_POINT('Ctrl Pts',(68.3123700687952,282.316572035917,52.8557580344726));
#44963=CARTESIAN_POINT('Ctrl Pts',(71.5275734779309,281.68010400726,47.3122932630761));
#44964=CARTESIAN_POINT('Ctrl Pts',(77.9173327360281,281.043635978603,47.0278990613398));
#44965=CARTESIAN_POINT('Ctrl Pts',(81.6194748985279,280.407167949946,52.2436489448233));
#44966=CARTESIAN_POINT('Ctrl Pts',(79.221883044505,279.770699921289,58.1866353940218));
#44967=CARTESIAN_POINT('Ctrl Pts',(73.9889689229884,279.240309897408,59.1688677132986));
#44968=CARTESIAN_POINT('Ctrl Pts',(70.7301472839238,278.815997878304,57.0591309024144));
#44969=CARTESIAN_POINT('Ctrl Pts',(68.7973374677702,278.391685859198,53.6923588428567));
#44970=CARTESIAN_POINT('Ctrl Pts',(70.0574457782005,277.861295835319,48.5193232177926));
#44971=CARTESIAN_POINT('Ctrl Pts',(76.1199198830696,277.224827806661,46.4423200012274));
#44972=CARTESIAN_POINT('Ctrl Pts',(81.1306566444992,276.588359778005,50.4175458496641));
#44973=CARTESIAN_POINT('Ctrl Pts',(80.5056521700667,275.951891749347,56.7830209179806));
#44974=CARTESIAN_POINT('Ctrl Pts',(74.7984951898932,275.315423720691,59.6977925792757));
#44975=CARTESIAN_POINT('Ctrl Pts',(70.2035816423413,274.78503369681,57.008008197077));
#44976=CARTESIAN_POINT('Ctrl Pts',(69.1265928622935,274.360721677705,53.2782624880387));
#44977=CARTESIAN_POINT('Ctrl Pts',(69.8750124991416,273.936409658601,49.4689612484914));
#44978=CARTESIAN_POINT('Ctrl Pts',(74.2184942159277,273.406019634719,46.389620879493));
#44979=CARTESIAN_POINT('Ctrl Pts',(80.1575950910935,272.769551606063,48.796821624848));
#44980=CARTESIAN_POINT('Ctrl Pts',(81.3340222132102,272.133083577406,55.0837861280693));
#44981=CARTESIAN_POINT('Ctrl Pts',(76.6881265535354,271.496615548749,59.4798704036303));
#44982=CARTESIAN_POINT('Ctrl Pts',(70.4679411286712,270.860147520092,57.9381739632954));
#44983=CARTESIAN_POINT('Ctrl Pts',(68.7625597545307,270.329757496211,52.8943812533468));
#44984=CARTESIAN_POINT('Ctrl Pts',(70.3951339519087,269.905445477106,49.3722214931296));
#44985=CARTESIAN_POINT('Ctrl Pts',(73.4580535169106,269.481133458002,46.9869685453763));
#44986=CARTESIAN_POINT('Ctrl Pts',(78.7565799488251,268.950743434121,47.5102162711232));
#44987=CARTESIAN_POINT('Ctrl Pts',(81.6621171947612,268.314275405464,53.2220800603177));
#44988=CARTESIAN_POINT('Ctrl Pts',(78.4277792530005,267.677807376808,58.7401378270421));
#44989=CARTESIAN_POINT('Ctrl Pts',(72.0375055083273,267.04133934815,59.0127270905129));
#44990=CARTESIAN_POINT('Ctrl Pts',(68.3522149334259,266.404871319494,53.7700018438139));
#44991=CARTESIAN_POINT('Ctrl Pts',(70.3720114990969,265.874481295612,48.8436855359119));
#44992=CARTESIAN_POINT('Ctrl Pts',(73.9141788037828,265.450169276508,47.2549883740677));
#44993=CARTESIAN_POINT('Ctrl Pts',(77.7907517378467,265.025857257403,47.4625701009125));
#44994=CARTESIAN_POINT('Ctrl Pts',(81.4480173029673,264.495467233522,51.3320118072031));
#44995=CARTESIAN_POINT('Ctrl Pts',(79.8962625176273,263.858999204865,57.5496955978126));
#44996=CARTESIAN_POINT('Ctrl Pts',(73.83600196959,263.222531176209,59.5949695472677));
#44997=CARTESIAN_POINT('Ctrl Pts',(68.8326175982397,262.586063147551,55.6104936380737));
#44998=CARTESIAN_POINT('Ctrl Pts',(69.4880334727284,261.949595118895,49.2357022951904));
#44999=CARTESIAN_POINT('Ctrl Pts',(74.2432971283764,261.419205095013,46.8407830695233));
#45000=CARTESIAN_POINT('Ctrl Pts',(77.959377089695,260.994893075909,47.9640183999525));
#45001=CARTESIAN_POINT('Ctrl Pts',(80.7500624399219,260.570581056804,50.6627186727628));
#45002=CARTESIAN_POINT('Ctrl Pts',(80.973987939756,260.040191032924,55.982307745494));
#45003=CARTESIAN_POINT('Ctrl Pts',(75.7253090599096,259.403723004267,59.6591140566951));
#45004=CARTESIAN_POINT('Ctrl Pts',(69.8086851766418,258.76725497561,57.2294092881355));
#45005=CARTESIAN_POINT('Ctrl Pts',(68.64387461178,258.130786946953,50.9402821796723));
#45006=CARTESIAN_POINT('Ctrl Pts',(73.3188397393547,257.494318918296,46.5571057413125));
#45007=CARTESIAN_POINT('Ctrl Pts',(78.4794664963865,256.963928894415,47.8671065072692));
#45008=CARTESIAN_POINT('Ctrl Pts',(80.5485605550081,256.539616875311,51.1518831607137));
#45009=CARTESIAN_POINT('Ctrl Pts',(80.8859079471689,256.115304856205,55.0193247728702));
#45010=CARTESIAN_POINT('Ctrl Pts',(77.5667687190911,255.584914832326,59.1824348262834));
#45011=CARTESIAN_POINT('Ctrl Pts',(71.193045766207,254.948446803668,58.5167093921053));
#45012=CARTESIAN_POINT('Ctrl Pts',(68.3192351039939,254.311978775012,52.8025939123332));
#45013=CARTESIAN_POINT('Ctrl Pts',(71.5637615965536,253.675510746354,47.2905206837289));
#45014=CARTESIAN_POINT('Ctrl Pts',(77.9675186861103,253.039042717698,47.0467384616874));
#45015=CARTESIAN_POINT('Ctrl Pts',(81.0047745224026,252.508652693817,51.4197520126738));
#45016=CARTESIAN_POINT('Ctrl Pts',(80.4130157998748,252.084340674712,55.2565122997844));
#45017=CARTESIAN_POINT('Ctrl Pts',(78.1317232526417,251.660028655607,58.3976286937398));
#45018=CARTESIAN_POINT('Ctrl Pts',(72.8959148267621,251.129638631727,59.3643140922468));
#45019=CARTESIAN_POINT('Ctrl Pts',(68.5203052848772,250.493170603069,54.6822658470019));
#45020=CARTESIAN_POINT('Ctrl Pts',(70.0974900542959,249.856702574413,48.4836860385676));
#45021=CARTESIAN_POINT('Ctrl Pts',(76.1615187036544,249.220234545756,46.4496113157072));
#45022=CARTESIAN_POINT('Ctrl Pts',(81.1561933875673,248.583766517099,50.4646778700389));
#45023=CARTESIAN_POINT('Ctrl Pts',(80.5818071049249,248.053376493218,55.7579047620688));
#45024=CARTESIAN_POINT('Ctrl Pts',(77.6191604611375,247.629064474113,58.2666161345652));
#45025=CARTESIAN_POINT('Ctrl Pts',(73.8370732189359,247.204752455009,59.1422438972669));
#45026=CARTESIAN_POINT('Ctrl Pts',(69.2501690271641,246.674362431128,56.4388237546138));
#45027=CARTESIAN_POINT('Ctrl Pts',(69.0167443893414,246.037894402471,50.0346807540015));
#45028=CARTESIAN_POINT('Ctrl Pts',(74.2720958288138,245.401426373814,46.3889730468402));
#45029=CARTESIAN_POINT('Ctrl Pts',(80.1842209746279,244.764958345157,48.8296040510377));
#45030=CARTESIAN_POINT('Ctrl Pts',(81.3223966119943,244.1284903165,55.1361158327074));
#45031=CARTESIAN_POINT('Ctrl Pts',(77.4178204841707,243.598100292619,58.7558472860377));
#45032=CARTESIAN_POINT('Ctrl Pts',(73.5359982239256,243.173788273515,58.7072280891914));
#45033=CARTESIAN_POINT('Ctrl Pts',(70.1063587579266,242.74947625441,56.8883050507697));
#45034=CARTESIAN_POINT('Ctrl Pts',(68.415965773611,242.21908623053,51.8394693344116));
#45035=CARTESIAN_POINT('Ctrl Pts',(72.4391053296256,241.582618201872,46.8512950444875));
#45036=CARTESIAN_POINT('Ctrl Pts',(78.7974738286708,240.946150173216,47.5448752264207));
#45037=CARTESIAN_POINT('Ctrl Pts',(81.6607233194671,240.309682144558,53.2642900384335));
#45038=CARTESIAN_POINT('Ctrl Pts',(78.3846879127202,239.673214115902,58.7720233877865));
#45039=CARTESIAN_POINT('Ctrl Pts',(73.0631846035857,239.14282409202,58.9445721144314));
#45040=CARTESIAN_POINT('Ctrl Pts',(70.1642998769843,238.718512072917,56.3624460082323));
#45041=CARTESIAN_POINT('Ctrl Pts',(68.7676494101067,238.294200053811,52.740253942672));
#45042=CARTESIAN_POINT('Ctrl Pts',(70.8020690104725,237.763810029931,47.8199584818442));
#45043=CARTESIAN_POINT('Ctrl Pts',(77.1104133983672,237.127342001273,46.6919843165582));
#45044=CARTESIAN_POINT('Ctrl Pts',(81.4561652353981,236.490873972617,51.3849944816189));
#45045=CARTESIAN_POINT('Ctrl Pts',(79.8675318896678,235.854405943959,57.5806500184647));
#45046=CARTESIAN_POINT('Ctrl Pts',(73.7825598716915,235.217937915303,59.5907868730799));
#45047=CARTESIAN_POINT('Ctrl Pts',(69.6516937528243,234.687547891422,56.2316030971915));
#45048=CARTESIAN_POINT('Ctrl Pts',(69.1562151927476,234.263235872318,52.3812253387187));
#45049=CARTESIAN_POINT('Ctrl Pts',(70.4769197368907,233.838923853213,48.7306572468295));
#45050=CARTESIAN_POINT('Ctrl Pts',(75.2392757088466,233.308533829332,46.3498724752568));
#45051=CARTESIAN_POINT('Ctrl Pts',(80.7417032823629,232.672065800675,49.634811657659));
#45052=CARTESIAN_POINT('Ctrl Pts',(80.9453973953874,232.035597772018,56.027652352275));
#45053=CARTESIAN_POINT('Ctrl Pts',(75.683319836815,231.399129743361,59.6636450923455));
#45054=CARTESIAN_POINT('Ctrl Pts',(69.7710792277636,230.762661714704,57.1912079111794));
#45055=CARTESIAN_POINT('Ctrl Pts',(68.8549962387284,230.232271690823,51.9463092001141));
#45056=CARTESIAN_POINT('Ctrl Pts',(71.0057109233227,229.807959671719,48.71438496963));
#45057=CARTESIAN_POINT('Ctrl Pts',(74.3966183648981,229.383647652614,46.8242382530895));
#45058=CARTESIAN_POINT('Ctrl Pts',(79.5533314475779,228.853257628733,48.1495611239604));
#45059=CARTESIAN_POINT('Ctrl Pts',(81.553624002664,228.216789600076,54.2377763246406));
#45060=CARTESIAN_POINT('Ctrl Pts',(77.5154492131354,227.58032157142,59.1979222716756));
#45061=CARTESIAN_POINT('Ctrl Pts',(71.1583728874286,226.943853542763,58.492596811605));
#45062=CARTESIAN_POINT('Ctrl Pts',(68.3158924128625,226.307385514106,52.7490927066299));
#45063=CARTESIAN_POINT('Ctrl Pts',(71.0634780017905,225.776995490225,48.1885067791575));
#45064=CARTESIAN_POINT('Ctrl Pts',(74.8065245107504,225.35268347112,47.1586958035716));
#45065=CARTESIAN_POINT('Ctrl Pts',(78.6060725394363,224.928371452016,47.955152209226));
#45066=CARTESIAN_POINT('Ctrl Pts',(81.6303263902578,224.397981428135,52.3371676064709));
#45067=CARTESIAN_POINT('Ctrl Pts',(79.1483302191681,223.761513399478,58.2454016254753));
#45068=CARTESIAN_POINT('Ctrl Pts',(72.8470130986032,223.125045370821,59.3423554510688));
#45069=CARTESIAN_POINT('Ctrl Pts',(68.5099388049065,222.488577342164,54.6413249332986));
#45070=CARTESIAN_POINT('Ctrl Pts',(70.1300482334095,221.852109313507,48.4411008882662));
#45071=CARTESIAN_POINT('Ctrl Pts',(75.1949720228243,221.321719289626,46.7995385915325));
#45072=CARTESIAN_POINT('Ctrl Pts',(78.6962367276934,220.897407270522,48.4764536776389));
#45073=CARTESIAN_POINT('Ctrl Pts',(81.0426295882978,220.473095251417,51.5692452983744));
#45074=CARTESIAN_POINT('Ctrl Pts',(80.4525183097322,219.942705227537,56.8607430811448));
#45075=CARTESIAN_POINT('Ctrl Pts',(74.7044349299368,219.306237198879,59.6939299756169));
#45076=CARTESIAN_POINT('Ctrl Pts',(69.2276352050903,218.669769170223,56.3901794069435));
#45077=CARTESIAN_POINT('Ctrl Pts',(69.0357866029293,218.033301141565,49.9969717623945));
#45078=CARTESIAN_POINT('Ctrl Pts',(74.3245562273971,217.396833112908,46.3781728935986));
#45079=CARTESIAN_POINT('Ctrl Pts',(79.2251026994422,216.866443089028,48.4600028300045));
#45080=CARTESIAN_POINT('Ctrl Pts',(80.7687641568812,216.442131069923,52.0219549838932));
#45081=CARTESIAN_POINT('Ctrl Pts',(80.5126174062247,216.017819050818,55.895581808213));
#45082=CARTESIAN_POINT('Ctrl Pts',(76.5965009308421,215.487429026938,59.503735860729));
#45083=CARTESIAN_POINT('Ctrl Pts',(70.4003730145984,214.85096099828,57.873534909508));
#45084=CARTESIAN_POINT('Ctrl Pts',(68.429181621647,214.214492969624,51.7880485052417));
#45085=CARTESIAN_POINT('Ctrl Pts',(72.4813418470979,213.578024940966,46.8351607156745));
#45086=CARTESIAN_POINT('Ctrl Pts',(78.8381545815176,212.94155691231,47.5713888109593));
#45087=CARTESIAN_POINT('Ctrl Pts',(81.6581187360802,212.305088883653,53.3130386131624));
#45088=CARTESIAN_POINT('Ctrl Pts',(78.3435294198688,211.668620854996,58.7960171796599));
#45089=CARTESIAN_POINT('Ctrl Pts',(73.0203157428126,211.138230831115,58.9307022339566));
#45090=CARTESIAN_POINT('Ctrl Pts',(70.1404093382657,210.713918812011,56.3274859477036));
#45091=CARTESIAN_POINT('Ctrl Pts',(68.7697904747173,210.289606792905,52.6954344925807));
#45092=CARTESIAN_POINT('Ctrl Pts',(70.8397506710645,209.759216769025,47.7898625183533));
#45093=CARTESIAN_POINT('Ctrl Pts',(77.1560180005676,209.122748740368,46.7074779213906));
#45094=CARTESIAN_POINT('Ctrl Pts',(81.4678228126991,208.486280711711,51.4316973420522));
#45095=CARTESIAN_POINT('Ctrl Pts',(79.8345150471389,207.849812683054,57.6157420369948));
#45096=CARTESIAN_POINT('Ctrl Pts',(73.7352061577403,207.213344654398,59.5819163913665));
#45097=CARTESIAN_POINT('Ctrl Pts',(69.6286797739237,206.682954630516,56.1930196438724));
#45098=CARTESIAN_POINT('Ctrl Pts',(69.1609966055946,206.258642611412,52.3391654795781));
#45099=CARTESIAN_POINT('Ctrl Pts',(70.5080046768267,205.834330592307,48.6982221958113));
#45100=CARTESIAN_POINT('Ctrl Pts',(75.2874147618561,205.303940568427,46.3518592644304));
#45101=CARTESIAN_POINT('Ctrl Pts',(80.7659978619589,204.667472539769,49.6764133674932));
#45102=CARTESIAN_POINT('Ctrl Pts',(80.9235624218643,204.031004511113,56.0705571543901));
#45103=CARTESIAN_POINT('Ctrl Pts',(75.6353879853842,203.394536482455,59.668489377038));
#45104=CARTESIAN_POINT('Ctrl Pts',(69.7411399911392,202.758068453799,57.153459596108));
#45105=CARTESIAN_POINT('Ctrl Pts',(68.8629228367167,202.227678429917,51.902087877635));
#45106=CARTESIAN_POINT('Ctrl Pts',(71.0368999365241,201.803366410813,48.6857651951434));
#45107=CARTESIAN_POINT('Ctrl Pts',(74.4413565467986,201.379054391709,46.8201331300155));
#45108=CARTESIAN_POINT('Ctrl Pts',(79.5883731887436,200.848664367828,48.1826272613378));
#45109=CARTESIAN_POINT('Ctrl Pts',(81.5446871133722,200.212196339171,54.2851161372355));
#45110=CARTESIAN_POINT('Ctrl Pts',(77.4708299078219,199.575728310514,59.2159974868797));
#45111=CARTESIAN_POINT('Ctrl Pts',(71.1190079787084,198.939260281857,58.4648239866103));
#45112=CARTESIAN_POINT('Ctrl Pts',(68.3180409606457,198.3027922532,52.7009608376928));
#45113=CARTESIAN_POINT('Ctrl Pts',(71.098459721967,197.77240222932,48.1603174867096));
#45114=CARTESIAN_POINT('Ctrl Pts',(74.8488389159196,197.348090210214,47.1575394509773));
#45115=CARTESIAN_POINT('Ctrl Pts',(78.6425415842146,196.92377819111,47.9813889218711));
#45116=CARTESIAN_POINT('Ctrl Pts',(81.6351004541037,196.393388167229,52.3851102961616));
#45117=CARTESIAN_POINT('Ctrl Pts',(79.11054081409,195.756920138572,58.2752828961914));
#45118=CARTESIAN_POINT('Ctrl Pts',(72.8014733044529,195.120452109916,59.3267440686173));
#45119=CARTESIAN_POINT('Ctrl Pts',(68.498429651078,194.483984081258,54.5945438662197));
#45120=CARTESIAN_POINT('Ctrl Pts',(70.1632321105985,193.847516052601,48.4061702992275));
#45121=CARTESIAN_POINT('Ctrl Pts',(75.2398670646046,193.317126028721,46.8011942632874));
#45122=CARTESIAN_POINT('Ctrl Pts',(78.7289430044913,192.892814009616,48.5033273286335));
#45123=CARTESIAN_POINT('Ctrl Pts',(81.0529576331648,192.468501990511,51.6129678049825));
#45124=CARTESIAN_POINT('Ctrl Pts',(80.4246892842127,191.938111966631,56.9000699804562));
#45125=CARTESIAN_POINT('Ctrl Pts',(74.65630346539,191.301643937974,59.6917110173807));
#45126=CARTESIAN_POINT('Ctrl Pts',(69.2035016326957,190.665175909317,56.3485305538422));
#45127=CARTESIAN_POINT('Ctrl Pts',(69.0577500836245,190.02870788066,49.9541064261852));
#45128=CARTESIAN_POINT('Ctrl Pts',(74.3725601345045,189.392239852003,46.3735577591653));
#45129=CARTESIAN_POINT('Ctrl Pts',(79.2578336803251,188.861849828122,48.4906956655628));
#45130=CARTESIAN_POINT('Ctrl Pts',(80.7759409611788,188.437537809017,52.0636857537459));
#45131=CARTESIAN_POINT('Ctrl Pts',(80.4914882630651,188.013225789913,55.9353771863079));
#45132=CARTESIAN_POINT('Ctrl Pts',(76.5502474625308,187.482835766032,59.515152526242));
#45133=CARTESIAN_POINT('Ctrl Pts',(70.3645745965685,186.846367737375,57.8403433343832));
#45134=CARTESIAN_POINT('Ctrl Pts',(68.4399397736334,186.209899708718,51.7406970957261));
#45135=CARTESIAN_POINT('Ctrl Pts',(72.5228993479575,185.573431680061,46.8173502104404));
#45136=CARTESIAN_POINT('Ctrl Pts',(78.8834323500699,184.936963651404,47.5991139617571));
#45137=CARTESIAN_POINT('Ctrl Pts',(81.1835349749613,184.406573627523,52.4009571960959));
#45138=CARTESIAN_POINT('Ctrl Pts',(79.9867931126735,183.982261608419,56.094020531795));
#45139=CARTESIAN_POINT('Ctrl Pts',(77.2332563931867,183.557949589314,58.8306139288627));
#45140=CARTESIAN_POINT('Ctrl Pts',(71.9102716857639,183.027559565433,58.9489538491949));
#45141=CARTESIAN_POINT('Ctrl Pts',(68.3383237334809,182.391091536777,53.6283596662101));
#45142=CARTESIAN_POINT('Ctrl Pts',(70.8849370199572,181.754623508119,47.761106117269));
#45143=CARTESIAN_POINT('Ctrl Pts',(77.1959362348037,181.118155479463,46.7213021219764));
#45144=CARTESIAN_POINT('Ctrl Pts',(81.4854978487712,180.481687450805,51.482309976812));
#45145=CARTESIAN_POINT('Ctrl Pts',(80.073367272166,179.951297426925,56.6159303140414));
#45146=CARTESIAN_POINT('Ctrl Pts',(76.7481860199208,179.52698540782,58.6194466045056));
#45147=CARTESIAN_POINT('Ctrl Pts',(72.8748126305075,179.102673388715,58.8799969309715));
#45148=CARTESIAN_POINT('Ctrl Pts',(68.7783742806616,178.572283364835,55.4789142536309));
#45149=CARTESIAN_POINT('Ctrl Pts',(69.5704243653522,177.935815336178,49.1196539745438));
#45150=CARTESIAN_POINT('Ctrl Pts',(75.340431971015,177.299347307521,46.3597779503322));
#45151=CARTESIAN_POINT('Ctrl Pts',(80.7870483010708,176.662879278864,49.7130262250032));
#45152=CARTESIAN_POINT('Ctrl Pts',(80.9037309672252,176.026411250207,56.1203595072083));
#45153=CARTESIAN_POINT('Ctrl Pts',(76.4713185355127,175.496021226327,59.0702562117385));
#45154=CARTESIAN_POINT('Ctrl Pts',(72.6470540467699,175.071709207221,58.4024920268817));
#45155=CARTESIAN_POINT('Ctrl Pts',(69.551817146766,174.647397188117,56.0593282640832));
#45156=CARTESIAN_POINT('Ctrl Pts',(68.6892013076634,174.117007164236,50.8053712366301));
#45157=CARTESIAN_POINT('Ctrl Pts',(73.4571407575176,173.480539135579,46.5235155598984));
#45158=CARTESIAN_POINT('Ctrl Pts',(79.6232088666685,172.844071106923,48.2233707042361));
#45159=CARTESIAN_POINT('Ctrl Pts',(81.5365719076763,172.207603078265,54.3265621080611));
#45160=CARTESIAN_POINT('Ctrl Pts',(77.4232005111353,171.571135049609,59.2405940969629));
#45161=CARTESIAN_POINT('Ctrl Pts',(72.1424114296051,171.040745025728,58.5613024007155));
#45162=CARTESIAN_POINT('Ctrl Pts',(69.692973246283,170.616433006623,55.5494656733147));
#45163=CARTESIAN_POINT('Ctrl Pts',(68.8925550574566,170.192120987518,51.7507502839452));
#45164=CARTESIAN_POINT('Ctrl Pts',(71.6864479885501,169.661730963638,47.2183852476993));
#45165=CARTESIAN_POINT('Ctrl Pts',(78.0939616097122,169.025262934981,47.1120657835623));
#45166=CARTESIAN_POINT('Ctrl Pts',(81.6346846946041,168.388794906324,52.43871421147));
#45167=CARTESIAN_POINT('Ctrl Pts',(79.0772365788344,167.752326877667,58.301253130195));
#45168=CARTESIAN_POINT('Ctrl Pts',(72.7493845539464,167.11585884901,59.3140825259745));
#45169=CARTESIAN_POINT('Ctrl Pts',(69.207833010338,166.585468825129,55.3384589024206));
#45170=CARTESIAN_POINT('Ctrl Pts',(69.3334586153764,166.161156806024,51.4583653347606));
#45171=CARTESIAN_POINT('Ctrl Pts',(71.2200682242025,165.73684478692,48.0654886688141));
#45172=CARTESIAN_POINT('Ctrl Pts',(76.3014478199115,165.206454763039,46.4755981265107));
#45173=CARTESIAN_POINT('Ctrl Pts',(81.20882052468,164.569986734382,50.5969119668202));
#45174=CARTESIAN_POINT('Ctrl Pts',(80.3892258098679,163.933518705725,56.940268171691));
#45175=CARTESIAN_POINT('Ctrl Pts',(74.6141294504006,163.297050677068,59.6894799636937));
#45176=CARTESIAN_POINT('Ctrl Pts',(69.1724772872813,162.660582648411,56.3048150808067));
#45177=CARTESIAN_POINT('Ctrl Pts',(69.1055420061302,162.13019262453,50.980935837216));
#45178=CARTESIAN_POINT('Ctrl Pts',(71.7446741979597,161.705880605426,48.1338515110173));
#45179=CARTESIAN_POINT('Ctrl Pts',(75.3938630579889,161.281568586321,46.8093408276792));
#45180=CARTESIAN_POINT('Ctrl Pts',(80.27282681849,160.751178562441,48.9409794358665));
#45181=CARTESIAN_POINT('Ctrl Pts',(81.2754203909972,160.114710533783,55.2704613074101));
#45182=CARTESIAN_POINT('Ctrl Pts',(76.4971135606888,159.478242505127,59.5222476700871));
#45183=CARTESIAN_POINT('Ctrl Pts',(70.334196289122,158.841774476469,57.8110042209413));
#45184=CARTESIAN_POINT('Ctrl Pts',(68.4451819243434,158.205306447813,51.6873485020516));
#45185=CARTESIAN_POINT('Ctrl Pts',(71.8856615424623,157.674916423932,47.6239422302756));
#45186=CARTESIAN_POINT('Ctrl Pts',(75.7451117847744,157.250604404827,47.2049533120979));
#45187=CARTESIAN_POINT('Ctrl Pts',(79.3687583251269,156.826292385722,48.5978257531446));
#45188=CARTESIAN_POINT('Ctrl Pts',(81.6545885653878,156.295902361842,53.4064794779313));
#45189=CARTESIAN_POINT('Ctrl Pts',(78.2611269268695,155.659434333185,58.8426502572334));
#45190=CARTESIAN_POINT('Ctrl Pts',(71.8655032454052,155.022966304528,58.9194692881673));
#45191=CARTESIAN_POINT('Ctrl Pts',(68.33462666264,154.386498275871,53.5862888115946));
#45192=CARTESIAN_POINT('Ctrl Pts',(70.9238769856076,153.750030247214,47.7242654920534));
#45193=CARTESIAN_POINT('Ctrl Pts',(76.1859185490112,153.219640223333,46.9124224547526));
#45194=CARTESIAN_POINT('Ctrl Pts',(79.3745360971544,152.795328204228,49.1268356994087));
#45195=CARTESIAN_POINT('Ctrl Pts',(81.1970346167882,152.371016185124,52.5545765052998));
#45196=CARTESIAN_POINT('Ctrl Pts',(79.7696625991367,151.840626161243,57.6839799458007));
#45197=CARTESIAN_POINT('Ctrl Pts',(73.642959648389,151.204158132586,59.5630876029432));
#45198=CARTESIAN_POINT('Ctrl Pts',(68.7639080710162,150.567690103929,55.4272975763874));
#45199=CARTESIAN_POINT('Ctrl Pts',(69.5952201151085,149.931222075272,49.0854663169038));
#45200=CARTESIAN_POINT('Ctrl Pts',(75.3939889653761,149.294754046615,46.3574973920444));
#45201=CARTESIAN_POINT('Ctrl Pts',(79.8991646679696,148.764364022735,49.1950249110227));
#45202=CARTESIAN_POINT('Ctrl Pts',(80.8545102956352,148.34005200363,52.957766281106));
#45203=CARTESIAN_POINT('Ctrl Pts',(79.9828270161261,147.915739984525,56.740764582277));
#45204=CARTESIAN_POINT('Ctrl Pts',(75.5416724725442,147.385349960645,59.6774833042897));
#45205=CARTESIAN_POINT('Ctrl Pts',(69.6838446044191,146.748881931988,57.0787552882691));
#45206=CARTESIAN_POINT('Ctrl Pts',(68.712125846895,146.112413903331,50.7569148841861));
#45207=CARTESIAN_POINT('Ctrl Pts',(73.4982792811873,145.475945874674,46.5139632297563));
#45208=CARTESIAN_POINT('Ctrl Pts',(79.6651396832196,144.839477846017,48.2567676983297));
#45209=CARTESIAN_POINT('Ctrl Pts',(81.2058899375428,144.309087822136,53.3532624924015));
#45210=CARTESIAN_POINT('Ctrl Pts',(79.4598393053229,143.884775803031,56.8205690949624));
#45211=CARTESIAN_POINT('Ctrl Pts',(76.3211035792066,143.460463783927,59.1051359965959));
#45212=CARTESIAN_POINT('Ctrl Pts',(71.0423553953876,142.930073760046,58.4101625121945));
#45213=CARTESIAN_POINT('Ctrl Pts',(68.3237688121462,142.293605731389,52.6069891024768));
#45214=CARTESIAN_POINT('Ctrl Pts',(71.7355301328902,141.657137702732,47.1968330854384));
#45215=CARTESIAN_POINT('Ctrl Pts',(78.131284816172,141.020669674075,47.1318294725001));
#45216=CARTESIAN_POINT('Ctrl Pts',(81.6444430145778,140.384201645418,52.4914240566834));
#45217=CARTESIAN_POINT('Ctrl Pts',(79.4657921614448,139.853811621537,57.3495771000057));
#45218=CARTESIAN_POINT('Ctrl Pts',(75.8739191842768,139.429499602433,58.8224506187867));
#45219=CARTESIAN_POINT('Ctrl Pts',(72.0061278849508,139.005187583328,58.4891364257266));
#45220=CARTESIAN_POINT('Ctrl Pts',(68.476400198112,138.474797559447,54.5030113663535));
#45221=CARTESIAN_POINT('Ctrl Pts',(70.2291765021866,137.83832953079,48.3389777955731));
#45222=CARTESIAN_POINT('Ctrl Pts',(76.3526370626844,137.201861502133,46.4915108263287));
#45223=CARTESIAN_POINT('Ctrl Pts',(81.2240398481348,136.565393473476,50.6363073641968));
#45224=CARTESIAN_POINT('Ctrl Pts',(80.3620300055901,135.928925444819,56.9864627690029));
#45225=CARTESIAN_POINT('Ctrl Pts',(75.5315283240709,135.398535420939,59.2257537364833));
#45226=CARTESIAN_POINT('Ctrl Pts',(71.853869491347,134.974223401834,57.9824784666719));
#45227=CARTESIAN_POINT('Ctrl Pts',(69.1522605248948,134.549911382729,55.1946088716546));
#45228=CARTESIAN_POINT('Ctrl Pts',(69.1011383080979,134.019521358849,49.8705543028932));
#45229=CARTESIAN_POINT('Ctrl Pts',(74.4664079702696,133.383053330192,46.3660691643869));
#45230=CARTESIAN_POINT('Ctrl Pts',(80.3010401637996,132.746585301535,48.9865596918726));
#45231=CARTESIAN_POINT('Ctrl Pts',(81.2610782835899,132.110117272878,55.3101844630753));
#45232=CARTESIAN_POINT('Ctrl Pts',(76.4462897180739,131.473649244221,59.5392914259234));
#45233=CARTESIAN_POINT('Ctrl Pts',(71.3309082217835,130.94325922034,58.0624560662408));
#45234=CARTESIAN_POINT('Ctrl Pts',(69.3695355394668,130.518947201236,54.7122433733663));
#45235=CARTESIAN_POINT('Ctrl Pts',(69.1579113875603,130.094635182131,50.8358890158844));
#45236=CARTESIAN_POINT('Ctrl Pts',(72.6104447936233,129.56424515825,46.7827194398347));
#45237=CARTESIAN_POINT('Ctrl Pts',(78.9591977010965,128.927777129593,47.6549987263476));
#45238=CARTESIAN_POINT('Ctrl Pts',(81.6460013269083,128.291309100936,53.4593927269945));
#45239=CARTESIAN_POINT('Ctrl Pts',(78.2242510960193,127.654841072279,58.8632366177664));
#45240=CARTESIAN_POINT('Ctrl Pts',(71.8159553123667,127.018373043623,58.8990106732897));
#45241=CARTESIAN_POINT('Ctrl Pts',(68.9222576097237,126.487983019741,54.4297060139589));
#45242=CARTESIAN_POINT('Ctrl Pts',(69.6382539201413,126.063671000637,50.6141775879205));
#45243=CARTESIAN_POINT('Ctrl Pts',(72.0203115207733,125.639358981532,47.5487723172087));
#45244=CARTESIAN_POINT('Ctrl Pts',(77.2847411767612,125.108968957652,46.7525619622429));
#45245=CARTESIAN_POINT('Ctrl Pts',(81.5060552979621,124.472500928994,51.5741842746995));
#45246=CARTESIAN_POINT('Ctrl Pts',(79.728482568503,123.836032900338,57.7182984199529));
#45247=CARTESIAN_POINT('Ctrl Pts',(73.6016194435095,123.19956487168,59.5544497443309));
#45248=CARTESIAN_POINT('Ctrl Pts',(68.7399147931205,122.563096843024,55.3793614187719));
#45249=CARTESIAN_POINT('Ctrl Pts',(69.4858278482179,122.032706819143,50.107570048997));
#45250=CARTESIAN_POINT('Ctrl Pts',(72.5283512255512,121.608394800038,47.6963547154323));
#45251=CARTESIAN_POINT('Ctrl Pts',(76.33686993267,121.184082780934,46.9439630993421));
#45252=CARTESIAN_POINT('Ctrl Pts',(80.833597854669,120.653692757053,49.7948591914003));
#45253=CARTESIAN_POINT('Ctrl Pts',(80.8590072572753,120.017224728396,56.2032044533298));
#45254=CARTESIAN_POINT('Ctrl Pts',(75.4880780795087,119.380756699739,59.6763907722353));
#45255=CARTESIAN_POINT('Ctrl Pts',(69.6582969414783,118.744288671082,57.0451258062755));
#45256=CARTESIAN_POINT('Ctrl Pts',(68.7254440554294,118.107820642425,50.7049901510374));
#45257=CARTESIAN_POINT('Ctrl Pts',(72.7454665815478,117.577430618544,47.2139173328772));
#45258=CARTESIAN_POINT('Ctrl Pts',(76.6236647050234,117.153118599439,47.3885231790242));
#45259=CARTESIAN_POINT('Ctrl Pts',(79.9924504918158,116.728806580335,49.3178210329446));
#45260=CARTESIAN_POINT('Ctrl Pts',(81.5180565489095,116.198416556454,54.4188696203192));
#45261=CARTESIAN_POINT('Ctrl Pts',(77.3351104931415,115.561948527797,59.2738152357066));
#45262=CARTESIAN_POINT('Ctrl Pts',(71.002608172017,114.92548049914,58.3741943203373));
#45263=CARTESIAN_POINT('Ctrl Pts',(68.326532179209,114.289012470483,52.5648466186468));
#45264=CARTESIAN_POINT('Ctrl Pts',(71.7796338362221,113.652544441826,47.1663631667719));
#45265=CARTESIAN_POINT('Ctrl Pts',(77.1039338323076,113.122154417946,47.1666527860612));
#45266=CARTESIAN_POINT('Ctrl Pts',(79.9174693977396,112.697842398841,49.8415220367884));
#45267=CARTESIAN_POINT('Ctrl Pts',(81.1957996614328,112.273530379737,53.5071433515677));
#45268=CARTESIAN_POINT('Ctrl Pts',(79.0027289300506,111.743140355855,58.3588040259504));
#45269=CARTESIAN_POINT('Ctrl Pts',(72.6610927960897,111.106672327199,59.2814013261173));
#45270=CARTESIAN_POINT('Ctrl Pts',(68.4699764911283,110.470204298542,54.4497921162674));
#45271=CARTESIAN_POINT('Ctrl Pts',(70.2588968349819,109.833736269885,48.3089723467443));
#45272=CARTESIAN_POINT('Ctrl Pts',(76.4059152161931,109.197268241228,46.4974261411829));
#45273=CARTESIAN_POINT('Ctrl Pts',(80.4255579194777,108.666878217347,49.9889362829594));
#45274=CARTESIAN_POINT('Ctrl Pts',(80.7957838280293,108.242566198242,53.8533690567407));
#45275=CARTESIAN_POINT('Ctrl Pts',(79.3572700732904,107.818254179138,57.4591402729806));
#45276=CARTESIAN_POINT('Ctrl Pts',(74.52013864804,107.287864155257,59.6840740039152));
#45277=CARTESIAN_POINT('Ctrl Pts',(69.1272472113271,106.6513961266,56.2222455007014));
#45278=CARTESIAN_POINT('Ctrl Pts',(69.1311857674209,106.014928097943,49.8261617046435));
#45279=CARTESIAN_POINT('Ctrl Pts',(74.5085221507447,105.378460069286,46.362903576955));
#45280=CARTESIAN_POINT('Ctrl Pts',(80.3373861944358,104.741992040629,49.0259617051221));
#45281=CARTESIAN_POINT('Ctrl Pts',(81.0827257190345,104.211602016748,54.2978341926989));
#45282=CARTESIAN_POINT('Ctrl Pts',(78.8282293448942,103.787289997644,57.4582382784806));
#45283=CARTESIAN_POINT('Ctrl Pts',(75.3777508129794,103.362977978539,59.2373126971688));
#45284=CARTESIAN_POINT('Ctrl Pts',(70.2667783164759,102.832587954658,57.7452903541108));
#45285=CARTESIAN_POINT('Ctrl Pts',(68.4651765033714,102.196119926002,51.5953500665264));
#45286=CARTESIAN_POINT('Ctrl Pts',(72.6622400074956,101.559651897344,46.7689060980581));
#45287=CARTESIAN_POINT('Ctrl Pts',(78.9930695612056,100.923183868688,47.6802241546619));
#45288=CARTESIAN_POINT('Ctrl Pts',(81.647605490126,100.286715840031,53.5129742466773));
#45289=CARTESIAN_POINT('Ctrl Pts',(78.7534215822551,99.7563258161497,57.9819640698496));
#45290=CARTESIAN_POINT('Ctrl Pts',(74.9789179052989,99.3320137970452,58.8897249850046));
#45291=CARTESIAN_POINT('Ctrl Pts',(71.2072270700948,98.9077017779404,57.9703468636246));
#45292=CARTESIAN_POINT('Ctrl Pts',(68.3268166778703,98.3773117540599,53.4924671751376));
#45293=CARTESIAN_POINT('Ctrl Pts',(70.9992987716281,97.7408437254027,47.6679179142612));
#45294=CARTESIAN_POINT('Ctrl Pts',(77.3329042202886,97.1043756967459,46.7760964864426));
#45295=CARTESIAN_POINT('Ctrl Pts',(81.5150874496195,96.4679076680889,51.6154401273427));
#45296=CARTESIAN_POINT('Ctrl Pts',(79.6945588159604,95.8314396394319,57.7598042220118));
#45297=CARTESIAN_POINT('Ctrl Pts',(74.57901668281,95.3010496155514,59.2360830629346));
#45298=CARTESIAN_POINT('Ctrl Pts',(71.1340321876925,94.8767375964465,57.4463932253265));
#45299=CARTESIAN_POINT('Ctrl Pts',(68.8892772267267,94.452425577342,54.2790626376455));
#45300=CARTESIAN_POINT('Ctrl Pts',(69.6508450514793,93.9220355534612,49.0095100019376));
#45301=CARTESIAN_POINT('Ctrl Pts',(75.4878808899357,93.285567524804,46.3644112789393));
#45302=CARTESIAN_POINT('Ctrl Pts',(80.8545285853664,92.6490994961474,49.8442095419927));
#45303=CARTESIAN_POINT('Ctrl Pts',(80.8387738990692,92.0126314674903,56.240275147369));
#45304=CARTESIAN_POINT('Ctrl Pts',(75.4352492268543,91.3761634388334,59.6854827972209));
#45305=CARTESIAN_POINT('Ctrl Pts',(70.6049911897418,90.8457734149526,57.4456663254745));
#45306=CARTESIAN_POINT('Ctrl Pts',(69.1775862436694,90.4214613958479,53.8354830882459));
#45307=CARTESIAN_POINT('Ctrl Pts',(69.5597087935644,89.9971493767433,49.9722085389421));
#45308=CARTESIAN_POINT('Ctrl Pts',(73.5900826298085,89.4667593528626,46.493091226704));
#45309=CARTESIAN_POINT('Ctrl Pts',(79.7314942136654,88.8302913242055,48.3235552092793));
#45310=CARTESIAN_POINT('Ctrl Pts',(81.5014987995875,88.1938232955488,54.4698538681659));
#45311=CARTESIAN_POINT('Ctrl Pts',(77.2955260761042,87.5573552668916,59.2885359377501));
#45312=CARTESIAN_POINT('Ctrl Pts',(70.9567606325384,86.9208872382348,58.3464174285945));
#45313=CARTESIAN_POINT('Ctrl Pts',(68.7786383180496,86.3904972143539,53.4880273953303));
#45314=CARTESIAN_POINT('Ctrl Pts',(70.0682487881018,85.9661851952494,49.8263593707863));
#45315=CARTESIAN_POINT('Ctrl Pts',(72.8900068067502,85.5418731761447,47.1601655348787));
#45316=CARTESIAN_POINT('Ctrl Pts',(78.2142824574917,85.0114831522641,47.1762691716988));
#45317=CARTESIAN_POINT('Ctrl Pts',(81.6507460849712,84.3750151236068,52.5853589630448));
#45318=CARTESIAN_POINT('Ctrl Pts',(78.9567960842213,83.7385470949501,58.3864396237387));
#45319=CARTESIAN_POINT('Ctrl Pts',(72.6215538909905,83.102079066293,59.2665588153995));
#45320=CARTESIAN_POINT('Ctrl Pts',(68.4535757982522,82.4656110376363,54.3987571295987));
#45321=CARTESIAN_POINT('Ctrl Pts',(69.9948804987645,81.9352210137553,49.3024299862164));
#45322=CARTESIAN_POINT('Ctrl Pts',(73.3695905296702,81.5109089946509,47.3835136009241));
#45323=CARTESIAN_POINT('Ctrl Pts',(77.2483078732814,81.0865969755459,47.2208493614383));
#45324=CARTESIAN_POINT('Ctrl Pts',(81.2575625050972,80.5562069516654,50.724283081299));
#45325=CARTESIAN_POINT('Ctrl Pts',(80.3051930785702,79.9197389230083,57.0615164768155));
#45326=CARTESIAN_POINT('Ctrl Pts',(74.4673380396858,79.2832708943515,59.6748193646171));
#45327=CARTESIAN_POINT('Ctrl Pts',(69.107128087849,78.6468028656945,56.1851126848734));
#45328=CARTESIAN_POINT('Ctrl Pts',(69.1522683461807,78.0103348370375,49.7768760326491));
#45329=CARTESIAN_POINT('Ctrl Pts',(73.6577527209851,77.4799448131567,46.9398386552797));
#45330=CARTESIAN_POINT('Ctrl Pts',(77.4639367994623,77.0556327940522,47.7039529446272));
#45331=CARTESIAN_POINT('Ctrl Pts',(80.4990217432763,76.6313207749475,50.1245246271578));
#45332=CARTESIAN_POINT('Ctrl Pts',(81.2286996794729,76.1009307510668,55.3985876379329));
#45333=CARTESIAN_POINT('Ctrl Pts',(76.3541631842683,75.4644627224097,59.5586872269757));
#45334=CARTESIAN_POINT('Ctrl Pts',(70.2329825190307,74.8279946937529,57.7036802992425));
#45335=CARTESIAN_POINT('Ctrl Pts',(68.4743356369337,74.1915266650958,51.554122218981));
#45336=CARTESIAN_POINT('Ctrl Pts',(72.7104752843599,73.555058636439,46.7455199770257));
#45337=CARTESIAN_POINT('Ctrl Pts',(77.9724284950027,73.0246686125582,47.5579354749106));
#45338=CARTESIAN_POINT('Ctrl Pts',(80.3450365744471,72.6003565934535,50.630660452482));
#45339=CARTESIAN_POINT('Ctrl Pts',(81.0492816689046,72.176044574349,54.4483753100075));
#45340=CARTESIAN_POINT('Ctrl Pts',(78.1418369156852,71.6456545504681,58.908749233702));
#45341=CARTESIAN_POINT('Ctrl Pts',(71.7336816537533,71.0091865218112,58.8532445239228));
#45342=CARTESIAN_POINT('Ctrl Pts',(68.3285858083172,70.3727184931542,53.4388908485694));
#45343=CARTESIAN_POINT('Ctrl Pts',(71.0332481390232,69.7362504644973,47.6427968952868));
#45344=CARTESIAN_POINT('Ctrl Pts',(77.3846566580606,69.0997824358403,46.7900692376301));
#45345=CARTESIAN_POINT('Ctrl Pts',(80.8246941917609,68.5693924119597,50.8538497802933));
#45346=CARTESIAN_POINT('Ctrl Pts',(80.6011359407797,68.1450803928549,54.7295341837058));
#45347=CARTESIAN_POINT('Ctrl Pts',(78.6294574171612,67.7207683737503,58.0736920277588));
#45348=CARTESIAN_POINT('Ctrl Pts',(73.5095530650882,67.1903783498695,59.534770382201));
#45349=CARTESIAN_POINT('Ctrl Pts',(68.7078085314535,66.5539103212125,55.2908589708327));
#45350=CARTESIAN_POINT('Ctrl Pts',(69.6873122266739,65.9174422925556,48.9702200830722));
#45351=CARTESIAN_POINT('Ctrl Pts',(75.5299851241042,65.2809742638987,46.3677065188326));
#45352=CARTESIAN_POINT('Ctrl Pts',(80.8844392196639,64.6445062352417,49.8886944444544));
#45353=CARTESIAN_POINT('Ctrl Pts',(80.8169247461073,64.1141162113609,55.2125663745499));
#45354=CARTESIAN_POINT('Ctrl Pts',(78.1067448734721,63.6898041922563,57.9921046355568));
#45355=CARTESIAN_POINT('Ctrl Pts',(74.4252754900851,63.2654921731517,59.2240506837341));
#45356=CARTESIAN_POINT('Ctrl Pts',(69.6016913704958,62.7351021492708,56.9698974561461));
#45357=CARTESIAN_POINT('Ctrl Pts',(68.7592374263501,62.0986341206141,50.6171180655309));
#45358=CARTESIAN_POINT('Ctrl Pts',(73.6433787437401,61.4621660919569,46.4873399806718));
#45359=CARTESIAN_POINT('Ctrl Pts',(79.7611220203028,60.8256980633001,48.3536520233085));
#45360=CARTESIAN_POINT('Ctrl Pts',(81.4949112636297,60.1892300346431,54.5230530877197));
#45361=CARTESIAN_POINT('Ctrl Pts',(77.9529272269266,59.6588400107624,58.4982913970464));
#45362=CARTESIAN_POINT('Ctrl Pts',(74.0841280030346,59.2345279916577,58.8196952732654));
#45363=CARTESIAN_POINT('Ctrl Pts',(70.4968069555375,58.8102159725532,57.3357695377179));
#45364=CARTESIAN_POINT('Ctrl Pts',(68.3331244406284,58.2798259486722,52.4709315643751));
#45365=CARTESIAN_POINT('Ctrl Pts',(71.8627679117568,57.6433579200153,47.1221792238239));
#45366=CARTESIAN_POINT('Ctrl Pts',(78.2582921364095,57.0068898913583,47.2068747390464));
#45367=CARTESIAN_POINT('Ctrl Pts',(81.6533796843252,56.3704218627016,52.6275097553897));
#45368=CARTESIAN_POINT('Ctrl Pts',(78.9169383049789,55.7339538340444,58.4222852653844));
#45369=CARTESIAN_POINT('Ctrl Pts',(73.6360753535378,55.2035638101638,59.1010024526532));
#45370=CARTESIAN_POINT('Ctrl Pts',(70.5043885727656,54.779251791059,56.8067823687086));
#45371=CARTESIAN_POINT('Ctrl Pts',(68.7690218812751,54.3549397719544,53.334116198098));
#45372=CARTESIAN_POINT('Ctrl Pts',(70.325456686331,53.8245497480737,48.2423894546636));
#45373=CARTESIAN_POINT('Ctrl Pts',(76.4976538658095,53.1880817194167,46.5185807032441));
#45374=CARTESIAN_POINT('Ctrl Pts',(81.2707207768341,52.5516136907598,50.7762485744269));
#45375=CARTESIAN_POINT('Ctrl Pts',(80.2795419932234,51.9151456621028,57.0950671394231));
#45376=CARTESIAN_POINT('Ctrl Pts',(74.4137405368346,51.2786776334458,59.6757468770239));
#45377=CARTESIAN_POINT('Ctrl Pts',(69.9816490550362,50.7482876095651,56.7253679811584));
#45378=CARTESIAN_POINT('Ctrl Pts',(69.1216175708044,50.3239755904604,52.9397037418783));
#45379=CARTESIAN_POINT('Ctrl Pts',(70.0885439635866,49.8996635713559,49.1799216687548));
#45380=CARTESIAN_POINT('Ctrl Pts',(74.6024349177723,49.369273547475,46.3562788113952));
#45381=CARTESIAN_POINT('Ctrl Pts',(80.3927770014313,48.7328055188181,49.1020889264681));
#45382=CARTESIAN_POINT('Ctrl Pts',(81.2045589222609,48.0963374901611,55.4464496942236));
#45383=CARTESIAN_POINT('Ctrl Pts',(76.3127965798036,47.4598694615042,59.5671977602111));
#45384=CARTESIAN_POINT('Ctrl Pts',(70.1919083484634,46.8234014328472,57.6692351964939));
#45385=CARTESIAN_POINT('Ctrl Pts',(68.7803362744653,46.2930114089665,52.535461261843));
#45386=CARTESIAN_POINT('Ctrl Pts',(70.6133799988629,45.8686993898619,49.113348085619));
#45387=CARTESIAN_POINT('Ctrl Pts',(73.808800501213,45.4443873707573,46.9087629319908));
#45388=CARTESIAN_POINT('Ctrl Pts',(79.0683174983399,44.9139973468763,47.7368036852939));
#45389=CARTESIAN_POINT('Ctrl Pts',(81.6395066702259,44.2775293182195,53.6067713918667));
#45390=CARTESIAN_POINT('Ctrl Pts',(78.0922262264452,43.6410612895625,58.9290551959863));
#45391=CARTESIAN_POINT('Ctrl Pts',(71.6968693820735,43.0045932609057,58.8325447221204));
#45392=CARTESIAN_POINT('Ctrl Pts',(68.3201615278016,42.3681252322486,53.3859514106338));
#45393=CARTESIAN_POINT('Ctrl Pts',(70.6207865388037,41.8377352083679,48.584358436323));
#45394=CARTESIAN_POINT('Ctrl Pts',(74.2487044880827,41.4134231892631,47.2026496248374));
#45395=CARTESIAN_POINT('Ctrl Pts',(78.1068463906541,40.9891111701586,47.6335196122566));
#45396=CARTESIAN_POINT('Ctrl Pts',(81.5347986752688,40.4587211462778,51.7074996891105));
#45397=CARTESIAN_POINT('Ctrl Pts',(79.6269388331483,39.8222531176209,57.8253102007773));
#45398=CARTESIAN_POINT('Ctrl Pts',(73.4587819402533,39.185785088964,59.5175702230695));
#45399=CARTESIAN_POINT('Ctrl Pts',(68.6935887976469,38.5493170603069,55.2510918448196));
#45400=CARTESIAN_POINT('Ctrl Pts',(69.715665777593,37.91284903165,48.9247269106014));
#45401=CARTESIAN_POINT('Ctrl Pts',(74.601169621109,37.3824590077692,46.808120492965));
#45402=CARTESIAN_POINT('Ctrl Pts',(78.2462630815789,36.9581469886647,48.1438605690558));
#45403=CARTESIAN_POINT('Ctrl Pts',(80.8766167330158,36.5338349695599,50.9990571568275));
#45404=CARTESIAN_POINT('Ctrl Pts',(80.793289809878,36.0034449456793,56.3227050749385));
#45405=CARTESIAN_POINT('Ctrl Pts',(75.3412422253247,35.3669769170222,59.6905993383795));
#45406=CARTESIAN_POINT('Ctrl Pts',(69.574637925996,34.7305088883653,56.9236193432539));
#45407=CARTESIAN_POINT('Ctrl Pts',(68.7745779741261,34.0940408597084,50.5777697144526));
#45408=CARTESIAN_POINT('Ctrl Pts',(73.6946167383032,33.4575728310515,46.4715849653604));
#45409=CARTESIAN_POINT('Ctrl Pts',(78.7710770544774,32.9271828071706,48.0771132866675));
#45410=CARTESIAN_POINT('Ctrl Pts',(80.6472312224613,32.5028707880661,51.4757826473492));
#45411=CARTESIAN_POINT('Ctrl Pts',(80.7609096169022,32.0785587689613,55.3562446188384));
#45412=CARTESIAN_POINT('Ctrl Pts',(77.2071341131469,31.5481687450806,59.3209451361635));
#45413=CARTESIAN_POINT('Ctrl Pts',(70.8824305329507,30.9117007164236,58.2886374013044));
#45414=CARTESIAN_POINT('Ctrl Pts',(68.3430450059106,30.2752326877667,52.4182520125253));
#45415=CARTESIAN_POINT('Ctrl Pts',(71.9001517916369,29.6387646591098,47.1025305483846));
#45416=CARTESIAN_POINT('Ctrl Pts',(78.3073076922158,29.0022966304529,47.2285779136388));
#45417=CARTESIAN_POINT('Ctrl Pts',(81.0872324480072,28.471906606572,51.7695237430829));
#45418=CARTESIAN_POINT('Ctrl Pts',(80.275122006266,28.0475945874674,55.565756650326));
#45419=CARTESIAN_POINT('Ctrl Pts',(77.8164221205999,27.6232825683628,58.5700374594237));
#45420=CARTESIAN_POINT('Ctrl Pts',(72.5335666026989,27.092892544482,59.2330665250225));
#45421=CARTESIAN_POINT('Ctrl Pts',(68.4353446939828,26.4564245158251,54.3063931884985));
#45422=CARTESIAN_POINT('Ctrl Pts',(70.3674902113553,25.8199564871681,48.2091214630561));
#45423=CARTESIAN_POINT('Ctrl Pts',(76.5387626327649,25.1834884585111,46.5282601413106));
#45424=CARTESIAN_POINT('Ctrl Pts',(81.2934963114684,24.5470204298542,50.8247743089652));
#45425=CARTESIAN_POINT('Ctrl Pts',(80.414707068145,24.0166304059735,56.0760531511082));
#45426=CARTESIAN_POINT('Ctrl Pts',(77.3122715737554,23.5923183868688,58.4096717625035));
#45427=CARTESIAN_POINT('Ctrl Pts',(73.4859668057208,23.1680063677642,59.0656658471794));
#45428=CARTESIAN_POINT('Ctrl Pts',(69.0626632683662,22.6376163438834,56.1021187103944));
#45429=CARTESIAN_POINT('Ctrl Pts',(69.1990635927837,22.0011483152264,49.695206442741));
#45430=CARTESIAN_POINT('Ctrl Pts',(74.6559956914946,21.3646802865695,46.3586883014623));
#45431=CARTESIAN_POINT('Ctrl Pts',(80.4174464448778,20.7282122579125,49.1364208319506));
#45432=CARTESIAN_POINT('Ctrl Pts',(81.1899753790609,20.0917442292556,55.4978865304285));
#45433=CARTESIAN_POINT('Ctrl Pts',(77.0829706090005,19.5613542053749,58.8867113839554));
#45434=CARTESIAN_POINT('Ctrl Pts',(73.2105872069091,19.1370421862702,58.6136853706606));
#45435=CARTESIAN_POINT('Ctrl Pts',(69.8912577533702,18.7127301671655,56.6010225426405));
#45436=CARTESIAN_POINT('Ctrl Pts',(68.4956769583314,18.1823401432847,51.4606824589819));
#45437=CARTESIAN_POINT('Ctrl Pts',(72.7985336869453,17.5458721146278,46.717269598202));
#45438=CARTESIAN_POINT('Ctrl Pts',(79.1086961350004,16.9094040859709,47.76874527729));
#45439=CARTESIAN_POINT('Ctrl Pts',(81.6326438925532,16.272936057314,53.6584623286513));
#45440=CARTESIAN_POINT('Ctrl Pts',(78.6506201566575,15.7425460334332,58.0582788876747));
#45441=CARTESIAN_POINT('Ctrl Pts',(74.8443820757933,15.3182340143285,58.8942202496515));
#45442=CARTESIAN_POINT('Ctrl Pts',(72.983431993014,15.1060780047762,58.3814745569358));
#45443=CARTESIAN_POINT('Ctrl Pts',(72.1688064861966,15.,57.9117293166054));
#45444=CARTESIAN_POINT('Ctrl Pts',(80.7895856589294,416.407550721688,50.3113098152966));
#45445=CARTESIAN_POINT('Ctrl Pts',(81.2413947982782,416.301472716912,51.2780186311425));
#45446=CARTESIAN_POINT('Ctrl Pts',(81.6399980963661,416.08931670736,53.431861897913));
#45447=CARTESIAN_POINT('Ctrl Pts',(80.3245054469483,415.665004688255,57.6537570089119));
#45448=CARTESIAN_POINT('Ctrl Pts',(75.0599862662509,415.134614664374,60.5970028556877));
#45449=CARTESIAN_POINT('Ctrl Pts',(68.6468240838236,414.498146635717,57.1703399986101));
#45450=CARTESIAN_POINT('Ctrl Pts',(68.0721122133495,413.86167860706,49.9338964270263));
#45451=CARTESIAN_POINT('Ctrl Pts',(73.8536277062205,413.225210578404,45.5307843216615));
#45452=CARTESIAN_POINT('Ctrl Pts',(79.5293668686138,412.694820554522,47.608817812333));
#45453=CARTESIAN_POINT('Ctrl Pts',(81.4818216899602,412.270508535419,51.5574321359389));
#45454=CARTESIAN_POINT('Ctrl Pts',(81.4136646470584,411.846196516312,55.9620266993605));
#45455=CARTESIAN_POINT('Ctrl Pts',(77.182673447473,411.315806492434,60.2755324159434));
#45456=CARTESIAN_POINT('Ctrl Pts',(70.0657272634679,410.679338463775,58.7830751157563));
#45457=CARTESIAN_POINT('Ctrl Pts',(67.485953158802,410.04287043512,51.9990045803245));
#45458=CARTESIAN_POINT('Ctrl Pts',(71.7891733015741,409.406402406461,46.1542126641332));
#45459=CARTESIAN_POINT('Ctrl Pts',(79.045951076736,408.769934377805,46.623478484056));
#45460=CARTESIAN_POINT('Ctrl Pts',(81.9660221235307,408.239544353924,51.9127534736459));
#45461=CARTESIAN_POINT('Ctrl Pts',(80.8520208784144,407.815232334819,56.1748467453594));
#45462=CARTESIAN_POINT('Ctrl Pts',(77.9117788239603,407.390920315716,59.4552955240192));
#45463=CARTESIAN_POINT('Ctrl Pts',(71.8892887985956,406.860530291833,59.9378154737378));
#45464=CARTESIAN_POINT('Ctrl Pts',(67.4944491078429,406.224062263178,54.1441181451339));
#45465=CARTESIAN_POINT('Ctrl Pts',(69.9953373217988,405.58759423452,47.3305926903669));
#45466=CARTESIAN_POINT('Ctrl Pts',(77.0767924089223,404.951126205863,45.7394991594704));
#45467=CARTESIAN_POINT('Ctrl Pts',(82.2479624544353,404.314658177207,50.8522825051723));
#45468=CARTESIAN_POINT('Ctrl Pts',(80.9842660833594,403.784268153325,56.7604331801431));
#45469=CARTESIAN_POINT('Ctrl Pts',(77.3484330715765,403.359956134221,59.2478253779512));
#45470=CARTESIAN_POINT('Ctrl Pts',(72.9774724614809,402.935644115116,59.7965549476201));
#45471=CARTESIAN_POINT('Ctrl Pts',(68.1141092087561,402.405254091235,56.2117436971656));
#45472=CARTESIAN_POINT('Ctrl Pts',(68.5951035493501,401.768786062579,48.9556979554233));
#45473=CARTESIAN_POINT('Ctrl Pts',(74.951086404199,401.132318033922,45.4514063382047));
#45474=CARTESIAN_POINT('Ctrl Pts',(81.3408903658783,400.495850005264,48.8936415491659));
#45475=CARTESIAN_POINT('Ctrl Pts',(81.8925163663265,399.859381976608,56.1446596895001));
#45476=CARTESIAN_POINT('Ctrl Pts',(77.0642901766376,399.328991952727,59.7766571422207));
#45477=CARTESIAN_POINT('Ctrl Pts',(72.6881935969392,398.904679933622,59.2705150455746));
#45478=CARTESIAN_POINT('Ctrl Pts',(69.028312474448,398.480367914518,56.8186440741339));
#45479=CARTESIAN_POINT('Ctrl Pts',(67.7071462846999,397.949977890636,50.9230784909119));
#45480=CARTESIAN_POINT('Ctrl Pts',(72.8282865991981,397.31350986198,45.7601842258385));
#45481=CARTESIAN_POINT('Ctrl Pts',(79.9248984922716,396.677041833323,47.2822477977728));
#45482=CARTESIAN_POINT('Ctrl Pts',(82.4920145257144,396.040573804666,54.0710984478771));
#45483=CARTESIAN_POINT('Ctrl Pts',(78.1537966050903,395.404105776009,59.9073147380206));
#45484=CARTESIAN_POINT('Ctrl Pts',(72.1268967499142,394.873715752128,59.4834612461347));
#45485=CARTESIAN_POINT('Ctrl Pts',(69.1548466821309,394.449403733024,56.2317971356439));
#45486=CARTESIAN_POINT('Ctrl Pts',(67.9994059152317,394.025091713919,51.9807551778361));
#45487=CARTESIAN_POINT('Ctrl Pts',(70.8678150888879,393.494701690038,46.6632931460518));
#45488=CARTESIAN_POINT('Ctrl Pts',(78.1197159299898,392.858233661381,46.1233954679321));
#45489=CARTESIAN_POINT('Ctrl Pts',(82.4795800207196,392.221765632725,51.9259951429827));
#45490=CARTESIAN_POINT('Ctrl Pts',(79.9661078860758,391.585297604067,58.7348890110715));
#45491=CARTESIAN_POINT('Ctrl Pts',(72.8637954461731,390.948829575411,60.2965270350745));
#45492=CARTESIAN_POINT('Ctrl Pts',(68.5914342841124,390.418439551529,56.0245130196589));
#45493=CARTESIAN_POINT('Ctrl Pts',(68.4797507593773,389.994127532425,51.6206592660523));
#45494=CARTESIAN_POINT('Ctrl Pts',(70.3949223493767,389.56981551332,47.6534790491081));
#45495=CARTESIAN_POINT('Ctrl Pts',(76.0473714332612,389.03942548944,45.5197046933984));
#45496=CARTESIAN_POINT('Ctrl Pts',(81.8765635723464,388.402957460782,49.8673562799026));
#45497=CARTESIAN_POINT('Ctrl Pts',(81.3633237207986,387.766489432126,57.1071879584235));
#45498=CARTESIAN_POINT('Ctrl Pts',(75.0008778710985,387.130021403469,60.5997315427138));
#45499=CARTESIAN_POINT('Ctrl Pts',(68.6146410439638,386.493553374812,57.1215805253265));
#45500=CARTESIAN_POINT('Ctrl Pts',(68.1902978235643,385.963163350931,51.094715131252));
#45501=CARTESIAN_POINT('Ctrl Pts',(70.9937063513919,385.538851331826,47.6965830386227));
#45502=CARTESIAN_POINT('Ctrl Pts',(75.0410462321251,385.114539312722,45.9572035565431));
#45503=CARTESIAN_POINT('Ctrl Pts',(80.7078056992447,384.584149288842,48.0526774382226));
#45504=CARTESIAN_POINT('Ctrl Pts',(82.2579545906091,383.947681260183,55.1575063402167));
#45505=CARTESIAN_POINT('Ctrl Pts',(77.1231010004394,383.311213231528,60.2870147461023));
#45506=CARTESIAN_POINT('Ctrl Pts',(70.0293130803531,382.674745202869,58.7518434776859));
#45507=CARTESIAN_POINT('Ctrl Pts',(67.4884412136621,382.038277174214,51.9382155549809));
#45508=CARTESIAN_POINT('Ctrl Pts',(71.1200463257472,381.507887150331,47.1096942537058));
#45509=CARTESIAN_POINT('Ctrl Pts',(75.4648621085364,381.083575131228,46.3823862677193));
#45510=CARTESIAN_POINT('Ctrl Pts',(79.661152632736,380.659263112123,47.7231125370846));
#45511=CARTESIAN_POINT('Ctrl Pts',(82.5654807936886,380.128873088243,53.0210415268397));
#45512=CARTESIAN_POINT('Ctrl Pts',(79.077005396985,379.492405059585,59.4016445327163));
#45513=CARTESIAN_POINT('Ctrl Pts',(71.8366431041545,378.855937030929,59.9073437981783));
#45514=CARTESIAN_POINT('Ctrl Pts',(67.4875061865788,378.219469002271,54.096699604054));
#45515=CARTESIAN_POINT('Ctrl Pts',(70.037039744923,377.583000973615,47.2863079892577));
#45516=CARTESIAN_POINT('Ctrl Pts',(75.9450877467993,377.052610949733,46.0221313977504));
#45517=CARTESIAN_POINT('Ctrl Pts',(79.7023283940244,376.62829893063,48.3220322242411));
#45518=CARTESIAN_POINT('Ctrl Pts',(81.9913653223898,376.203986911524,52.0859013815623));
#45519=CARTESIAN_POINT('Ctrl Pts',(80.7101262330765,375.673596887645,57.9902726472438));
#45520=CARTESIAN_POINT('Ctrl Pts',(73.8923976840809,375.037128858986,60.5201210111223));
#45521=CARTESIAN_POINT('Ctrl Pts',(68.0943419684742,374.40066083033,56.1542158590086));
#45522=CARTESIAN_POINT('Ctrl Pts',(68.6209558225136,373.764192801673,48.915344695128));
#45523=CARTESIAN_POINT('Ctrl Pts',(75.0116100672234,373.127724773017,45.4453167937154));
#45524=CARTESIAN_POINT('Ctrl Pts',(80.3011266292082,372.597334749135,48.3649380341302));
#45525=CARTESIAN_POINT('Ctrl Pts',(81.6297246308043,372.173022730031,52.5650842747992));
#45526=CARTESIAN_POINT('Ctrl Pts',(80.8898679317703,371.748710710926,56.9077808054986));
#45527=CARTESIAN_POINT('Ctrl Pts',(76.0508754272462,371.218320687045,60.5254216373323));
#45528=CARTESIAN_POINT('Ctrl Pts',(69.2446162674512,370.581852658388,57.9648764684838));
#45529=CARTESIAN_POINT('Ctrl Pts',(67.729944664901,369.945384629731,50.8666831902644));
#45530=CARTESIAN_POINT('Ctrl Pts',(72.8742657559371,369.308916601074,45.7466696755505));
#45531=CARTESIAN_POINT('Ctrl Pts',(79.9745867816891,368.672448572417,47.3173372544069));
#45532=CARTESIAN_POINT('Ctrl Pts',(82.0536812051091,368.142058548537,52.990126693959));
#45533=CARTESIAN_POINT('Ctrl Pts',(80.3026166120396,367.717746529432,57.0324247883297));
#45534=CARTESIAN_POINT('Ctrl Pts',(76.8963999262717,367.293434510327,59.8260047464567));
#45535=CARTESIAN_POINT('Ctrl Pts',(70.8707855677016,366.763044486447,59.3842522718924));
#45536=CARTESIAN_POINT('Ctrl Pts',(67.4110982780816,366.126576457789,52.9879940555559));
#45537=CARTESIAN_POINT('Ctrl Pts',(70.9220077724125,365.490108429133,46.6356643725854));
#45538=CARTESIAN_POINT('Ctrl Pts',(78.1632919396892,364.853640400476,46.1433418286396));
#45539=CARTESIAN_POINT('Ctrl Pts',(82.4940854177424,364.217172371819,51.9850695835472));
#45540=CARTESIAN_POINT('Ctrl Pts',(80.3439905932449,363.686782347938,57.6313308148986));
#45541=CARTESIAN_POINT('Ctrl Pts',(76.3712941874098,363.262470328833,59.5350336173121));
#45542=CARTESIAN_POINT('Ctrl Pts',(71.9677814533701,362.838158309729,59.4106282556724));
#45543=CARTESIAN_POINT('Ctrl Pts',(67.7081276982914,362.307768285848,55.1259434908579));
#45544=CARTESIAN_POINT('Ctrl Pts',(69.29027709203,361.671300257191,48.0281721076772));
#45545=CARTESIAN_POINT('Ctrl Pts',(76.106403722641,361.034832228534,45.534380690175));
#45546=CARTESIAN_POINT('Ctrl Pts',(81.8963839629881,360.398364199878,49.9109897308505));
#45547=CARTESIAN_POINT('Ctrl Pts',(81.3355385052593,359.76189617122,57.1613005989825));
#45548=CARTESIAN_POINT('Ctrl Pts',(76.0098121089718,359.231506147339,60.0143361751496));
#45549=CARTESIAN_POINT('Ctrl Pts',(71.7621258456939,358.807194128235,58.8466193851635));
#45550=CARTESIAN_POINT('Ctrl Pts',(68.5190612661091,358.382882109129,55.8651879796984));
#45551=CARTESIAN_POINT('Ctrl Pts',(68.1126206673736,357.85249208525,49.8370888027861));
#45552=CARTESIAN_POINT('Ctrl Pts',(73.9613452910871,357.216024056592,45.5157492433467));
#45553=CARTESIAN_POINT('Ctrl Pts',(80.7427514648477,356.579556027936,48.1024668902907));
#45554=CARTESIAN_POINT('Ctrl Pts',(82.2443072674208,355.943087999278,55.2034462629049));
#45555=CARTESIAN_POINT('Ctrl Pts',(77.0666400728443,355.306619970621,60.3096501105997));
#45556=CARTESIAN_POINT('Ctrl Pts',(71.1749158110719,354.776229946741,58.9714577215049));
#45557=CARTESIAN_POINT('Ctrl Pts',(68.7336281098145,354.351917927636,55.3045086555177));
#45558=CARTESIAN_POINT('Ctrl Pts',(68.2401302403252,353.927605908532,50.9269681422087));
#45559=CARTESIAN_POINT('Ctrl Pts',(71.8860608107843,353.397215884651,46.1092545846811));
#45560=CARTESIAN_POINT('Ctrl Pts',(79.1354550994434,352.760747855994,46.6818257676457));
#45561=CARTESIAN_POINT('Ctrl Pts',(82.5592164281373,352.124279827337,53.0815473430482));
#45562=CARTESIAN_POINT('Ctrl Pts',(79.0365776194958,351.48781179868,59.4273801254641));
#45563=CARTESIAN_POINT('Ctrl Pts',(71.7791726134526,350.851343770023,59.8874104399738));
#45564=CARTESIAN_POINT('Ctrl Pts',(68.2084260981037,350.320953746142,55.0137113345597));
#45565=CARTESIAN_POINT('Ctrl Pts',(68.7697806630927,349.896641727037,50.6443541569855));
#45566=CARTESIAN_POINT('Ctrl Pts',(71.2676660331981,349.472329707933,47.0157222149629));
#45567=CARTESIAN_POINT('Ctrl Pts',(77.1794427808517,348.941939684052,45.769099042993));
#45568=CARTESIAN_POINT('Ctrl Pts',(82.2772657295171,348.305471655395,50.9550181029155));
#45569=CARTESIAN_POINT('Ctrl Pts',(80.6657213081576,347.669003626738,58.0318466621302));
#45570=CARTESIAN_POINT('Ctrl Pts',(73.8449992740799,347.032535598081,60.5130416992796));
#45571=CARTESIAN_POINT('Ctrl Pts',(68.0640227548013,346.396067569424,56.101481227569));
#45572=CARTESIAN_POINT('Ctrl Pts',(68.5639383988084,345.865677545544,50.0804133824217));
#45573=CARTESIAN_POINT('Ctrl Pts',(71.8528685658973,345.441365526439,47.1496558952068));
#45574=CARTESIAN_POINT('Ctrl Pts',(76.118160318495,345.017053507335,46.047981098329));
#45575=CARTESIAN_POINT('Ctrl Pts',(81.3989818087853,344.486663483453,48.9833001669616));
#45576=CARTESIAN_POINT('Ctrl Pts',(81.8472735889369,343.850195454797,56.2414397214105));
#45577=CARTESIAN_POINT('Ctrl Pts',(75.9900885877292,343.213727426139,60.5276923668058));
#45578=CARTESIAN_POINT('Ctrl Pts',(69.2134726930078,342.577259397483,57.9284511517702));
#45579=CARTESIAN_POINT('Ctrl Pts',(67.7416333010628,341.940791368825,50.806987529991));
#45580=CARTESIAN_POINT('Ctrl Pts',(72.0672498319467,341.410401344945,46.5889055873615));
#45581=CARTESIAN_POINT('Ctrl Pts',(76.4721626684415,340.98608932584,46.5328342422951));
#45582=CARTESIAN_POINT('Ctrl Pts',(80.4148456024942,340.561777306736,48.4979429859479));
#45583=CARTESIAN_POINT('Ctrl Pts',(82.4770817672208,340.031387282855,54.1768826447122));
#45584=CARTESIAN_POINT('Ctrl Pts',(78.0561770688721,339.394919254198,59.9507164629067));
#45585=CARTESIAN_POINT('Ctrl Pts',(70.8234026819354,338.75845122554,59.3461070466697));
#45586=CARTESIAN_POINT('Ctrl Pts',(67.4114700530779,338.121983196884,52.9400713291086));
#45587=CARTESIAN_POINT('Ctrl Pts',(70.9699767657366,337.485515168227,46.5982588683077));
#45588=CARTESIAN_POINT('Ctrl Pts',(77.001719526524,336.955125144347,46.2500449761636));
#45589=CARTESIAN_POINT('Ctrl Pts',(80.364184772194,336.530813125241,49.0961350247236));
#45590=CARTESIAN_POINT('Ctrl Pts',(82.0523236900641,336.106501106137,53.1651137770432));
#45591=CARTESIAN_POINT('Ctrl Pts',(79.8854680545447,335.576111082256,58.8049639791148));
#45592=CARTESIAN_POINT('Ctrl Pts',(72.7616332336275,334.939643053599,60.2652833812645));
#45593=CARTESIAN_POINT('Ctrl Pts',(67.6973666273895,334.303175024943,55.0660736702146));
#45594=CARTESIAN_POINT('Ctrl Pts',(69.3219820447791,333.666706996285,47.9922343573584));
#45595=CARTESIAN_POINT('Ctrl Pts',(76.1671480162545,333.030238967629,45.5375942340481));
#45596=CARTESIAN_POINT('Ctrl Pts',(80.9494316003633,332.499848943748,49.2298750153747));
#45597=CARTESIAN_POINT('Ctrl Pts',(81.6218237505459,332.075536924643,53.5835274922297));
#45598=CARTESIAN_POINT('Ctrl Pts',(80.2282217793196,331.651224905538,57.7625554460304));
#45599=CARTESIAN_POINT('Ctrl Pts',(74.8940449044853,331.120834881658,60.5997601822053));
#45600=CARTESIAN_POINT('Ctrl Pts',(68.5579961719892,330.484366853,57.0310010461126));
#45601=CARTESIAN_POINT('Ctrl Pts',(68.1437543921941,329.847898824344,49.7848309110412));
#45602=CARTESIAN_POINT('Ctrl Pts',(74.0088478294097,329.211430795687,45.5094061542176));
#45603=CARTESIAN_POINT('Ctrl Pts',(80.7865060381157,328.57496276703,48.1447248290591));
#45604=CARTESIAN_POINT('Ctrl Pts',(81.9759865511057,328.044572743149,54.0682634468287));
#45605=CARTESIAN_POINT('Ctrl Pts',(79.6288299458803,327.620260724044,57.7961659352798));
#45606=CARTESIAN_POINT('Ctrl Pts',(75.8363593186907,327.19594870494,60.0374976007762));
#45607=CARTESIAN_POINT('Ctrl Pts',(69.9486356894012,326.665558681059,58.6818117551253));
#45608=CARTESIAN_POINT('Ctrl Pts',(67.5050699649132,326.029090652403,51.832684667524));
#45609=CARTESIAN_POINT('Ctrl Pts',(71.9438336438113,325.392622623745,46.0902152612994));
#45610=CARTESIAN_POINT('Ctrl Pts',(79.1754787318497,324.756154595088,46.708185486457));
#45611=CARTESIAN_POINT('Ctrl Pts',(82.564541311991,324.119686566431,53.1421430663524));
#45612=CARTESIAN_POINT('Ctrl Pts',(79.5783670997,323.58929654255,58.3943747083155));
#45613=CARTESIAN_POINT('Ctrl Pts',(75.3617807153705,323.164984523446,59.6698355490872));
#45614=CARTESIAN_POINT('Ctrl Pts',(71.028771816179,322.740672504341,58.8752067222889));
#45615=CARTESIAN_POINT('Ctrl Pts',(67.472516713564,322.210282480461,53.9909234286913));
#45616=CARTESIAN_POINT('Ctrl Pts',(70.1187939445722,321.573814451803,47.2175363787246));
#45617=CARTESIAN_POINT('Ctrl Pts',(77.2355457326337,320.937346423146,45.7926076557161));
#45618=CARTESIAN_POINT('Ctrl Pts',(82.290198667416,320.30087839449,51.0011642299913));
#45619=CARTESIAN_POINT('Ctrl Pts',(80.6300072817412,319.664410365832,58.081087949562));
#45620=CARTESIAN_POINT('Ctrl Pts',(74.9314192802274,319.134020341952,60.088391722286));
#45621=CARTESIAN_POINT('Ctrl Pts',(70.9115524333953,318.709708322847,58.2864284522404));
#45622=CARTESIAN_POINT('Ctrl Pts',(68.161202218195,318.285396303743,54.8452114020383));
#45623=CARTESIAN_POINT('Ctrl Pts',(68.6789991873789,317.755006279862,48.8256549444831));
#45624=CARTESIAN_POINT('Ctrl Pts',(75.1184297311182,317.118538251205,45.4470029078914));
#45625=CARTESIAN_POINT('Ctrl Pts',(81.4259241403883,316.482070222548,49.0378373729645));
#45626=CARTESIAN_POINT('Ctrl Pts',(81.8267786253167,315.845602193891,56.284760413845));
#45627=CARTESIAN_POINT('Ctrl Pts',(75.9308357102248,315.209134165234,60.5414507307445));
#45628=CARTESIAN_POINT('Ctrl Pts',(70.3121717567199,314.678744141353,58.3202373180855));
#45629=CARTESIAN_POINT('Ctrl Pts',(68.458780164777,314.254432122249,54.3238213362628));
#45630=CARTESIAN_POINT('Ctrl Pts',(68.6387745812983,313.830120103144,49.9222303622086));
#45631=CARTESIAN_POINT('Ctrl Pts',(72.9769004072191,313.299730079263,45.7170147951457));
#45632=CARTESIAN_POINT('Ctrl Pts',(80.0541297174874,312.663262050606,47.3886548885531));
#45633=CARTESIAN_POINT('Ctrl Pts',(82.4616615956628,312.026794021949,54.2357249286578));
#45634=CARTESIAN_POINT('Ctrl Pts',(78.0122968427819,311.390325993293,59.9699843555021));
#45635=CARTESIAN_POINT('Ctrl Pts',(70.7696451723068,310.753857964635,59.3176408170394));
#45636=CARTESIAN_POINT('Ctrl Pts',(67.9840799037379,310.223467940755,53.9563163741867));
#45637=CARTESIAN_POINT('Ctrl Pts',(69.2053351116376,309.79915592165,49.7237123518345));
#45638=CARTESIAN_POINT('Ctrl Pts',(72.227475957166,309.374843902546,46.5185499842403));
#45639=CARTESIAN_POINT('Ctrl Pts',(78.2602263630497,308.844453878664,46.1882528645145));
#45640=CARTESIAN_POINT('Ctrl Pts',(82.5073751721094,308.207985850008,52.0910727250313));
#45641=CARTESIAN_POINT('Ctrl Pts',(79.8352413443009,307.57151782135,58.8392783150243));
#45642=CARTESIAN_POINT('Ctrl Pts',(72.7158692846742,306.935049792694,60.2510571061724));
#45643=CARTESIAN_POINT('Ctrl Pts',(67.6754459456847,306.298581764036,55.0093314479775));
#45644=CARTESIAN_POINT('Ctrl Pts',(69.0879208695682,305.768191740156,49.1349729096867));
#45645=CARTESIAN_POINT('Ctrl Pts',(72.785401456947,305.343879721051,46.7401788895649));
#45646=CARTESIAN_POINT('Ctrl Pts',(77.168823957582,304.919567701947,46.3019914025474));
#45647=CARTESIAN_POINT('Ctrl Pts',(81.9401197854956,304.389177678066,50.0084600412286));
#45648=CARTESIAN_POINT('Ctrl Pts',(81.2760630292531,303.752709649409,57.2500471557014));
#45649=CARTESIAN_POINT('Ctrl Pts',(74.8336230054931,303.116241620752,60.5927323665434));
#45650=CARTESIAN_POINT('Ctrl Pts',(68.5327730738057,302.479773592095,56.9902515523144));
#45651=CARTESIAN_POINT('Ctrl Pts',(68.1644117867583,301.843305563438,49.7276166809875));
#45652=CARTESIAN_POINT('Ctrl Pts',(73.0828068247428,301.312915539558,46.2186903641038));
#45653=CARTESIAN_POINT('Ctrl Pts',(77.4447280224918,300.888603520453,46.835167904231));
#45654=CARTESIAN_POINT('Ctrl Pts',(81.0415322946407,300.464291501348,49.37866945145));
#45655=CARTESIAN_POINT('Ctrl Pts',(82.2134137079766,299.933901477468,55.3057148874212));
#45656=CARTESIAN_POINT('Ctrl Pts',(76.9635426598555,299.29743344881,60.3376538069737));
#45657=CARTESIAN_POINT('Ctrl Pts',(69.9076256472494,298.660965420154,58.6368854542147));
#45658=CARTESIAN_POINT('Ctrl Pts',(67.5127471671405,298.024497391496,51.7853794194773));
#45659=CARTESIAN_POINT('Ctrl Pts',(71.9969468835859,297.38802936284,46.0605642945113));
#45660=CARTESIAN_POINT('Ctrl Pts',(78.0112228190499,296.857639338958,46.6364623923447));
#45661=CARTESIAN_POINT('Ctrl Pts',(80.9002204941133,296.433327319855,49.9621342833063));
#45662=CARTESIAN_POINT('Ctrl Pts',(81.9479536881278,296.009015300749,54.2409958429987));
#45663=CARTESIAN_POINT('Ctrl Pts',(78.9461926833289,295.478625276869,59.4843349048045));
#45664=CARTESIAN_POINT('Ctrl Pts',(71.6829715334687,294.842157248211,59.8409493187482));
#45665=CARTESIAN_POINT('Ctrl Pts',(67.4710136627625,294.205689219555,53.9301127642556));
#45666=CARTESIAN_POINT('Ctrl Pts',(70.1556095780848,293.569221190898,47.1868551946558));
#45667=CARTESIAN_POINT('Ctrl Pts',(77.2950890531586,292.932753162241,45.8050490805407));
#45668=CARTESIAN_POINT('Ctrl Pts',(81.4582193150135,292.402363138361,50.1835785220108));
#45669=CARTESIAN_POINT('Ctrl Pts',(81.4586695413219,291.978051119255,54.5888481948173));
#45670=CARTESIAN_POINT('Ctrl Pts',(79.4439369285092,291.553739100151,58.5064052897073));
#45671=CARTESIAN_POINT('Ctrl Pts',(73.739412051243,291.02334907627,60.4967744945643));
#45672=CARTESIAN_POINT('Ctrl Pts',(68.0218570386755,290.386881047614,56.0033214804261));
#45673=CARTESIAN_POINT('Ctrl Pts',(68.7177396306583,289.750413018956,48.7787574592059));
#45674=CARTESIAN_POINT('Ctrl Pts',(75.1663439435118,289.113944990299,45.4479797279876));
#45675=CARTESIAN_POINT('Ctrl Pts',(81.4627210041053,288.477476961642,49.0862748263596));
#45676=CARTESIAN_POINT('Ctrl Pts',(81.7347500545205,287.947086937761,55.1219333523798));
#45677=CARTESIAN_POINT('Ctrl Pts',(78.8464322188351,287.522774918657,58.4481956951477));
#45678=CARTESIAN_POINT('Ctrl Pts',(74.7564632857218,287.098462899552,60.0848249198105));
#45679=CARTESIAN_POINT('Ctrl Pts',(69.1444214732981,286.568072875672,57.8469329781387));
#45680=CARTESIAN_POINT('Ctrl Pts',(67.7741643695786,285.931604847014,50.7052279449051));
#45681=CARTESIAN_POINT('Ctrl Pts',(73.0369013253525,285.295136818358,45.7070105013696));
#45682=CARTESIAN_POINT('Ctrl Pts',(80.0896642948305,284.6586687897,47.4208110658734));
#45683=CARTESIAN_POINT('Ctrl Pts',(82.4576813474655,284.022200761044,54.2964238058723));
#45684=CARTESIAN_POINT('Ctrl Pts',(78.7053135331846,283.491810737163,59.0317072644775));
#45685=CARTESIAN_POINT('Ctrl Pts',(74.3435184367344,283.067498718059,59.6490763837532));
#45686=CARTESIAN_POINT('Ctrl Pts',(70.1824192885522,282.643186698953,58.2028208835556));
#45687=CARTESIAN_POINT('Ctrl Pts',(67.4127902942353,282.112796675073,52.8332465167339));
#45688=CARTESIAN_POINT('Ctrl Pts',(71.0612642256814,281.476328646415,46.542762172618));
#45689=CARTESIAN_POINT('Ctrl Pts',(78.3120869932642,280.839860617759,46.2200439183594));
#45690=CARTESIAN_POINT('Ctrl Pts',(82.5131179862013,280.203392589102,52.1386515650035));
#45691=CARTESIAN_POINT('Ctrl Pts',(79.7924343265619,279.566924560445,58.882495849696));
#45692=CARTESIAN_POINT('Ctrl Pts',(73.8543494440967,279.036534536564,59.9970906530344));
#45693=CARTESIAN_POINT('Ctrl Pts',(70.1563794296432,278.61222251746,57.6030524609712));
#45694=CARTESIAN_POINT('Ctrl Pts',(67.9631103479317,278.187910498355,53.7825849728147));
#45695=CARTESIAN_POINT('Ctrl Pts',(69.3930268217517,277.657520474474,47.9124476213647));
#45696=CARTESIAN_POINT('Ctrl Pts',(76.2724605362172,277.021052445817,45.5555540980418));
#45697=CARTESIAN_POINT('Ctrl Pts',(81.9584281485478,276.384584417161,50.0664686605292));
#45698=CARTESIAN_POINT('Ctrl Pts',(81.2492000712417,275.748116388503,57.2897347786293));
#45699=CARTESIAN_POINT('Ctrl Pts',(74.7729648801304,275.111648359847,60.5972917413162));
#45700=CARTESIAN_POINT('Ctrl Pts',(69.5588554872861,274.581258335966,57.5450406234622));
#45701=CARTESIAN_POINT('Ctrl Pts',(68.3367351457568,274.156946316861,53.3126863183886));
#45702=CARTESIAN_POINT('Ctrl Pts',(69.1860094178192,273.732634297757,48.990055834104));
#45703=CARTESIAN_POINT('Ctrl Pts',(74.1148048310027,273.202244273876,45.4957534113066));
#45704=CARTESIAN_POINT('Ctrl Pts',(80.8542399341408,272.565776245219,48.2273408257238));
#45705=CARTESIAN_POINT('Ctrl Pts',(82.1891986104981,271.929308216562,55.361516546222));
#45706=CARTESIAN_POINT('Ctrl Pts',(76.917236919249,271.292840187905,60.3500030706631));
#45707=CARTESIAN_POINT('Ctrl Pts',(69.8588392120054,270.656372159248,58.6005525516741));
#45708=CARTESIAN_POINT('Ctrl Pts',(67.9236461013498,270.125982135367,52.8770744769839));
#45709=CARTESIAN_POINT('Ctrl Pts',(69.7762207730987,269.701670116262,48.8802797388908));
#45710=CARTESIAN_POINT('Ctrl Pts',(73.2518895769041,269.277358097158,46.1735977370467));
#45711=CARTESIAN_POINT('Ctrl Pts',(79.2644284747478,268.746968073277,46.7673566518502));
#45712=CARTESIAN_POINT('Ctrl Pts',(82.5615066218131,268.11050004462,53.2489329265036));
#45713=CARTESIAN_POINT('Ctrl Pts',(78.891319649359,267.474032015963,59.5105864993037));
#45714=CARTESIAN_POINT('Ctrl Pts',(71.6399130646353,266.837563987306,59.8199090195935));
#45715=CARTESIAN_POINT('Ctrl Pts',(67.4580045253141,266.201095958649,53.8706908961121));
#45716=CARTESIAN_POINT('Ctrl Pts',(69.7499824125412,265.670705934768,48.2805199674685));
#45717=CARTESIAN_POINT('Ctrl Pts',(73.7694808477695,265.246393915664,46.4777350601514));
#45718=CARTESIAN_POINT('Ctrl Pts',(78.1684483448451,264.822081896559,46.7132898362162));
#45719=CARTESIAN_POINT('Ctrl Pts',(82.3185553137515,264.291691872679,51.1041651240854));
#45720=CARTESIAN_POINT('Ctrl Pts',(80.5576910193728,263.655223844021,58.1597240848477));
#45721=CARTESIAN_POINT('Ctrl Pts',(73.6807691535739,263.018755815364,60.4806126065627));
#45722=CARTESIAN_POINT('Ctrl Pts',(68.0031447158811,262.382287786708,55.959201474732));
#45723=CARTESIAN_POINT('Ctrl Pts',(68.746882336194,261.74581975805,48.7253636507177));
#45724=CARTESIAN_POINT('Ctrl Pts',(74.1429501045604,261.21542973417,46.0077127742825));
#45725=CARTESIAN_POINT('Ctrl Pts',(78.3597971094831,260.791117715065,47.2823117033291));
#45726=CARTESIAN_POINT('Ctrl Pts',(81.5265462869171,260.36680569596,50.3446801886808));
#45727=CARTESIAN_POINT('Ctrl Pts',(81.7806472705137,259.83641567208,56.3811200614141));
#45728=CARTESIAN_POINT('Ctrl Pts',(75.8246732213346,259.199947643423,60.5534010248098));
#45729=CARTESIAN_POINT('Ctrl Pts',(69.1107440375934,258.563479614766,57.7962770170366));
#45730=CARTESIAN_POINT('Ctrl Pts',(67.7889673285718,257.927011586109,50.6596472655351));
#45731=CARTESIAN_POINT('Ctrl Pts',(73.0939157961889,257.290543557452,45.6858079971291));
#45732=CARTESIAN_POINT('Ctrl Pts',(78.9499721002604,256.760153533571,47.1723402741198));
#45733=CARTESIAN_POINT('Ctrl Pts',(81.2978906528269,256.335841514467,50.8997629176322));
#45734=CARTESIAN_POINT('Ctrl Pts',(81.6806978999942,255.911529495362,55.2883685850816));
#45735=CARTESIAN_POINT('Ctrl Pts',(77.9142820912556,255.381139471482,60.0124860267495));
#45736=CARTESIAN_POINT('Ctrl Pts',(70.6816566300579,254.744671442824,59.2570495634751));
#45737=CARTESIAN_POINT('Ctrl Pts',(67.4205804396085,254.108203414168,52.7729181676277));
#45738=CARTESIAN_POINT('Ctrl Pts',(71.1023289393623,253.47173538551,46.5180555901532));
#45739=CARTESIAN_POINT('Ctrl Pts',(78.3690358413775,252.835267356853,46.2414220560095));
#45740=CARTESIAN_POINT('Ctrl Pts',(81.8155825545176,252.304877332973,51.2037289188641));
#45741=CARTESIAN_POINT('Ctrl Pts',(81.1440803202529,251.880565313868,55.557518744089));
#45742=CARTESIAN_POINT('Ctrl Pts',(78.555368089813,251.456253294763,59.1219219312753));
#45743=CARTESIAN_POINT('Ctrl Pts',(72.613998875791,250.925863270883,60.218874760553));
#45744=CARTESIAN_POINT('Ctrl Pts',(67.6487461946136,250.289395242226,54.9058886769958));
#45745=CARTESIAN_POINT('Ctrl Pts',(69.4384673363466,249.652927213568,47.8720080899112));
#45746=CARTESIAN_POINT('Ctrl Pts',(76.3196650807418,249.016459184912,45.5638279667278));
#45747=CARTESIAN_POINT('Ctrl Pts',(81.9874061413906,248.379991156254,50.1199520411405));
#45748=CARTESIAN_POINT('Ctrl Pts',(81.3356174014151,247.849601132374,56.1264772500639));
#45749=CARTESIAN_POINT('Ctrl Pts',(77.9737339767994,247.425289113269,58.9732545388849));
#45750=CARTESIAN_POINT('Ctrl Pts',(73.6819847610538,247.000977094165,59.9668790967541));
#45751=CARTESIAN_POINT('Ctrl Pts',(68.4769640391432,246.470587070284,56.8991547070032));
#45752=CARTESIAN_POINT('Ctrl Pts',(68.2120838441216,245.834119041627,49.6320098897938));
#45753=CARTESIAN_POINT('Ctrl Pts',(74.1756296257088,245.19765101297,45.4950182787986));
#45754=CARTESIAN_POINT('Ctrl Pts',(80.8844538365335,244.561182984313,48.2645409067584));
#45755=CARTESIAN_POINT('Ctrl Pts',(82.176006380466,243.924714955656,55.4208980343947));
#45756=CARTESIAN_POINT('Ctrl Pts',(77.7452620688528,243.394324931776,59.5284129147206));
#45757=CARTESIAN_POINT('Ctrl Pts',(73.3403378631987,242.970012912671,59.4732419504946));
#45758=CARTESIAN_POINT('Ctrl Pts',(69.4485311580947,242.545700893566,57.4092066642255));
#45759=CARTESIAN_POINT('Ctrl Pts',(67.5303462247113,242.015310869685,51.6800060037207));
#45760=CARTESIAN_POINT('Ctrl Pts',(72.0956311926795,241.378842841029,46.0196413093522));
#45761=CARTESIAN_POINT('Ctrl Pts',(79.310833082975,240.742374812371,46.80668613705));
#45762=CARTESIAN_POINT('Ctrl Pts',(82.5599249123451,240.105906783714,53.2968309861926));
#45763=CARTESIAN_POINT('Ctrl Pts',(78.8424214579609,239.469438755058,59.5467688561755));
#45764=CARTESIAN_POINT('Ctrl Pts',(72.8038093924522,238.939048731177,59.7425696970413));
#45765=CARTESIAN_POINT('Ctrl Pts',(69.514280236937,238.514736712072,56.8124845399393));
#45766=CARTESIAN_POINT('Ctrl Pts',(67.9294216226235,238.090424692967,52.7021774631518));
#45767=CARTESIAN_POINT('Ctrl Pts',(70.2379930979051,237.560034669087,47.1188387316663));
#45768=CARTESIAN_POINT('Ctrl Pts',(77.3964297879165,236.92356664043,45.8388623775458));
#45769=CARTESIAN_POINT('Ctrl Pts',(82.3278012354823,236.287098611773,51.1642875741535));
#45770=CARTESIAN_POINT('Ctrl Pts',(80.5250887439314,235.650630583116,58.1948498241683));
#45771=CARTESIAN_POINT('Ctrl Pts',(73.6201253695851,235.014162554459,60.4758662885864));
#45772=CARTESIAN_POINT('Ctrl Pts',(68.9325969518973,234.483772530578,56.6640096569224));
#45773=CARTESIAN_POINT('Ctrl Pts',(68.3703492866676,234.059460511474,52.2947673134723));
#45774=CARTESIAN_POINT('Ctrl Pts',(69.8690277487388,233.635148492369,48.1522603478558));
#45775=CARTESIAN_POINT('Ctrl Pts',(75.2731435712621,233.104758468489,45.4506486393164));
#45776=CARTESIAN_POINT('Ctrl Pts',(81.5170606760362,232.468290439831,49.1782557136697));
#45777=CARTESIAN_POINT('Ctrl Pts',(81.74820395588,231.831822411175,56.4325751622959));
#45778=CARTESIAN_POINT('Ctrl Pts',(75.777025664907,231.195354382517,60.5585426483244));
#45779=CARTESIAN_POINT('Ctrl Pts',(69.0680704313891,230.558886353861,57.7529277447718));
#45780=CARTESIAN_POINT('Ctrl Pts',(68.0285390303481,230.028496329979,51.8012432678224));
#45781=CARTESIAN_POINT('Ctrl Pts',(70.4690771432479,229.604184310875,48.1337952706548));
#45782=CARTESIAN_POINT('Ctrl Pts',(74.3169324202657,229.17987229177,45.9889384313317));
#45783=CARTESIAN_POINT('Ctrl Pts',(80.1685476557545,228.64948226789,47.4928575710618));
#45784=CARTESIAN_POINT('Ctrl Pts',(82.438393234342,228.013014239233,54.4015011690346));
#45785=CARTESIAN_POINT('Ctrl Pts',(77.8560469329069,227.376546210576,60.0300605107207));
#45786=CARTESIAN_POINT('Ctrl Pts',(70.6423113450935,226.740078181919,59.2296876487903));
#45787=CARTESIAN_POINT('Ctrl Pts',(67.4167872981172,226.103610153262,52.7122073106552));
#45788=CARTESIAN_POINT('Ctrl Pts',(70.5346287283472,225.573220129381,47.5370514181189));
#45789=CARTESIAN_POINT('Ctrl Pts',(74.7820762065753,225.148908110276,46.3684664110055));
#45790=CARTESIAN_POINT('Ctrl Pts',(79.0936391685144,224.724596091172,47.2722507331135));
#45791=CARTESIAN_POINT('Ctrl Pts',(82.5254317902303,224.194206067291,52.2447725022218));
#45792=CARTESIAN_POINT('Ctrl Pts',(79.7089697578622,223.557738038634,58.94918123044));
#45793=CARTESIAN_POINT('Ctrl Pts',(72.5585073072376,222.921270009977,60.1939570431606));
#45794=CARTESIAN_POINT('Ctrl Pts',(67.6369827609765,222.28480198132,54.8594306967786));
#45795=CARTESIAN_POINT('Ctrl Pts',(69.4754129514866,221.648333952663,47.8236843010338));
#45796=CARTESIAN_POINT('Ctrl Pts',(75.2228696622896,221.117943928782,45.9609103224261));
#45797=CARTESIAN_POINT('Ctrl Pts',(79.1959535942427,220.693631909678,47.8638011191713));
#45798=CARTESIAN_POINT('Ctrl Pts',(81.8585388479515,220.269319890573,51.3733674413462));
#45799=CARTESIAN_POINT('Ctrl Pts',(81.1889060619244,219.738929866692,57.3779305317796));
#45800=CARTESIAN_POINT('Ctrl Pts',(74.6662293605485,219.102461838036,60.5929086255491));
#45801=CARTESIAN_POINT('Ctrl Pts',(68.4513936313183,218.465993809378,56.8439552027099));
#45802=CARTESIAN_POINT('Ctrl Pts',(68.2336921254748,217.829525780721,49.5892193551519));
#45803=CARTESIAN_POINT('Ctrl Pts',(74.2351594197245,217.193057752065,45.4827627314684));
#45804=CARTESIAN_POINT('Ctrl Pts',(79.7960878518984,216.662667728184,47.8451334079548));
#45805=CARTESIAN_POINT('Ctrl Pts',(81.5477681874052,216.238355709079,51.8870828353502));
#45806=CARTESIAN_POINT('Ctrl Pts',(81.257103920335,215.814043689975,56.2827072143604));
#45807=CARTESIAN_POINT('Ctrl Pts',(76.8132641208564,215.283653666094,60.3770845603876));
#45808=CARTESIAN_POINT('Ctrl Pts',(69.7821658351079,214.647185637437,58.5272029458524));
#45809=CARTESIAN_POINT('Ctrl Pts',(67.5453429981363,214.01071760878,51.6216558681655));
#45810=CARTESIAN_POINT('Ctrl Pts',(72.1435593680832,213.374249580123,46.0013327700207));
#45811=CARTESIAN_POINT('Ctrl Pts',(79.3569958438914,212.737781551466,46.8367726073938));
#45812=CARTESIAN_POINT('Ctrl Pts',(82.5569693436358,212.101313522809,53.3521487628495));
#45813=CARTESIAN_POINT('Ctrl Pts',(78.7957165783259,211.464845494152,59.5739959746584));
#45814=CARTESIAN_POINT('Ctrl Pts',(72.7551636611878,210.934455470271,59.7268307558592));
#45815=CARTESIAN_POINT('Ctrl Pts',(69.4871702856738,210.510143451167,56.772813373531));
#45816=CARTESIAN_POINT('Ctrl Pts',(67.9318512102494,210.085831432062,52.6513182873948));
#45817=CARTESIAN_POINT('Ctrl Pts',(70.2807526184919,209.555441408181,47.0846871324468));
#45818=CARTESIAN_POINT('Ctrl Pts',(77.4481799203683,208.918973379524,45.8564438509837));
#45819=CARTESIAN_POINT('Ctrl Pts',(82.3410297505945,208.282505350868,51.2172839626031));
#45820=CARTESIAN_POINT('Ctrl Pts',(80.4876226573618,207.64603732221,58.2346707308159));
#45821=CARTESIAN_POINT('Ctrl Pts',(73.5663904206805,207.009569293554,60.4658004491442));
#45822=CARTESIAN_POINT('Ctrl Pts',(68.906481682848,206.479179269673,56.6202268209065));
#45823=CARTESIAN_POINT('Ctrl Pts',(68.3757750274088,206.054867250568,52.2470396023114));
#45824=CARTESIAN_POINT('Ctrl Pts',(69.9043015957043,205.630555231463,48.1154544531592));
#45825=CARTESIAN_POINT('Ctrl Pts',(75.3277696890035,205.100165207583,45.4529031618409));
#45826=CARTESIAN_POINT('Ctrl Pts',(81.5446291154323,204.463697178925,49.2254635367899));
#45827=CARTESIAN_POINT('Ctrl Pts',(81.7234265711998,203.827229150269,56.4812616782425));
#45828=CARTESIAN_POINT('Ctrl Pts',(75.7226346705662,203.190761121611,60.5640397333196));
#45829=CARTESIAN_POINT('Ctrl Pts',(69.0340966790468,202.554293092955,57.7100925875615));
#45830=CARTESIAN_POINT('Ctrl Pts',(68.0375337913152,202.023903069074,51.7510628214405));
#45831=CARTESIAN_POINT('Ctrl Pts',(70.5044690880589,201.599591049969,48.1013187869457));
#45832=CARTESIAN_POINT('Ctrl Pts',(74.3676993763908,201.175279030865,45.9842801150092));
#45833=CARTESIAN_POINT('Ctrl Pts',(80.2083115098209,200.644889006984,47.5303795952959));
#45834=CARTESIAN_POINT('Ctrl Pts',(82.4282520384488,200.008420978327,54.4552203432806));
#45835=CARTESIAN_POINT('Ctrl Pts',(77.8054148727975,199.37195294967,60.0505714840824));
#45836=CARTESIAN_POINT('Ctrl Pts',(70.5976417472473,198.735484921013,59.1981722467762));
#45837=CARTESIAN_POINT('Ctrl Pts',(67.419225377324,198.099016892356,52.6575893450889));
#45838=CARTESIAN_POINT('Ctrl Pts',(70.5743244731881,197.568626868476,47.5050634268305));
#45839=CARTESIAN_POINT('Ctrl Pts',(74.8300927655731,197.144314849371,46.3671542320359));
#45840=CARTESIAN_POINT('Ctrl Pts',(79.1350226650609,196.720002830266,47.3020230211936));
#45841=CARTESIAN_POINT('Ctrl Pts',(82.5308491916423,196.189612806385,52.2991757953517));
#45842=CARTESIAN_POINT('Ctrl Pts',(79.6660879734873,195.553144777728,58.9830892055735));
#45843=CARTESIAN_POINT('Ctrl Pts',(72.5068307161614,194.916676749071,60.1762419207686));
#45844=CARTESIAN_POINT('Ctrl Pts',(67.6239226704089,194.280208720415,54.8063455628062));
#45845=CARTESIAN_POINT('Ctrl Pts',(69.5130685817726,193.643740691757,47.7840465775991));
#45846=CARTESIAN_POINT('Ctrl Pts',(75.2738146162295,193.113350667877,45.9627891072083));
#45847=CARTESIAN_POINT('Ctrl Pts',(79.2330672642372,192.689038648772,47.8942961773743));
#45848=CARTESIAN_POINT('Ctrl Pts',(81.8702586670936,192.264726629668,51.4229818530266));
#45849=CARTESIAN_POINT('Ctrl Pts',(81.1573268859826,191.734336605787,57.4225569981905));
#45850=CARTESIAN_POINT('Ctrl Pts',(74.6116118538668,191.09786857713,60.590390647602));
#45851=CARTESIAN_POINT('Ctrl Pts',(68.4240078959387,190.461400548473,56.7966938834467));
#45852=CARTESIAN_POINT('Ctrl Pts',(68.2586153345421,189.824932519816,49.5405776234103));
#45853=CARTESIAN_POINT('Ctrl Pts',(74.2896321797345,189.188464491159,45.4775256762879));
#45854=CARTESIAN_POINT('Ctrl Pts',(79.8332295550212,188.658074467278,47.8799623118115));
#45855=CARTESIAN_POINT('Ctrl Pts',(81.555912114883,188.233762448174,51.934437110204));
#45856=CARTESIAN_POINT('Ctrl Pts',(81.2331274814595,187.809450429069,56.3278652902565));
#45857=CARTESIAN_POINT('Ctrl Pts',(76.7607776831728,187.279060405188,60.3900396992102));
#45858=CARTESIAN_POINT('Ctrl Pts',(69.7415433368246,186.642592376531,58.4895385802815));
#45859=CARTESIAN_POINT('Ctrl Pts',(67.5575508842565,186.006124347874,51.567923534235));
#45860=CARTESIAN_POINT('Ctrl Pts',(72.190717024769,185.369656319217,45.9811221780975));
#45861=CARTESIAN_POINT('Ctrl Pts',(79.4083750996385,184.73318829056,46.8682339107886));
#45862=CARTESIAN_POINT('Ctrl Pts',(82.0184321936041,184.20279826668,52.3171581728088));
#45863=CARTESIAN_POINT('Ctrl Pts',(80.6604212276972,183.778486247575,56.5078869053));
#45864=CARTESIAN_POINT('Ctrl Pts',(77.5358267115987,183.35417422847,59.6132548710689));
#45865=CARTESIAN_POINT('Ctrl Pts',(71.4955336193098,182.82378420459,59.7475419003588));
#45866=CARTESIAN_POINT('Ctrl Pts',(67.4422413917183,182.187316175932,53.7099614719295));
#45867=CARTESIAN_POINT('Ctrl Pts',(70.3320281351587,181.550848147276,47.052055610777));
#45868=CARTESIAN_POINT('Ctrl Pts',(77.493477408106,180.914380118619,45.8721309566008));
#45869=CARTESIAN_POINT('Ctrl Pts',(82.3610866179652,180.277912089962,51.2747169940557));
#45870=CARTESIAN_POINT('Ctrl Pts',(80.7586618438728,179.747522066081,57.1001275796167));
#45871=CARTESIAN_POINT('Ctrl Pts',(76.985389807126,179.323210046977,59.3736313138467));
#45872=CARTESIAN_POINT('Ctrl Pts',(72.590053015099,178.898898027871,59.6692925685079));
#45873=CARTESIAN_POINT('Ctrl Pts',(67.9415917424124,178.368508003991,55.8098908735143));
#45874=CARTESIAN_POINT('Ctrl Pts',(68.8403759618455,177.732039975334,48.5936770297519));
#45875=CARTESIAN_POINT('Ctrl Pts',(75.3879313276058,177.095571946677,45.4618889445139));
#45876=CARTESIAN_POINT('Ctrl Pts',(81.5685162443548,176.45910391802,49.2670102258116));
#45877=CARTESIAN_POINT('Ctrl Pts',(81.7009226931967,175.822635889363,56.5377752367517));
#45878=CARTESIAN_POINT('Ctrl Pts',(76.6712125465343,175.292245865482,59.8851905810956));
#45879=CARTESIAN_POINT('Ctrl Pts',(72.3316024134768,174.867933846378,59.1274406316263));
#45880=CARTESIAN_POINT('Ctrl Pts',(68.8192612940262,174.443621827273,56.4685196186083));
#45881=CARTESIAN_POINT('Ctrl Pts',(67.8404021049406,173.913231803392,50.5065561555424));
#45882=CARTESIAN_POINT('Ctrl Pts',(73.2508538169764,173.276763774735,45.6476913103612));
#45883=CARTESIAN_POINT('Ctrl Pts',(80.247841532224,172.640295746078,47.5766134941744));
#45884=CARTESIAN_POINT('Ctrl Pts',(82.4190432536031,172.003827717421,54.5022514405018));
#45885=CARTESIAN_POINT('Ctrl Pts',(77.751367091034,171.367359688765,60.0784826546278));
#45886=CARTESIAN_POINT('Ctrl Pts',(71.758955772151,170.836969664884,59.307651783222));
#45887=CARTESIAN_POINT('Ctrl Pts',(68.9794391377946,170.412657645779,55.8899495767404));
#45888=CARTESIAN_POINT('Ctrl Pts',(68.0711591552949,169.988345626674,51.5793314579269));
#45889=CARTESIAN_POINT('Ctrl Pts',(71.2415481569305,169.457955602794,46.4361994136081));
#45890=CARTESIAN_POINT('Ctrl Pts',(78.5125178087286,168.821487574137,46.3155526787233));
#45891=CARTESIAN_POINT('Ctrl Pts',(82.530377405723,168.18501954548,52.360003202747));
#45892=CARTESIAN_POINT('Ctrl Pts',(79.6282957660669,167.548551516823,59.0125591052029));
#45893=CARTESIAN_POINT('Ctrl Pts',(72.4477226523281,166.912083488166,60.1618741491581));
#45894=CARTESIAN_POINT('Ctrl Pts',(68.4289229561712,166.381693464285,55.650508208652));
#45895=CARTESIAN_POINT('Ctrl Pts',(68.5714774657263,165.957381445181,51.2475456486637));
#45896=CARTESIAN_POINT('Ctrl Pts',(70.7123205480204,165.533069426076,47.3974557809012));
#45897=CARTESIAN_POINT('Ctrl Pts',(76.4784505969129,165.002679402195,45.5933166769935));
#45898=CARTESIAN_POINT('Ctrl Pts',(82.0471251430861,164.366211373538,50.2700055816363));
#45899=CARTESIAN_POINT('Ctrl Pts',(81.1170844673234,163.729743344881,57.4681721690361));
#45900=CARTESIAN_POINT('Ctrl Pts',(74.5637546035804,163.093275316224,60.5878589442599));
#45901=CARTESIAN_POINT('Ctrl Pts',(68.3888028090185,162.456807287567,56.7470874531606));
#45902=CARTESIAN_POINT('Ctrl Pts',(68.3128475435835,161.926417263686,50.7057792798719));
#45903=CARTESIAN_POINT('Ctrl Pts',(71.3076207439878,161.502105244582,47.475030980949));
#45904=CARTESIAN_POINT('Ctrl Pts',(75.4485626168732,161.077793225477,45.9720334765473));
#45905=CARTESIAN_POINT('Ctrl Pts',(80.9849999203633,160.547403201597,48.3909248820298));
#45906=CARTESIAN_POINT('Ctrl Pts',(82.1226997942578,159.910935172939,55.5733474753437));
#45907=CARTESIAN_POINT('Ctrl Pts',(76.700483626755,159.274467144283,60.3980909619345));
#45908=CARTESIAN_POINT('Ctrl Pts',(69.7070713458812,158.637999115625,58.4562458218015));
#45909=CARTESIAN_POINT('Ctrl Pts',(67.5634994504208,158.001531086969,51.5073858547998));
#45910=CARTESIAN_POINT('Ctrl Pts',(71.4676070918562,157.471141063088,46.8964079573167));
#45911=CARTESIAN_POINT('Ctrl Pts',(75.8471444980346,157.046829043983,46.4209574333503));
#45912=CARTESIAN_POINT('Ctrl Pts',(79.9591020499818,156.622517024879,48.0015289071645));
#45913=CARTESIAN_POINT('Ctrl Pts',(82.5529634584382,156.092127000998,53.4581814195306));
#45914=CARTESIAN_POINT('Ctrl Pts',(78.7022097890694,155.455658972341,59.6269131765332));
#45915=CARTESIAN_POINT('Ctrl Pts',(71.4447323271936,154.819190943684,59.714084094242));
#45916=CARTESIAN_POINT('Ctrl Pts',(67.438046115442,154.182722915027,53.6622212835787));
#45917=CARTESIAN_POINT('Ctrl Pts',(70.3762155259669,153.54625488637,47.0102504608026));
#45918=CARTESIAN_POINT('Ctrl Pts',(76.3473529711757,153.015864862489,46.0890060538096));
#45919=CARTESIAN_POINT('Ctrl Pts',(79.9656584160781,152.591552843385,48.6018265408803));
#45920=CARTESIAN_POINT('Ctrl Pts',(82.0337510039629,152.16724082428,52.4914787285174));
#45921=CARTESIAN_POINT('Ctrl Pts',(80.4140309010038,151.636850800399,58.3121041618417));
#45922=CARTESIAN_POINT('Ctrl Pts',(73.4617130669307,151.000382771742,60.4444343534476));
#45923=CARTESIAN_POINT('Ctrl Pts',(67.9251761126493,150.363914743085,55.7513184980263));
#45924=CARTESIAN_POINT('Ctrl Pts',(68.8685131074888,149.727446714428,48.5548823527737));
#45925=CARTESIAN_POINT('Ctrl Pts',(75.4487054911373,149.090978685771,45.4593010654896));
#45926=CARTESIAN_POINT('Ctrl Pts',(80.5609842542104,148.560588661891,48.6792047124364));
#45927=CARTESIAN_POINT('Ctrl Pts',(81.6450692014175,148.136276642786,52.9490010682467));
#45928=CARTESIAN_POINT('Ctrl Pts',(80.6559206726707,147.711964623682,57.2417841143524));
#45929=CARTESIAN_POINT('Ctrl Pts',(75.6162903551188,147.1815745998,60.5742456534258));
#45930=CARTESIAN_POINT('Ctrl Pts',(68.9690803493656,146.545106571144,57.6253213662624));
#45931=CARTESIAN_POINT('Ctrl Pts',(67.8664158817172,145.908638542487,50.4515699801105));
#45932=CARTESIAN_POINT('Ctrl Pts',(73.2975360364468,145.27217051383,45.6368517387779));
#45933=CARTESIAN_POINT('Ctrl Pts',(80.2954228114288,144.635702485173,47.6145109603169));
#45934=CARTESIAN_POINT('Ctrl Pts',(82.0437996394039,144.105312461292,53.3977930833325));
#45935=CARTESIAN_POINT('Ctrl Pts',(80.0624568115943,143.681000442187,57.3323428277813));
#45936=CARTESIAN_POINT('Ctrl Pts',(76.5007551034253,143.256688423083,59.92477065414));
#45937=CARTESIAN_POINT('Ctrl Pts',(70.5106597070975,142.726298399202,59.1361447669926));
#45938=CARTESIAN_POINT('Ctrl Pts',(67.4257250957628,142.089830370545,52.550954279558));
#45939=CARTESIAN_POINT('Ctrl Pts',(71.297244453972,141.453362341888,46.4117429509309));
#45940=CARTESIAN_POINT('Ctrl Pts',(78.5548705710514,140.816894313231,46.3379796591357));
#45941=CARTESIAN_POINT('Ctrl Pts',(82.5414507256682,140.180426284574,52.4198160580224));
#45942=CARTESIAN_POINT('Ctrl Pts',(80.0692118555573,139.650036260693,57.9326382586836));
#45943=CARTESIAN_POINT('Ctrl Pts',(75.9933095704882,139.225724241589,59.6039914994505));
#45944=CARTESIAN_POINT('Ctrl Pts',(71.6043070931456,138.801412222484,59.2257609523848));
#45945=CARTESIAN_POINT('Ctrl Pts',(67.5989245988587,138.271022198604,54.7024784361751));
#45946=CARTESIAN_POINT('Ctrl Pts',(69.5878994285397,137.634554169946,47.7077994271777));
#45947=CARTESIAN_POINT('Ctrl Pts',(76.5365379382289,136.99808614129,45.6113737213163));
#45948=CARTESIAN_POINT('Ctrl Pts',(82.0643953738658,136.361618112632,50.3147097766925));
#45949=CARTESIAN_POINT('Ctrl Pts',(81.0862238434915,135.725150083976,57.5205918024526));
#45950=CARTESIAN_POINT('Ctrl Pts',(75.6047792136601,135.194760060095,60.0616424546605));
#45951=CARTESIAN_POINT('Ctrl Pts',(71.4315308456683,134.77044804099,58.6508273881453));
#45952=CARTESIAN_POINT('Ctrl Pts',(68.3658617004297,134.346136021886,55.4872734080804));
#45953=CARTESIAN_POINT('Ctrl Pts',(68.3078504172972,133.815745998005,49.4457662833621));
#45954=CARTESIAN_POINT('Ctrl Pts',(74.3961266495209,133.179277969348,45.4690279424416));
#45955=CARTESIAN_POINT('Ctrl Pts',(81.0170152058,132.542809940691,48.442647387472));
#45956=CARTESIAN_POINT('Ctrl Pts',(82.1064249903531,131.906341912034,55.6184235963466));
#45957=CARTESIAN_POINT('Ctrl Pts',(76.6428109257527,131.269873883377,60.4174314797647));
#45958=CARTESIAN_POINT('Ctrl Pts',(70.8380969889688,130.739483859496,58.7415825130923));
#45959=CARTESIAN_POINT('Ctrl Pts',(68.6124160006545,130.315171840392,54.9399058788808));
#45960=CARTESIAN_POINT('Ctrl Pts',(68.3722740552658,129.890859821287,50.5411864130682));
#45961=CARTESIAN_POINT('Ctrl Pts',(72.2900598145347,129.360469797406,45.941824675668));
#45962=CARTESIAN_POINT('Ctrl Pts',(79.4943503469096,128.724001768749,46.9316495274165));
#45963=CARTESIAN_POINT('Ctrl Pts',(82.5432190311814,128.087533740092,53.5182250887076));
#45964=CARTESIAN_POINT('Ctrl Pts',(78.6603646892618,127.451065711435,59.6502736891323));
#45965=CARTESIAN_POINT('Ctrl Pts',(71.3885074732591,126.814597682778,59.6908685418939));
#45966=CARTESIAN_POINT('Ctrl Pts',(68.1048643284523,126.284207658898,54.6192946890791));
#45967=CARTESIAN_POINT('Ctrl Pts',(68.9173460103732,125.859895639793,50.28959786258));
#45968=CARTESIAN_POINT('Ctrl Pts',(71.6204020703455,125.435583620688,46.8111083873192));
#45969=CARTESIAN_POINT('Ctrl Pts',(77.5942494198532,124.905193596808,45.9076032729058));
#45970=CARTESIAN_POINT('Ctrl Pts',(82.3844143232222,124.268725568151,51.3789719783156));
#45971=CARTESIAN_POINT('Ctrl Pts',(80.3673015812238,123.632257539494,58.3510472837465));
#45972=CARTESIAN_POINT('Ctrl Pts',(73.4148019883362,122.995789510837,60.4346324846513));
#45973=CARTESIAN_POINT('Ctrl Pts',(67.8979495774062,122.35932148218,55.6969226172128));
#45974=CARTESIAN_POINT('Ctrl Pts',(68.7443794887827,121.828931458299,49.7147215129271));
#45975=CARTESIAN_POINT('Ctrl Pts',(72.19690357994,121.404619439194,46.978578517243));
#45976=CARTESIAN_POINT('Ctrl Pts',(76.5186460802307,120.98030742009,46.1247970147295));
#45977=CARTESIAN_POINT('Ctrl Pts',(81.6213386668304,120.449917396209,49.3598707408833));
#45978=CARTESIAN_POINT('Ctrl Pts',(81.6501721592166,119.813449367552,56.6317841026972));
#45979=CARTESIAN_POINT('Ctrl Pts',(75.5554737531873,119.176981338895,60.5730058952479));
#45980=CARTESIAN_POINT('Ctrl Pts',(68.9400899651232,118.540513310238,57.5871600828947));
#45981=CARTESIAN_POINT('Ctrl Pts',(67.8815288094136,117.904045281581,50.3926480360889));
#45982=CARTESIAN_POINT('Ctrl Pts',(72.4432767065111,117.3736552577,46.431129416883));
#45983=CARTESIAN_POINT('Ctrl Pts',(76.8440883983223,116.949343238596,46.6292645880943));
#45984=CARTESIAN_POINT('Ctrl Pts',(80.6668409771502,116.525031219491,48.8185484467835));
#45985=CARTESIAN_POINT('Ctrl Pts',(82.3980328243406,115.99464119561,54.6069980177146));
#45986=CARTESIAN_POINT('Ctrl Pts',(77.6514063441161,115.358173166953,60.1161805677161));
#45987=CARTESIAN_POINT('Ctrl Pts',(70.4655562751022,114.721705138296,59.095329616704));
#45988=CARTESIAN_POINT('Ctrl Pts',(67.4288608453278,114.085237109639,52.5031328094692));
#45989=CARTESIAN_POINT('Ctrl Pts',(71.3472914312269,113.448769080983,46.3771670035329));
#45990=CARTESIAN_POINT('Ctrl Pts',(77.3890770562702,112.918379057102,46.3774956509925));
#45991=CARTESIAN_POINT('Ctrl Pts',(80.5817556707862,112.494067037997,49.4128217219879));
#45992=CARTESIAN_POINT('Ctrl Pts',(82.0323496299757,112.069755018893,53.5724104346394));
#45993=CARTESIAN_POINT('Ctrl Pts',(79.5437477049679,111.539364995012,59.0778653754993));
#45994=CARTESIAN_POINT('Ctrl Pts',(72.3475329797288,110.902896966355,60.1247889353924));
#45995=CARTESIAN_POINT('Ctrl Pts',(67.5916352536787,110.266428937698,54.6420875302564));
#45996=CARTESIAN_POINT('Ctrl Pts',(69.6216247782731,109.629960909041,47.6737505400865));
#45997=CARTESIAN_POINT('Ctrl Pts',(76.5969956852068,108.993492880384,45.6180861650704));
#45998=CARTESIAN_POINT('Ctrl Pts',(81.1583125757584,108.463102856503,49.5801010402264));
#45999=CARTESIAN_POINT('Ctrl Pts',(81.5784289429698,108.038790837399,53.9652924078702));
#46000=CARTESIAN_POINT('Ctrl Pts',(79.9460656780891,107.614478818294,58.0569658142309));
#46001=CARTESIAN_POINT('Ctrl Pts',(74.4570979014776,107.084088794413,60.5817244946414));
#46002=CARTESIAN_POINT('Ctrl Pts',(68.3374776727713,106.447620765756,56.6533910606747));
#46003=CARTESIAN_POINT('Ctrl Pts',(68.3419469760824,105.811152737099,49.3953914806349));
#46004=CARTESIAN_POINT('Ctrl Pts',(74.4439160021854,105.174684708442,45.4654357705778));
#46005=CARTESIAN_POINT('Ctrl Pts',(81.0582591112123,104.538216679785,48.487359089935));
#46006=CARTESIAN_POINT('Ctrl Pts',(81.904038204952,104.007826655905,54.4696522431987));
#46007=CARTESIAN_POINT('Ctrl Pts',(79.3457331141397,103.5835146368,58.0559422698385));
#46008=CARTESIAN_POINT('Ctrl Pts',(75.4302791372836,103.159202617695,60.0747590638976));
#46009=CARTESIAN_POINT('Ctrl Pts',(69.6305683429886,102.628812593814,58.3816765645705));
#46010=CARTESIAN_POINT('Ctrl Pts',(67.586188434933,101.992344565158,51.4029900045114));
#46011=CARTESIAN_POINT('Ctrl Pts',(72.3488347856765,101.355876536501,45.9261498921585));
#46012=CARTESIAN_POINT('Ctrl Pts',(79.5327866704922,100.719408507844,46.9602742537252));
#46013=CARTESIAN_POINT('Ctrl Pts',(82.5450393663006,100.082940479187,53.5790270825144));
#46014=CARTESIAN_POINT('Ctrl Pts',(79.2608444968025,99.552550455306,58.6502436728556));
#46015=CARTESIAN_POINT('Ctrl Pts',(74.9777007832863,99.1282384362012,59.6803315439721));
#46016=CARTESIAN_POINT('Ctrl Pts',(70.6977489610756,98.7039264170968,58.6370609690939));
#46017=CARTESIAN_POINT('Ctrl Pts',(67.4291836821179,98.1735363932157,53.5557565436354));
#46018=CARTESIAN_POINT('Ctrl Pts',(70.4618009105109,97.537068364559,46.9463096637473));
#46019=CARTESIAN_POINT('Ctrl Pts',(77.6489027609979,96.900600335902,45.9343092342729));
#46020=CARTESIAN_POINT('Ctrl Pts',(82.3946636187328,96.2641323072451,51.4257873376363));
#46021=CARTESIAN_POINT('Ctrl Pts',(80.3288063723495,95.6276642785881,58.3981462748664));
#46022=CARTESIAN_POINT('Ctrl Pts',(74.5239101517951,95.0972742547074,60.0733637280889));
#46023=CARTESIAN_POINT('Ctrl Pts',(70.6146905705551,94.6729622356027,58.0425010152246));
#46024=CARTESIAN_POINT('Ctrl Pts',(68.0674396145845,94.248650216498,54.4483510934541));
#46025=CARTESIAN_POINT('Ctrl Pts',(68.9316338822774,93.7182601926173,48.4686904078737));
#46026=CARTESIAN_POINT('Ctrl Pts',(75.555249990983,93.0817921639603,45.467146645657));
#46027=CARTESIAN_POINT('Ctrl Pts',(81.6450899558155,92.4453241353034,49.4158713867934));
#46028=CARTESIAN_POINT('Ctrl Pts',(81.627212218408,91.8088561066465,56.6738503248336));
#46029=CARTESIAN_POINT('Ctrl Pts',(75.4955258534093,91.1723880779895,60.5833231324249));
#46030=CARTESIAN_POINT('Ctrl Pts',(70.0143577007266,90.6419980541087,58.0416761606747));
#46031=CARTESIAN_POINT('Ctrl Pts',(68.3946002320209,90.217686035004,53.9449961834947));
#46032=CARTESIAN_POINT('Ctrl Pts',(68.8282163938946,89.7933740158995,49.5611191189533));
#46033=CARTESIAN_POINT('Ctrl Pts',(73.4017105105445,89.2629839920186,45.6131670913877));
#46034=CARTESIAN_POINT('Ctrl Pts',(80.3707190660536,88.6265159633618,47.6902985425126));
#46035=CARTESIAN_POINT('Ctrl Pts',(82.3792438057071,87.9900479347048,54.6648527396444));
#46036=CARTESIAN_POINT('Ctrl Pts',(77.6064876577145,87.3535799060478,60.1328849844586));
#46037=CARTESIAN_POINT('Ctrl Pts',(70.4135304679223,86.7171118773909,59.0638095999201));
#46038=CARTESIAN_POINT('Ctrl Pts',(67.9418913606345,86.1867218535102,53.5507184733093));
#46039=CARTESIAN_POINT('Ctrl Pts',(69.4052856106959,85.7624098344054,49.3956157836349));
#46040=CARTESIAN_POINT('Ctrl Pts',(72.6072947099124,85.3380978153011,46.3701341985994));
#46041=CARTESIAN_POINT('Ctrl Pts',(78.649052708911,84.8077077914199,46.3884079099854));
#46042=CARTESIAN_POINT('Ctrl Pts',(82.5486031776573,84.1712397627633,52.5264093317599));
#46043=CARTESIAN_POINT('Ctrl Pts',(79.4916250958263,83.5347717341059,59.1092250580077));
#46044=CARTESIAN_POINT('Ctrl Pts',(72.3026659383084,82.8983037054495,60.1079462954285));
#46045=CARTESIAN_POINT('Ctrl Pts',(67.5730244559151,82.2618356767921,54.5841752321032));
#46046=CARTESIAN_POINT('Ctrl Pts',(69.3220304454764,81.7314456529117,48.8010833518486));
#46047=CARTESIAN_POINT('Ctrl Pts',(73.1515056005973,81.3071336338068,46.6235799352798));
#46048=CARTESIAN_POINT('Ctrl Pts',(77.552906480988,80.8828216147023,46.4389955834307));
#46049=CARTESIAN_POINT('Ctrl Pts',(82.1024354368033,80.3524315908214,50.4145408198967));
#46050=CARTESIAN_POINT('Ctrl Pts',(81.0217277540724,79.7159635621645,57.6057595077474));
#46051=CARTESIAN_POINT('Ctrl Pts',(74.3971820521111,79.0794955335075,60.5712227297676));
#46052=CARTESIAN_POINT('Ctrl Pts',(68.3146473605973,78.4430275048508,56.6112543454159));
#46053=CARTESIAN_POINT('Ctrl Pts',(68.3658705756886,77.8065594761935,49.3394642292037));
#46054=CARTESIAN_POINT('Ctrl Pts',(73.4784996066541,77.276169452313,46.1201167737832));
#46055=CARTESIAN_POINT('Ctrl Pts',(77.7975928712179,76.8518574332082,46.9872006594904));
#46056=CARTESIAN_POINT('Ctrl Pts',(81.2416761493576,76.4275454141037,49.7339608357872));
#46057=CARTESIAN_POINT('Ctrl Pts',(82.0696831491612,75.8971553902228,55.7187397001453));
#46058=CARTESIAN_POINT('Ctrl Pts',(76.5382697150696,75.2606873615659,60.4394409968975));
#46059=CARTESIAN_POINT('Ctrl Pts',(69.5922183320309,74.6242193329089,58.3344592718662));
#46060=CARTESIAN_POINT('Ctrl Pts',(67.5965818240238,73.987751304252,51.3562064241657));
#46061=CARTESIAN_POINT('Ctrl Pts',(72.4035700940913,73.351283275595,45.8996123322947));
#46062=CARTESIAN_POINT('Ctrl Pts',(78.3746072804039,72.8208932517143,46.8215063428315));
#46063=CARTESIAN_POINT('Ctrl Pts',(81.066940431951,72.3965812326096,50.3083019052256));
#46064=CARTESIAN_POINT('Ctrl Pts',(81.8660873416523,71.9722692135051,54.6404797997228));
#46065=CARTESIAN_POINT('Ctrl Pts',(78.5668446377229,71.4418791896242,59.7019194395446));
#46066=CARTESIAN_POINT('Ctrl Pts',(71.2951468796985,70.8054111609673,59.6389350926965));
#46067=CARTESIAN_POINT('Ctrl Pts',(67.4311912149224,70.1689431323103,53.4949604427505));
#46068=CARTESIAN_POINT('Ctrl Pts',(70.5003251860134,69.5324751036535,46.9178034166469));
#46069=CARTESIAN_POINT('Ctrl Pts',(77.7076291916687,68.8960070749964,45.9501649086956));
#46070=CARTESIAN_POINT('Ctrl Pts',(81.6112351748017,68.3656170511157,50.5615675126155));
#46071=CARTESIAN_POINT('Ctrl Pts',(81.357550929335,67.941305032011,54.9595267434923));
#46072=CARTESIAN_POINT('Ctrl Pts',(79.1201753175234,67.5169930129064,58.75433259683));
#46073=CARTESIAN_POINT('Ctrl Pts',(73.3103290393843,66.9866029890256,60.4123011946575));
#46074=CARTESIAN_POINT('Ctrl Pts',(67.8615167786614,66.3501349603686,55.5964938626097));
#46075=CARTESIAN_POINT('Ctrl Pts',(68.9730152573013,65.7136669317118,48.4241059052754));
#46076=CARTESIAN_POINT('Ctrl Pts',(75.6030280570083,65.0771989030548,45.4708859415329));
#46077=CARTESIAN_POINT('Ctrl Pts',(81.6790312514728,64.4407308743978,49.4663509323529));
#46078=CARTESIAN_POINT('Ctrl Pts',(81.6024187435134,63.9103408505171,55.507650806603));
#46079=CARTESIAN_POINT('Ctrl Pts',(78.5270237042011,63.4860288314123,58.6617507487461));
#46080=CARTESIAN_POINT('Ctrl Pts',(74.3494512879322,63.0617168123079,60.0597099039725));
#46081=CARTESIAN_POINT('Ctrl Pts',(68.8758564085409,62.5313267884269,57.5017942010431));
#46082=CARTESIAN_POINT('Ctrl Pts',(67.9198760668561,61.8948587597702,50.2929345895428));
#46083=CARTESIAN_POINT('Ctrl Pts',(73.4621886382343,61.2583907311131,45.6066408258451));
#46084=CARTESIAN_POINT('Ctrl Pts',(80.4043394211003,60.6219227024562,47.7244511068863));
#46085=CARTESIAN_POINT('Ctrl Pts',(82.3717685544846,59.9854546737992,54.7252209157801));
#46086=CARTESIAN_POINT('Ctrl Pts',(78.3524780838452,59.4550646499186,59.2361496183445));
#46087=CARTESIAN_POINT('Ctrl Pts',(73.9623318572474,59.0307526308137,59.6008648523837));
#46088=CARTESIAN_POINT('Ctrl Pts',(69.8915949053257,58.6064406117094,57.9169700334852));
#46089=CARTESIAN_POINT('Ctrl Pts',(67.4363414588,58.0760505878283,52.3965620630253));
#46090=CARTESIAN_POINT('Ctrl Pts',(71.4416283887399,57.4395825591715,46.3270289738281));
#46091=CARTESIAN_POINT('Ctrl Pts',(78.6989929913225,56.8031145305145,46.4231377856464));
#46092=CARTESIAN_POINT('Ctrl Pts',(82.5515916724324,56.1666465018575,52.5742402299928));
#46093=CARTESIAN_POINT('Ctrl Pts',(79.4463962098037,55.5301784732007,59.1499011436104));
#46094=CARTESIAN_POINT('Ctrl Pts',(73.4539010665363,54.9997884493199,59.9200800870426));
#46095=CARTESIAN_POINT('Ctrl Pts',(69.9001981970296,54.5754764302151,57.3166982464142));
#46096=CARTESIAN_POINT('Ctrl Pts',(67.9309790436144,54.1511644111106,53.3760666956756));
#46097=CARTESIAN_POINT('Ctrl Pts',(69.6971540221891,53.6207743872298,47.5981951505438));
#46098=CARTESIAN_POINT('Ctrl Pts',(76.7010967416689,52.9843063585729,45.6420914482174));
#46099=CARTESIAN_POINT('Ctrl Pts',(82.117366875131,52.3478383299159,50.4735090165814));
#46100=CARTESIAN_POINT('Ctrl Pts',(80.9926200105515,51.7113703012591,57.6438313502813));
#46101=CARTESIAN_POINT('Ctrl Pts',(74.3363619212952,51.0749022726018,60.572275230778));
#46102=CARTESIAN_POINT('Ctrl Pts',(69.3070159747315,50.5445122487213,57.2243127165354));
#46103=CARTESIAN_POINT('Ctrl Pts',(68.3310893999085,50.1202002296165,52.9285044790314));
#46104=CARTESIAN_POINT('Ctrl Pts',(69.4283156990817,49.695888210512,48.6620662055701));
#46105=CARTESIAN_POINT('Ctrl Pts',(74.5504841531635,49.1654981866311,45.4579182728111));
#46106=CARTESIAN_POINT('Ctrl Pts',(81.1211142061001,48.5290301579743,48.5737449720119));
#46107=CARTESIAN_POINT('Ctrl Pts',(82.0422892607611,47.8925621293172,55.7730514939763));
#46108=CARTESIAN_POINT('Ctrl Pts',(76.4913286793663,47.2560941006604,60.4490983823568));
#46109=CARTESIAN_POINT('Ctrl Pts',(69.545609137681,46.6196260720033,58.2953724573005));
#46110=CARTESIAN_POINT('Ctrl Pts',(67.9438181282235,46.0892360481227,52.4697875760198));
#46111=CARTESIAN_POINT('Ctrl Pts',(70.023876958922,45.664924029018,48.5865213794158));
#46112=CARTESIAN_POINT('Ctrl Pts',(73.6499021023712,45.2406120099134,46.0848533854706));
#46113=CARTESIAN_POINT('Ctrl Pts',(79.6181747788305,44.7102219860325,47.0244782608427));
#46114=CARTESIAN_POINT('Ctrl Pts',(82.5358491753481,44.0737539573756,53.6854640308254));
#46115=CARTESIAN_POINT('Ctrl Pts',(78.5105485707623,43.4372859287187,59.7249617683243));
#46116=CARTESIAN_POINT('Ctrl Pts',(71.2533739040916,42.8008179000617,59.6154458518454));
#46117=CARTESIAN_POINT('Ctrl Pts',(67.4216317053234,42.1643498714049,53.4348870555725));
#46118=CARTESIAN_POINT('Ctrl Pts',(70.0322815804837,41.6339598475239,47.9862467778226));
#46119=CARTESIAN_POINT('Ctrl Pts',(74.1490861427561,41.2096478284193,46.4183433085664));
#46120=CARTESIAN_POINT('Ctrl Pts',(78.527138901517,40.7853358093147,46.9072759566463));
#46121=CARTESIAN_POINT('Ctrl Pts',(82.4170310660717,40.254945785434,51.5302525513445));
#46122=CARTESIAN_POINT('Ctrl Pts',(80.2520741370471,39.618477756777,58.4724796297019));
#46123=CARTESIAN_POINT('Ctrl Pts',(73.2527161602415,38.9820097281201,60.3927831971243));
#46124=CARTESIAN_POINT('Ctrl Pts',(67.8453808390323,38.3455416994631,55.5513678459556));
#46125=CARTESIAN_POINT('Ctrl Pts',(69.0051896420068,37.7090736708062,48.372482218467));
#46126=CARTESIAN_POINT('Ctrl Pts',(74.5490483491708,37.1786836469254,45.970648693432));
#46127=CARTESIAN_POINT('Ctrl Pts',(78.6853429395574,36.7543716278208,47.4863888276205));
#46128=CARTESIAN_POINT('Ctrl Pts',(81.6701546315565,36.3300596087161,50.7263425705272));
#46129=CARTESIAN_POINT('Ctrl Pts',(81.5755988389129,35.7996695848354,56.7673882456549));
#46130=CARTESIAN_POINT('Ctrl Pts',(75.3888507691892,35.1632015561783,60.5891291622963));
#46131=CARTESIAN_POINT('Ctrl Pts',(68.8451573284352,34.5267335275214,57.4492797977542));
#46132=CARTESIAN_POINT('Ctrl Pts',(67.9372838577583,33.8902654988645,50.2482837805935));
#46133=CARTESIAN_POINT('Ctrl Pts',(73.5203313009761,33.2537974702075,45.5887627150886));
#46134=CARTESIAN_POINT('Ctrl Pts',(79.2808791639645,32.7234074463268,47.4106468950583));
#46135=CARTESIAN_POINT('Ctrl Pts',(81.4098578636657,32.2990954272222,51.2673100625624));
#46136=CARTESIAN_POINT('Ctrl Pts',(81.5388551947532,31.8747834081175,55.6706906713012));
#46137=CARTESIAN_POINT('Ctrl Pts',(77.506184276696,31.3443933842367,60.1696615427363));
#46138=CARTESIAN_POINT('Ctrl Pts',(70.3291838819809,30.7079253555798,58.9982433210564));
#46139=CARTESIAN_POINT('Ctrl Pts',(67.4475988877123,30.0714573269228,52.3367835833502));
#46140=CARTESIAN_POINT('Ctrl Pts',(71.484050000639,29.4349892982659,46.3047325057651));
#46141=CARTESIAN_POINT('Ctrl Pts',(78.7546137265724,28.798521269609,46.4477656105936));
#46142=CARTESIAN_POINT('Ctrl Pts',(81.9091522462999,28.2681312457281,51.6006347683443));
#46143=CARTESIAN_POINT('Ctrl Pts',(80.9876044002968,27.8438192266235,55.9084358736837));
#46144=CARTESIAN_POINT('Ctrl Pts',(78.1975779862256,27.4195072075189,59.3175639504902));
#46145=CARTESIAN_POINT('Ctrl Pts',(72.2028217646185,26.8891171836381,60.0699406911801));
#46146=CARTESIAN_POINT('Ctrl Pts',(67.5523365863765,26.2526491549812,54.4793646218784));
#46147=CARTESIAN_POINT('Ctrl Pts',(69.7448518505325,25.6161811263242,47.5604440708494));
#46148=CARTESIAN_POINT('Ctrl Pts',(76.7477451945052,24.9797130976673,45.6530752563823));
#46149=CARTESIAN_POINT('Ctrl Pts',(82.1432115679278,24.3432450690103,50.5285739238167));
#46150=CARTESIAN_POINT('Ctrl Pts',(81.1459994984225,23.8128550451296,56.4874982978904));
#46151=CARTESIAN_POINT('Ctrl Pts',(77.6254897250416,23.3885430260249,59.1355878854457));
#46152=CARTESIAN_POINT('Ctrl Pts',(73.2835643711842,22.9642310069203,59.8799816336974));
#46153=CARTESIAN_POINT('Ctrl Pts',(68.2641906043349,22.4338409830396,56.5170763685288));
#46154=CARTESIAN_POINT('Ctrl Pts',(68.4189717999724,21.7973729543825,49.2467891067138));
#46155=CARTESIAN_POINT('Ctrl Pts',(74.6112626053506,21.1609049257256,45.4606524580492));
#46156=CARTESIAN_POINT('Ctrl Pts',(81.1491080247995,20.5244368970687,48.6127033352101));
#46157=CARTESIAN_POINT('Ctrl Pts',(82.0257404859492,19.8879688684117,55.8314197936231));
#46158=CARTESIAN_POINT('Ctrl Pts',(77.3652888960716,19.357578844531,59.67691183969));
#46159=CARTESIAN_POINT('Ctrl Pts',(72.9710754988905,18.9332668254264,59.3670937145644));
#46160=CARTESIAN_POINT('Ctrl Pts',(69.2044438305179,18.5089548063216,57.0832108846456));
#46161=CARTESIAN_POINT('Ctrl Pts',(67.6207990335978,17.9785647824409,51.2501750211296));
#46162=CARTESIAN_POINT('Ctrl Pts',(72.5034949652097,17.3420967537839,45.867555022826));
#46163=CARTESIAN_POINT('Ctrl Pts',(79.6639947113501,16.705628725127,47.0607241995588));
#46164=CARTESIAN_POINT('Ctrl Pts',(82.5280615917182,16.0691606964701,53.7441206728326));
#46165=CARTESIAN_POINT('Ctrl Pts',(79.1441898800705,15.5387706725893,58.7368424313125));
#46166=CARTESIAN_POINT('Ctrl Pts',(74.8250353359302,15.1144586534846,59.6854325760972));
#46167=CARTESIAN_POINT('Ctrl Pts',(72.7133095752997,14.9023026439323,59.1035909146895));
#46168=CARTESIAN_POINT('Ctrl Pts',(71.7889077421008,14.7962246391561,58.5705443090233));
#46169=CARTESIAN_POINT('Ctrl Pts',(81.4785525543966,416.203775360844,49.9893084691035));
#46170=CARTESIAN_POINT('Ctrl Pts',(81.9840157928199,416.097697356068,51.0708177306788));
#46171=CARTESIAN_POINT('Ctrl Pts',(82.4299547886268,415.885541346517,53.4804382935736));
#46172=CARTESIAN_POINT('Ctrl Pts',(80.9582422516561,415.461229327411,58.2036999304802));
#46173=CARTESIAN_POINT('Ctrl Pts',(75.0685408665669,414.930839303531,61.496467711432));
#46174=CARTESIAN_POINT('Ctrl Pts',(67.8937906392098,414.294371274873,57.6628752630338));
#46175=CARTESIAN_POINT('Ctrl Pts',(67.2508294905527,413.657903246217,49.5670757676227));
#46176=CARTESIAN_POINT('Ctrl Pts',(73.718922518142,413.021435217559,44.6410769108337));
#46177=CARTESIAN_POINT('Ctrl Pts',(80.0686778630768,412.49104519368,46.965884990772));
#46178=CARTESIAN_POINT('Ctrl Pts',(82.25299431647,412.066733174574,51.3834126799471));
#46179=CARTESIAN_POINT('Ctrl Pts',(82.1767433586505,411.642421155469,56.3110700424759));
#46180=CARTESIAN_POINT('Ctrl Pts',(77.4433054371268,411.11203113159,61.1368214020091));
#46181=CARTESIAN_POINT('Ctrl Pts',(69.4811941105652,410.475563102931,59.4671289711532));
#46182=CARTESIAN_POINT('Ctrl Pts',(66.5950617600235,409.839095074275,51.877423575915));
#46183=CARTESIAN_POINT('Ctrl Pts',(71.4093060937056,409.202627045618,45.3385398027193));
#46184=CARTESIAN_POINT('Ctrl Pts',(79.5278545587503,408.566159016961,45.8635327706843));
#46185=CARTESIAN_POINT('Ctrl Pts',(82.7946954417536,408.035768993081,51.780929813614));
#46186=CARTESIAN_POINT('Ctrl Pts',(81.5484021999293,407.611456973975,56.5491632997459));
#46187=CARTESIAN_POINT('Ctrl Pts',(78.2589949233612,407.187144954872,60.2191781771201));
#46188=CARTESIAN_POINT('Ctrl Pts',(71.5213106968269,406.656754930989,60.7589992545326));
#46189=CARTESIAN_POINT('Ctrl Pts',(66.6045666361791,406.020286902334,54.2772777506614));
#46190=CARTESIAN_POINT('Ctrl Pts',(69.4024450885366,405.383818873676,46.6546195494321));
#46191=CARTESIAN_POINT('Ctrl Pts',(77.3248506119125,404.74735084502,44.8745774504162));
#46192=CARTESIAN_POINT('Ctrl Pts',(83.1101172875948,404.110882816362,50.594523777757));
#46193=CARTESIAN_POINT('Ctrl Pts',(81.6963520392216,403.580492792482,57.2042904096785));
#46194=CARTESIAN_POINT('Ctrl Pts',(77.628749663687,403.156180773377,59.9870701412823));
#46195=CARTESIAN_POINT('Ctrl Pts',(72.7387204177423,402.731868754272,60.6009634894842));
#46196=CARTESIAN_POINT('Ctrl Pts',(67.2978137931106,402.201478730392,56.5904419086148));
#46197=CARTESIAN_POINT('Ctrl Pts',(67.8359280893625,401.565010701735,48.4727124088158));
#46198=CARTESIAN_POINT('Ctrl Pts',(74.9467087207757,400.928542673078,44.5522724819652));
#46199=CARTESIAN_POINT('Ctrl Pts',(82.0953268474851,400.292074644421,48.4032865620621));
#46200=CARTESIAN_POINT('Ctrl Pts',(82.7124605889277,399.655606615763,56.5153914131592));
#46201=CARTESIAN_POINT('Ctrl Pts',(77.3108636907342,399.125216591883,60.5787027420174));
#46202=CARTESIAN_POINT('Ctrl Pts',(72.4150885587465,398.700904572778,60.012454295511));
#46203=CARTESIAN_POINT('Ctrl Pts',(68.3205822654791,398.276592553674,57.269414074572));
#46204=CARTESIAN_POINT('Ctrl Pts',(66.842522433118,397.746202529794,50.6737270631735));
#46205=CARTESIAN_POINT('Ctrl Pts',(72.5718181519236,397.109734501135,44.8977189491651));
#46206=CARTESIAN_POINT('Ctrl Pts',(80.5111804111243,396.47326647248,46.6005335121155));
#46207=CARTESIAN_POINT('Ctrl Pts',(83.3831514950707,395.836798443821,54.1955866793042));
#46208=CARTESIAN_POINT('Ctrl Pts',(78.5297532607916,395.200330415166,60.7248764373814));
#46209=CARTESIAN_POINT('Ctrl Pts',(71.7871355199413,394.669940391284,60.250688688689));
#46210=CARTESIAN_POINT('Ctrl Pts',(68.4621429042898,394.24562837218,56.6128767711974));
#46211=CARTESIAN_POINT('Ctrl Pts',(67.1694890357017,393.821316353075,51.857006985639));
#46212=CARTESIAN_POINT('Ctrl Pts',(70.378532996455,393.290926329195,45.908075579219));
#46213=CARTESIAN_POINT('Ctrl Pts',(78.4916253724822,392.654458300537,45.3040629441663));
#46214=CARTESIAN_POINT('Ctrl Pts',(83.369240344066,392.017990271881,51.7957439828776));
#46215=CARTESIAN_POINT('Ctrl Pts',(80.5572835813138,391.381522243223,59.4132205784301));
#46216=CARTESIAN_POINT('Ctrl Pts',(72.611543813093,390.745054214568,61.16030921412));
#46217=CARTESIAN_POINT('Ctrl Pts',(67.831823084552,390.214664190685,56.3809768572411));
#46218=CARTESIAN_POINT('Ctrl Pts',(67.7068767052643,389.790352171582,51.4541482785849));
#46219=CARTESIAN_POINT('Ctrl Pts',(69.8494823980434,389.366040152476,47.0158499237608));
#46220=CARTESIAN_POINT('Ctrl Pts',(76.1731818767277,388.835650128596,44.628681533462));
#46221=CARTESIAN_POINT('Ctrl Pts',(82.6946133383874,388.199182099939,49.4926337182714));
#46222=CARTESIAN_POINT('Ctrl Pts',(82.1204242508757,387.562714071282,57.5922236715447));
#46223=CARTESIAN_POINT('Ctrl Pts',(75.0024131187421,386.926246042624,61.4995204406948));
#46224=CARTESIAN_POINT('Ctrl Pts',(67.8577857377302,386.289778013968,57.6083254119501));
#46225=CARTESIAN_POINT('Ctrl Pts',(67.3830501033545,385.759387990087,50.8657462245909));
#46226=CARTESIAN_POINT('Ctrl Pts',(70.5193743378369,385.335075970983,47.0640726803003));
#46227=CARTESIAN_POINT('Ctrl Pts',(75.0473516294541,384.910763951878,45.1181350945174));
#46228=CARTESIAN_POINT('Ctrl Pts',(81.3870609052464,384.380373927997,47.4624546799801));
#46229=CARTESIAN_POINT('Ctrl Pts',(83.1212960289457,383.74390589934,55.4110097499891));
#46230=CARTESIAN_POINT('Ctrl Pts',(77.3766585294485,383.107437870683,61.1496673036992));
#46231=CARTESIAN_POINT('Ctrl Pts',(69.4404556010515,382.470969842026,59.4321884541394));
#46232=CARTESIAN_POINT('Ctrl Pts',(66.5978452811112,381.834501813369,51.8094156165031));
#46233=CARTESIAN_POINT('Ctrl Pts',(70.6607176773544,381.304111789489,46.407488561072));
#46234=CARTESIAN_POINT('Ctrl Pts',(75.5214972956857,380.879799770384,45.5938099124785));
#46235=CARTESIAN_POINT('Ctrl Pts',(80.2161137011552,380.455487751279,47.0937526602727));
#46236=CARTESIAN_POINT('Ctrl Pts',(83.4653421691651,379.925097727398,53.0208313996709));
#46237=CARTESIAN_POINT('Ctrl Pts',(79.562596700756,379.288629698742,60.1591559211569));
#46238=CARTESIAN_POINT('Ctrl Pts',(71.4624131206521,378.652161670085,60.7249089485447));
#46239=CARTESIAN_POINT('Ctrl Pts',(66.5967992159111,378.015693641428,54.2242280727153));
#46240=CARTESIAN_POINT('Ctrl Pts',(69.4490998372052,377.37922561277,46.6050758671872));
#46241=CARTESIAN_POINT('Ctrl Pts',(76.0587516032023,376.84883558889,45.1907733703342));
#46242=CARTESIAN_POINT('Ctrl Pts',(80.2621792448387,376.424523569785,47.7637963983479));
#46243=CARTESIAN_POINT('Ctrl Pts',(82.8230482444123,376.000211550681,51.9746397115319));
#46244=CARTESIAN_POINT('Ctrl Pts',(81.3896570115272,375.4698215268,58.5801781145572));
#46245=CARTESIAN_POINT('Ctrl Pts',(73.7622965822203,374.833353498143,61.4104558476921));
#46246=CARTESIAN_POINT('Ctrl Pts',(67.2756991158776,374.196885469486,56.526082415099));
#46247=CARTESIAN_POINT('Ctrl Pts',(67.8648504208867,373.560417440829,48.4275670413289));
#46248=CARTESIAN_POINT('Ctrl Pts',(75.0144198050572,372.923949412172,44.5454597802954));
#46249=CARTESIAN_POINT('Ctrl Pts',(80.9320871080452,372.393559388292,47.8117974406574));
#46250=CARTESIAN_POINT('Ctrl Pts',(82.4184613089243,371.969247369187,52.5107274439798));
#46251=CARTESIAN_POINT('Ctrl Pts',(81.5907437386188,371.544935350082,57.3691361407621));
#46252=CARTESIAN_POINT('Ctrl Pts',(76.1771019836737,371.014545326201,61.4163859439578));
#46253=CARTESIAN_POINT('Ctrl Pts',(68.56257297831,370.378077297545,58.5517660404247));
#46254=CARTESIAN_POINT('Ctrl Pts',(66.8680282099687,369.741609268887,50.6106346004175));
#46255=CARTESIAN_POINT('Ctrl Pts',(72.6232575130191,369.105141240231,44.8825994932723));
#46256=CARTESIAN_POINT('Ctrl Pts',(80.5667693788841,368.468673211573,46.6397899787074));
#46257=CARTESIAN_POINT('Ctrl Pts',(82.8927643814735,367.938283187694,52.9862453096999));
#46258=CARTESIAN_POINT('Ctrl Pts',(80.9337540321524,367.513971168588,57.5085820831407));
#46259=CARTESIAN_POINT('Ctrl Pts',(77.1230358177255,367.089659149484,60.6339105669001));
#46260=CARTESIAN_POINT('Ctrl Pts',(70.3818562312212,366.559269125603,60.139698261462));
#46261=CARTESIAN_POINT('Ctrl Pts',(66.5113175699981,365.922801096946,52.9838594121572));
#46262=CARTESIAN_POINT('Ctrl Pts',(70.4391612727063,365.286333068289,45.8771657810459));
#46263=CARTESIAN_POINT('Ctrl Pts',(78.5403762034458,364.649865039632,45.3263780130745));
#46264=CARTESIAN_POINT('Ctrl Pts',(83.3854683136115,364.013397010975,51.8618337438747));
#46265=CARTESIAN_POINT('Ctrl Pts',(80.9800413351421,363.483006987094,58.17861053838));
#46266=CARTESIAN_POINT('Ctrl Pts',(76.5355717224607,363.058694967989,60.3083854802736));
#46267=CARTESIAN_POINT('Ctrl Pts',(71.6091246607767,362.634382948885,60.169206496283));
#46268=CARTESIAN_POINT('Ctrl Pts',(66.8436203934035,362.103992925004,55.3756986890502));
#46269=CARTESIAN_POINT('Ctrl Pts',(68.6136562040615,361.467524896347,47.4350392457652));
#46270=CARTESIAN_POINT('Ctrl Pts',(76.2392244809221,360.83105686769,44.6451003621484));
#46271=CARTESIAN_POINT('Ctrl Pts',(82.7167874777929,360.194588839034,49.5414488118559));
#46272=CARTESIAN_POINT('Ctrl Pts',(82.0893394325227,359.558120810376,57.6527623994156));
#46273=CARTESIAN_POINT('Ctrl Pts',(76.1311622360508,359.027730786496,60.8446070879602));
#46274=CARTESIAN_POINT('Ctrl Pts',(71.3790466468484,358.603418767391,59.5382193706177));
#46275=CARTESIAN_POINT('Ctrl Pts',(67.7508554881302,358.179106748286,56.2027313468106));
#46276=CARTESIAN_POINT('Ctrl Pts',(67.2961484816295,357.648716724406,49.4587718600854));
#46277=CARTESIAN_POINT('Ctrl Pts',(73.8394319867204,357.012248695747,44.6242563582749));
#46278=CARTESIAN_POINT('Ctrl Pts',(81.4261566169365,356.375780667092,47.5181568238498));
#46279=CARTESIAN_POINT('Ctrl Pts',(83.1060280328521,355.739312638434,55.4624052178373));
#46280=CARTESIAN_POINT('Ctrl Pts',(77.3134926462889,355.102844609778,61.174990706095));
#46281=CARTESIAN_POINT('Ctrl Pts',(70.7221031282585,354.572454585897,59.6778827467444));
#46282=CARTESIAN_POINT('Ctrl Pts',(67.990902982154,354.148142566792,55.575469164098));
#46283=CARTESIAN_POINT('Ctrl Pts',(67.4388003141422,353.723830547688,50.6780786257463));
#46284=CARTESIAN_POINT('Ctrl Pts',(71.5176993728649,353.193440523807,45.2882427758245));
#46285=CARTESIAN_POINT('Ctrl Pts',(79.6279875335611,352.556972495149,45.928809021977));
#46286=CARTESIAN_POINT('Ctrl Pts',(83.4583338857497,351.920504466493,53.0885225177573));
#46287=CARTESIAN_POINT('Ctrl Pts',(79.5173679668675,351.284036437836,60.1879477160104));
#46288=CARTESIAN_POINT('Ctrl Pts',(71.3981177848255,350.647568409179,60.7026084262373));
#46289=CARTESIAN_POINT('Ctrl Pts',(67.4033311812638,350.117178385299,55.2501385260585));
#46290=CARTESIAN_POINT('Ctrl Pts',(68.0313487922679,349.692866366194,50.3619031265067));
#46291=CARTESIAN_POINT('Ctrl Pts',(70.8258678013444,349.268554347089,46.3023569758795));
#46292=CARTESIAN_POINT('Ctrl Pts',(77.439691116236,348.738164323209,44.9076924356594));
#46293=CARTESIAN_POINT('Ctrl Pts',(83.142900440987,348.101696294551,50.7094596287924));
#46294=CARTESIAN_POINT('Ctrl Pts',(81.339978828426,347.465228265895,58.6266892060083));
#46295=CARTESIAN_POINT('Ctrl Pts',(73.7092694259971,346.828760237237,61.4025358399319));
#46296=CARTESIAN_POINT('Ctrl Pts',(67.2417793772208,346.192292208581,56.4670853403098));
#46297=CARTESIAN_POINT('Ctrl Pts',(67.8010619555309,345.6619021847,49.7309921834458));
#46298=CARTESIAN_POINT('Ctrl Pts',(71.4805654193212,345.237590165595,46.4521958035041));
#46299=CARTESIAN_POINT('Ctrl Pts',(76.2523772184292,344.81327814649,45.2196928237691));
#46300=CARTESIAN_POINT('Ctrl Pts',(82.1603168760152,344.28288812261,48.5035924907313));
#46301=CARTESIAN_POINT('Ctrl Pts',(82.6618450551038,343.646420093953,56.6236644516698));
#46302=CARTESIAN_POINT('Ctrl Pts',(76.1090964696637,343.009952065296,61.4189263314207));
#46303=CARTESIAN_POINT('Ctrl Pts',(68.527730982823,342.373484036639,58.5110150751538));
#46304=CARTESIAN_POINT('Ctrl Pts',(66.8811049173047,341.737016007982,50.5438498474461));
#46305=CARTESIAN_POINT('Ctrl Pts',(71.720405297618,341.206625984101,45.8248542075397));
#46306=CARTESIAN_POINT('Ctrl Pts',(76.6484187293896,340.782313964996,45.7621241713557));
#46307=CARTESIAN_POINT('Ctrl Pts',(81.0593106533463,340.358001945892,47.9605972497298));
#46308=CARTESIAN_POINT('Ctrl Pts',(83.3664454132111,339.827611922011,54.3139331624748));
#46309=CARTESIAN_POINT('Ctrl Pts',(78.4205410235596,339.191143893355,60.7734322865299));
#46310=CARTESIAN_POINT('Ctrl Pts',(70.3288464427964,338.554675864696,60.0970231418323));
#46311=CARTESIAN_POINT('Ctrl Pts',(66.5117334947267,337.918207836041,52.9302456748633));
#46312=CARTESIAN_POINT('Ctrl Pts',(70.4928267712495,337.281739807383,45.8353182271111));
#46313=CARTESIAN_POINT('Ctrl Pts',(77.2408625316589,336.751349783503,45.4457525759158));
#46314=CARTESIAN_POINT('Ctrl Pts',(81.0026336516775,336.327037764398,48.6298269283381));
#46315=CARTESIAN_POINT('Ctrl Pts',(82.8912456562173,335.902725745293,53.1820127920165));
#46316=CARTESIAN_POINT('Ctrl Pts',(80.4670674549858,335.372335721413,59.4916172224879));
#46317=CARTESIAN_POINT('Ctrl Pts',(72.4972494389857,334.735867692755,61.1253552544506));
#46318=CARTESIAN_POINT('Ctrl Pts',(66.8315814033232,334.099399664099,55.3087190934851));
#46319=CARTESIAN_POINT('Ctrl Pts',(68.6491262437196,333.462931635441,47.394833747302));
#46320=CARTESIAN_POINT('Ctrl Pts',(76.3071823965364,332.826463606785,44.6486955269013));
#46321=CARTESIAN_POINT('Ctrl Pts',(81.6573808253843,332.296073582904,48.7794490649748));
#46322=CARTESIAN_POINT('Ctrl Pts',(82.4096221682912,331.871761563799,53.650114769289));
#46323=CARTESIAN_POINT('Ctrl Pts',(80.8505245226236,331.447449544695,58.3254186067349));
#46324=CARTESIAN_POINT('Ctrl Pts',(74.882893320288,330.917059520814,61.4995524812376));
#46325=CARTESIAN_POINT('Ctrl Pts',(67.7944140660781,330.280591492156,57.5069892659745));
#46326=CARTESIAN_POINT('Ctrl Pts',(67.3309794578124,329.6441234635,49.4003081396909));
#46327=CARTESIAN_POINT('Ctrl Pts',(73.8925756369099,329.007655434842,44.6171600025495));
#46328=CARTESIAN_POINT('Ctrl Pts',(81.4751072165895,328.371187406186,47.5654330578139));
#46329=CARTESIAN_POINT('Ctrl Pts',(82.8058431840019,327.840797382305,54.1924150108138));
#46330=CARTESIAN_POINT('Ctrl Pts',(80.1799525690512,327.4164853632,58.3630204727915));
#46331=CARTESIAN_POINT('Ctrl Pts',(75.9371112497972,326.992173344096,60.8705190232977));
#46332=CARTESIAN_POINT('Ctrl Pts',(69.3501974549747,326.461783320215,59.3538401911343));
#46333=CARTESIAN_POINT('Ctrl Pts',(66.6164487614888,325.825315291559,51.691352524188));
#46334=CARTESIAN_POINT('Ctrl Pts',(71.5823329553481,325.188847262901,45.2669424584653));
#46335=CARTESIAN_POINT('Ctrl Pts',(79.6727641285602,324.552379234245,45.9582990603005));
#46336=CARTESIAN_POINT('Ctrl Pts',(83.4642911203485,323.915911205587,53.1563142197581));
#46337=CARTESIAN_POINT('Ctrl Pts',(80.1234970628893,323.385521181707,59.0322688729184));
#46338=CARTESIAN_POINT('Ctrl Pts',(75.4061745846681,322.961209162602,60.4591956676878));
#46339=CARTESIAN_POINT('Ctrl Pts',(70.5586039634535,322.536897143498,59.570201565626));
#46340=CARTESIAN_POINT('Ctrl Pts',(66.5800296844598,322.006507119616,54.1058905635982));
#46341=CARTESIAN_POINT('Ctrl Pts',(69.5405626672157,321.37003909096,46.5281373594319));
#46342=CARTESIAN_POINT('Ctrl Pts',(77.5024565125574,320.733571062303,44.9339927879165));
#46343=CARTESIAN_POINT('Ctrl Pts',(83.1573692157493,320.097103033646,50.7610857886042));
#46344=CARTESIAN_POINT('Ctrl Pts',(81.3000236219517,319.460635004989,58.6817780885513));
#46345=CARTESIAN_POINT('Ctrl Pts',(74.9247060490522,318.930244981108,60.9274570204177));
#46346=CARTESIAN_POINT('Ctrl Pts',(70.4274643213623,318.505932962003,58.9115035775307));
#46347=CARTESIAN_POINT('Ctrl Pts',(67.3504992812629,318.081620942899,55.0616285687585));
#46348=CARTESIAN_POINT('Ctrl Pts',(67.9297866619199,317.551230919018,48.3272262826633));
#46349=CARTESIAN_POINT('Ctrl Pts',(75.1339247210432,316.914762890361,44.5473461271119));
#46350=CARTESIAN_POINT('Ctrl Pts',(82.1904587146737,316.278294861704,48.56460620285));
#46351=CARTESIAN_POINT('Ctrl Pts',(82.6389162345453,315.641826833047,56.6721296454466));
#46352=CARTESIAN_POINT('Ctrl Pts',(76.0428070816436,315.00535880439,61.4343185547872));
#46353=CARTESIAN_POINT('Ctrl Pts',(69.7569048494634,314.47496878051,58.9493273781782));
#46354=CARTESIAN_POINT('Ctrl Pts',(67.6834157706895,314.050656761404,54.4783213972643));
#46355=CARTESIAN_POINT('Ctrl Pts',(67.8847852268376,313.6263447423,49.554024312066));
#46356=CARTESIAN_POINT('Ctrl Pts',(72.7380804298073,313.095954718419,44.8494229800522));
#46357=CARTESIAN_POINT('Ctrl Pts',(80.6557583488287,312.459486689763,46.7195768603191));
#46358=CARTESIAN_POINT('Ctrl Pts',(83.3491940360832,311.823018661106,54.3797631973481));
#46359=CARTESIAN_POINT('Ctrl Pts',(78.371449849321,311.186550632448,60.794988316589));
#46360=CARTESIAN_POINT('Ctrl Pts',(70.2687050190405,310.550082603792,60.0651764363069));
#46361=CARTESIAN_POINT('Ctrl Pts',(67.1523430005122,310.01969257991,54.0671737862719));
#46362=CARTESIAN_POINT('Ctrl Pts',(68.5186270318996,309.595380560807,49.3319315129835));
#46363=CARTESIAN_POINT('Ctrl Pts',(71.8996589006993,309.171068541701,45.7461436018928));
#46364=CARTESIAN_POINT('Ctrl Pts',(78.6488219679938,308.640678517821,45.3766224097839));
#46365=CARTESIAN_POINT('Ctrl Pts',(83.4003362781905,308.004210489164,51.980425172226));
#46366=CARTESIAN_POINT('Ctrl Pts',(80.4108761268251,307.367742460507,59.5300065197432));
#46367=CARTESIAN_POINT('Ctrl Pts',(72.4460508424404,306.73127443185,61.1094395536548));
#46368=CARTESIAN_POINT('Ctrl Pts',(66.8070575550918,306.094806403193,55.2452385108463));
#46369=CARTESIAN_POINT('Ctrl Pts',(68.3872693902216,305.564416379312,48.6732769637535));
#46370=CARTESIAN_POINT('Ctrl Pts',(72.5238402316145,305.140104360207,45.9940918049221));
#46371=CARTESIAN_POINT('Ctrl Pts',(77.4278112662491,304.715792341103,45.5038678432214));
#46372=CARTESIAN_POINT('Ctrl Pts',(82.7657170999594,304.185402317222,49.6504941020972));
#46373=CARTESIAN_POINT('Ctrl Pts',(82.0228010115598,303.548934288565,57.7520479561944));
#46374=CARTESIAN_POINT('Ctrl Pts',(74.8152960849149,302.912466259908,61.4916900850307));
#46375=CARTESIAN_POINT('Ctrl Pts',(67.766195626519,302.275998231251,57.4614006107094));
#46376=CARTESIAN_POINT('Ctrl Pts',(67.3540899986238,301.639530202594,49.3362994964648));
#46377=CARTESIAN_POINT('Ctrl Pts',(72.8565636478503,301.109140178714,45.4106744812704));
#46378=CARTESIAN_POINT('Ctrl Pts',(77.7364800159439,300.684828159609,46.1003611359));
#46379=CARTESIAN_POINT('Ctrl Pts',(81.7604188366507,300.260516140504,48.9459134211992));
#46380=CARTESIAN_POINT('Ctrl Pts',(83.0714657426214,299.730126116623,55.5768186407524));
#46381=CARTESIAN_POINT('Ctrl Pts',(77.1981520130348,299.093658087967,61.2063199507342));
#46382=CARTESIAN_POINT('Ctrl Pts',(69.304317310222,298.45719005931,59.3035787166069));
#46383=CARTESIAN_POINT('Ctrl Pts',(66.625037661451,297.820722030652,51.6384295932651));
#46384=CARTESIAN_POINT('Ctrl Pts',(71.6417535996899,297.184254001996,45.2337703236194));
#46385=CARTESIAN_POINT('Ctrl Pts',(78.3702482810813,296.653863978115,45.8780585687687));
#46386=CARTESIAN_POINT('Ctrl Pts',(81.6023257081562,296.22955195901,49.5986669795743));
#46387=CARTESIAN_POINT('Ctrl Pts',(82.7744813091102,295.805239939906,54.3856600533435));
#46388=CARTESIAN_POINT('Ctrl Pts',(79.4162494666852,295.274849916025,60.2516660977382));
#46389=CARTESIAN_POINT('Ctrl Pts',(71.2904924510428,294.638381887368,60.6506298654907));
#46390=CARTESIAN_POINT('Ctrl Pts',(66.5783481405078,294.001913858711,54.0378583953677));
#46391=CARTESIAN_POINT('Ctrl Pts',(69.5817503009291,293.365445830054,46.4938126649812));
#46392=CARTESIAN_POINT('Ctrl Pts',(77.5690708348405,292.728977801397,44.9479116805083));
#46393=CARTESIAN_POINT('Ctrl Pts',(82.2265890673596,292.198587777516,49.8464085861014));
#46394=CARTESIAN_POINT('Ctrl Pts',(82.2270927597987,291.774275758412,54.7748212298901));
#46395=CARTESIAN_POINT('Ctrl Pts',(79.9731027840799,291.349963739307,59.1576035231967));
#46396=CARTESIAN_POINT('Ctrl Pts',(73.5911433082559,290.819573715426,61.3843368411525));
#46397=CARTESIAN_POINT('Ctrl Pts',(67.1946063176981,290.183105686769,56.3572687399966));
#46398=CARTESIAN_POINT('Ctrl Pts',(67.9731276840741,289.546637658112,48.2747595379305));
#46399=CARTESIAN_POINT('Ctrl Pts',(75.1875289332066,288.910169629455,44.548438948408));
#46400=CARTESIAN_POINT('Ctrl Pts',(82.2316253496051,288.273701600798,48.6187957929263));
#46401=CARTESIAN_POINT('Ctrl Pts',(82.5359589117053,287.743311576918,55.3712123309765));
#46402=CARTESIAN_POINT('Ctrl Pts',(79.3046420575872,287.318999557813,59.0924813120438));
#46403=CARTESIAN_POINT('Ctrl Pts',(74.7289733472039,286.894687538709,60.9234666462241));
#46404=CARTESIAN_POINT('Ctrl Pts',(68.4504796612101,286.364297514828,58.4198163001721));
#46405=CARTESIAN_POINT('Ctrl Pts',(66.917499177202,285.72782948617,50.4300059143811));
#46406=CARTESIAN_POINT('Ctrl Pts',(72.8052066912012,285.091361457514,44.8382306373356));
#46407=CARTESIAN_POINT('Ctrl Pts',(80.6955127959515,284.454893428857,46.7555517092276));
#46408=CARTESIAN_POINT('Ctrl Pts',(83.3447411178743,283.8184254002,54.4476703031889));
#46409=CARTESIAN_POINT('Ctrl Pts',(79.1467649771149,283.288035376319,59.7452871581497));
#46410=CARTESIAN_POINT('Ctrl Pts',(74.2669896853412,282.863723357215,60.4359712704303));
#46411=CARTESIAN_POINT('Ctrl Pts',(69.6117437691718,282.43941133811,58.8179672836763));
#46412=CARTESIAN_POINT('Ctrl Pts',(66.5132105196755,281.909021314229,52.810734998995));
#46413=CARTESIAN_POINT('Ctrl Pts',(70.5949549734316,281.272553285572,45.77323108216));
#46414=CARTESIAN_POINT('Ctrl Pts',(78.7068412505005,280.636085256915,45.4121887753791));
#46415=CARTESIAN_POINT('Ctrl Pts',(83.4067610738744,279.999617228258,52.0336541851837));
#46416=CARTESIAN_POINT('Ctrl Pts',(80.362985608619,279.363149199602,59.5783563053703));
#46417=CARTESIAN_POINT('Ctrl Pts',(73.7197299652048,278.83275917572,60.8253135927701));
#46418=CARTESIAN_POINT('Ctrl Pts',(69.5826115753629,278.408447156616,58.146974019528));
#46419=CARTESIAN_POINT('Ctrl Pts',(67.1288832280929,277.984135137511,53.8728111027727));
#46420=CARTESIAN_POINT('Ctrl Pts',(68.7286078653029,277.453745113631,47.3055720249368));
#46421=CARTESIAN_POINT('Ctrl Pts',(76.4250011893648,276.817277084973,44.6687881948561));
#46422=CARTESIAN_POINT('Ctrl Pts',(82.7861996525964,276.180809056317,49.7153914713944));
#46423=CARTESIAN_POINT('Ctrl Pts',(81.9927479724166,275.54434102766,57.7964486392779));
#46424=CARTESIAN_POINT('Ctrl Pts',(74.7474345703678,274.907872999002,61.4967909033568));
#46425=CARTESIAN_POINT('Ctrl Pts',(68.9141293322307,274.377482975122,58.0820730498474));
#46426=CARTESIAN_POINT('Ctrl Pts',(67.5468774292204,273.953170956017,53.3471101487385));
#46427=CARTESIAN_POINT('Ctrl Pts',(68.4970063364964,273.528858936913,48.5111504197167));
#46428=CARTESIAN_POINT('Ctrl Pts',(74.0111154460782,272.998468913031,44.6018859431201));
#46429=CARTESIAN_POINT('Ctrl Pts',(81.5508847771878,272.362000884375,47.6578600265996));
#46430=CARTESIAN_POINT('Ctrl Pts',(83.0443750077863,271.725532855717,55.6392469643748));
#46431=CARTESIAN_POINT('Ctrl Pts',(77.1463472849624,271.089064827061,61.2201357376961));
#46432=CARTESIAN_POINT('Ctrl Pts',(69.24973729534,270.452596798404,59.2629311400528));
#46433=CARTESIAN_POINT('Ctrl Pts',(67.0847324481688,269.922206774523,52.8597677006208));
#46434=CARTESIAN_POINT('Ctrl Pts',(69.1573075942886,269.497894755419,48.3883379846521));
#46435=CARTESIAN_POINT('Ctrl Pts',(73.0457256368976,269.073582736314,45.3602269287172));
#46436=CARTESIAN_POINT('Ctrl Pts',(79.7722770006702,268.543192712434,46.0244970325772));
#46437=CARTESIAN_POINT('Ctrl Pts',(83.4608960488652,267.906724683776,53.2757857926896));
#46438=CARTESIAN_POINT('Ctrl Pts',(79.3548600457172,267.27025665512,60.2810351715653));
#46439=CARTESIAN_POINT('Ctrl Pts',(71.2423206209435,266.633788626462,60.6270909486741));
#46440=CARTESIAN_POINT('Ctrl Pts',(66.5637941172022,265.997320597805,53.9713799484104));
#46441=CARTESIAN_POINT('Ctrl Pts',(69.1279533259856,265.466930573925,47.717354399025));
#46442=CARTESIAN_POINT('Ctrl Pts',(73.6247828917563,265.04261855482,45.7004817462351));
#46443=CARTESIAN_POINT('Ctrl Pts',(78.5461449518434,264.618306535716,45.9640095715196));
#46444=CARTESIAN_POINT('Ctrl Pts',(83.189093324536,264.087916511834,50.876318440968));
#46445=CARTESIAN_POINT('Ctrl Pts',(81.219119521118,263.451448483178,58.7697525718826));
#46446=CARTESIAN_POINT('Ctrl Pts',(73.5255363375579,262.81498045452,61.3662556658578));
#46447=CARTESIAN_POINT('Ctrl Pts',(67.1736718335224,262.178512425864,56.3079093113901));
#46448=CARTESIAN_POINT('Ctrl Pts',(68.0057311996598,261.542044397207,48.2150250062452));
#46449=CARTESIAN_POINT('Ctrl Pts',(74.0426030807442,261.011654373326,45.1746424790414));
#46450=CARTESIAN_POINT('Ctrl Pts',(78.7602171292713,260.587342354221,46.6006050067058));
#46451=CARTESIAN_POINT('Ctrl Pts',(82.3030301339121,260.163030335117,50.0266417045987));
#46452=CARTESIAN_POINT('Ctrl Pts',(82.5873066012716,259.632640311236,56.7799323773343));
#46453=CARTESIAN_POINT('Ctrl Pts',(75.9240373827595,258.996172282579,61.4476879929244));
#46454=CARTESIAN_POINT('Ctrl Pts',(68.4128028985451,258.359704253922,58.3631447459379));
#46455=CARTESIAN_POINT('Ctrl Pts',(66.9340600453635,257.723236225265,50.3790123513977));
#46456=CARTESIAN_POINT('Ctrl Pts',(72.8689918530231,257.086768196608,44.814510252946));
#46457=CARTESIAN_POINT('Ctrl Pts',(79.4204777041344,256.556378172727,46.4775740409702));
#46458=CARTESIAN_POINT('Ctrl Pts',(82.0472207506454,256.132066153623,50.6476426745507));
#46459=CARTESIAN_POINT('Ctrl Pts',(82.4754878528197,255.707754134518,55.5574123972929));
#46460=CARTESIAN_POINT('Ctrl Pts',(78.26179546342,255.177364110638,60.8425372272155));
#46461=CARTESIAN_POINT('Ctrl Pts',(70.1702674939088,254.540896081981,59.997389734845));
#46462=CARTESIAN_POINT('Ctrl Pts',(66.5219257752229,253.904428053323,52.7432424229221));
#46463=CARTESIAN_POINT('Ctrl Pts',(70.6408962821711,253.267960024667,45.7455904965778));
#46464=CARTESIAN_POINT('Ctrl Pts',(78.7705529966446,252.631491996009,45.4361056503313));
#46465=CARTESIAN_POINT('Ctrl Pts',(82.6263905866329,252.101101972129,50.9877058250546));
#46466=CARTESIAN_POINT('Ctrl Pts',(81.8751448406308,251.676789953024,55.8585251883935));
#46467=CARTESIAN_POINT('Ctrl Pts',(78.9790129269844,251.252477933919,59.8462151688108));
#46468=CARTESIAN_POINT('Ctrl Pts',(72.3320829248196,250.722087910039,61.0734354288592));
#46469=CARTESIAN_POINT('Ctrl Pts',(66.7771871043503,250.085619881382,55.1295115069896));
#46470=CARTESIAN_POINT('Ctrl Pts',(68.7794446183971,249.449151852725,47.2603301412549));
#46471=CARTESIAN_POINT('Ctrl Pts',(76.4778114578293,248.812683824068,44.6780446177483));
#46472=CARTESIAN_POINT('Ctrl Pts',(82.818618895214,248.176215795411,49.7752262122422));
#46473=CARTESIAN_POINT('Ctrl Pts',(82.0894276979053,247.64582577153,56.495049738059));
#46474=CARTESIAN_POINT('Ctrl Pts',(78.3283074924612,247.221513752426,59.6798929432045));
#46475=CARTESIAN_POINT('Ctrl Pts',(73.5268963031717,246.797201733321,60.7915142962413));
#46476=CARTESIAN_POINT('Ctrl Pts',(67.7037590511224,246.26681170944,57.3594856593927));
#46477=CARTESIAN_POINT('Ctrl Pts',(67.4074232989018,245.630343680783,49.2293390255862));
#46478=CARTESIAN_POINT('Ctrl Pts',(74.0791634226038,244.993875652126,44.601063510757));
#46479=CARTESIAN_POINT('Ctrl Pts',(81.5846866984392,244.357407623469,47.6994777624791));
#46480=CARTESIAN_POINT('Ctrl Pts',(83.0296161489375,243.720939594812,55.705680236082));
#46481=CARTESIAN_POINT('Ctrl Pts',(78.0727036535351,243.190549570932,60.3009785434037));
#46482=CARTESIAN_POINT('Ctrl Pts',(73.1446775024716,242.766237551827,60.2392558117977));
#46483=CARTESIAN_POINT('Ctrl Pts',(68.7907035582628,242.341925532722,57.9301082776814));
#46484=CARTESIAN_POINT('Ctrl Pts',(66.6447266758118,241.811535508841,51.5205426730296));
#46485=CARTESIAN_POINT('Ctrl Pts',(71.7521570557332,241.175067480185,45.1879875742171));
#46486=CARTESIAN_POINT('Ctrl Pts',(79.8241923372792,240.538599451528,46.0684970476793));
#46487=CARTESIAN_POINT('Ctrl Pts',(83.4591265052232,239.902131422871,53.3293719339515));
#46488=CARTESIAN_POINT('Ctrl Pts',(79.3001550032014,239.265663394214,60.3215143245647));
#46489=CARTESIAN_POINT('Ctrl Pts',(72.544434181319,238.735273370333,60.540567279651));
#46490=CARTESIAN_POINT('Ctrl Pts',(68.8642605968896,238.310961351228,57.2625230716464));
#46491=CARTESIAN_POINT('Ctrl Pts',(67.0911938351403,237.886649332124,52.6641009836316));
#46492=CARTESIAN_POINT('Ctrl Pts',(69.6739171853377,237.356259308243,46.4177189814885));
#46493=CARTESIAN_POINT('Ctrl Pts',(77.6824461774659,236.719791279586,44.9857404385333));
#46494=CARTESIAN_POINT('Ctrl Pts',(83.1994372355666,236.083323250929,50.943580666688));
#46495=CARTESIAN_POINT('Ctrl Pts',(81.1826455981949,235.446855222272,58.8090496298719));
#46496=CARTESIAN_POINT('Ctrl Pts',(73.4576908674786,234.810387193615,61.360945704093));
#46497=CARTESIAN_POINT('Ctrl Pts',(68.2135001509705,234.279997169734,57.0964162166533));
#46498=CARTESIAN_POINT('Ctrl Pts',(67.5844833805876,233.85568515063,52.2083092882258));
#46499=CARTESIAN_POINT('Ctrl Pts',(69.2611357605872,233.431373131525,47.5738634488822));
#46500=CARTESIAN_POINT('Ctrl Pts',(75.3070114336774,232.900983107644,44.5514248033759));
#46501=CARTESIAN_POINT('Ctrl Pts',(82.2924180697097,232.264515078987,48.7216997696805));
#46502=CARTESIAN_POINT('Ctrl Pts',(82.5510105163721,231.628047050331,56.8374979723166));
#46503=CARTESIAN_POINT('Ctrl Pts',(75.8707314929994,230.991579021673,61.4534402043034));
#46504=CARTESIAN_POINT('Ctrl Pts',(68.3650616350141,230.355110993017,58.3146475783642));
#46505=CARTESIAN_POINT('Ctrl Pts',(67.2020818219682,229.824720969136,51.6561773355309));
#46506=CARTESIAN_POINT('Ctrl Pts',(69.9324433631728,229.400408950031,47.5532055716795));
#46507=CARTESIAN_POINT('Ctrl Pts',(74.2372464756337,228.976096930926,45.153638609574));
#46508=CARTESIAN_POINT('Ctrl Pts',(80.7837638639308,228.445706907046,46.8361540181632));
#46509=CARTESIAN_POINT('Ctrl Pts',(83.3231624660204,227.809238878389,54.5652260134286));
#46510=CARTESIAN_POINT('Ctrl Pts',(78.1966446526784,227.172770849732,60.8621987497656));
#46511=CARTESIAN_POINT('Ctrl Pts',(70.1262498027585,226.536302821075,59.9667784859756));
#46512=CARTESIAN_POINT('Ctrl Pts',(66.5176821833719,225.899834792418,52.6753219146804));
#46513=CARTESIAN_POINT('Ctrl Pts',(70.0057794549039,225.369444768537,46.8855960570804));
#46514=CARTESIAN_POINT('Ctrl Pts',(74.7576279024003,224.945132749433,45.5782370184392));
#46515=CARTESIAN_POINT('Ctrl Pts',(79.5812057975926,224.520820730328,46.5893492570011));
#46516=CARTESIAN_POINT('Ctrl Pts',(83.4205371902028,223.990430706447,52.1523773979725));
#46517=CARTESIAN_POINT('Ctrl Pts',(80.2696092965562,223.35396267779,59.6529608354047));
#46518=CARTESIAN_POINT('Ctrl Pts',(72.2700015158721,222.717494649133,61.0455586352526));
#46519=CARTESIAN_POINT('Ctrl Pts',(66.7640267170464,222.081026620477,55.0775364602583));
#46520=CARTESIAN_POINT('Ctrl Pts',(68.8207776695637,221.444558591819,47.2062677138015));
#46521=CARTESIAN_POINT('Ctrl Pts',(75.2507673017546,220.914168567939,45.1222820533196));
#46522=CARTESIAN_POINT('Ctrl Pts',(79.6956704607921,220.489856548834,47.2511485607036));
#46523=CARTESIAN_POINT('Ctrl Pts',(82.6744481076051,220.065544529729,51.177489584318));
#46524=CARTESIAN_POINT('Ctrl Pts',(81.9252938141166,219.535154505848,57.8951179824144));
#46525=CARTESIAN_POINT('Ctrl Pts',(74.6280237911603,218.898686477192,61.4918872754814));
#46526=CARTESIAN_POINT('Ctrl Pts',(67.6751520575461,218.262218448535,57.2977309984761));
#46527=CARTESIAN_POINT('Ctrl Pts',(67.4315976480203,217.625750419878,49.1814669479095));
#46528=CARTESIAN_POINT('Ctrl Pts',(74.1457626120518,216.989282391221,44.5873525693379));
#46529=CARTESIAN_POINT('Ctrl Pts',(80.3670730043547,216.45889236734,47.2302639859052));
#46530=CARTESIAN_POINT('Ctrl Pts',(82.326772217929,216.034580348235,51.7522106868073));
#46531=CARTESIAN_POINT('Ctrl Pts',(82.0015904344453,215.61026832913,56.6698326205076));
#46532=CARTESIAN_POINT('Ctrl Pts',(77.0300273108705,215.07987830525,61.2504332600464));
#46533=CARTESIAN_POINT('Ctrl Pts',(69.1639586556176,214.443410276593,59.1808709821966));
#46534=CARTESIAN_POINT('Ctrl Pts',(66.6615043746255,213.806942247936,51.4552632310895));
#46535=CARTESIAN_POINT('Ctrl Pts',(71.8057768890687,213.170474219279,45.1675048243668));
#46536=CARTESIAN_POINT('Ctrl Pts',(79.875837106265,212.534006190622,46.1021564038283));
#46537=CARTESIAN_POINT('Ctrl Pts',(83.4558199511915,211.897538161965,53.3912589125365));
#46538=CARTESIAN_POINT('Ctrl Pts',(79.2479037367829,211.261070133308,60.3519747696568));
#46539=CARTESIAN_POINT('Ctrl Pts',(72.4900115795629,210.730680109427,60.5229592777618));
#46540=CARTESIAN_POINT('Ctrl Pts',(68.8339312330819,210.306368090323,57.2181407993583));
#46541=CARTESIAN_POINT('Ctrl Pts',(67.0939119457814,209.882056071218,52.6072020822089));
#46542=CARTESIAN_POINT('Ctrl Pts',(69.7217545659192,209.351666047338,46.3795117465403));
#46543=CARTESIAN_POINT('Ctrl Pts',(77.7403418401691,208.71519801868,45.0054097805767));
#46544=CARTESIAN_POINT('Ctrl Pts',(83.2142366884898,208.078729990024,51.0028705831539));
#46545=CARTESIAN_POINT('Ctrl Pts',(81.1407302675849,207.442261961366,58.8535994246372));
#46546=CARTESIAN_POINT('Ctrl Pts',(73.3975746836202,206.80579393271,61.3496845069219));
#46547=CARTESIAN_POINT('Ctrl Pts',(68.1842835917728,206.275403908829,57.0474339979407));
#46548=CARTESIAN_POINT('Ctrl Pts',(67.5905534492229,205.851091889724,52.1549137250446));
#46549=CARTESIAN_POINT('Ctrl Pts',(69.3005985145823,205.42677987062,47.5326867105072));
#46550=CARTESIAN_POINT('Ctrl Pts',(75.3681246161506,204.896389846739,44.5539470592515));
#46551=CARTESIAN_POINT('Ctrl Pts',(82.323260368906,204.259921818082,48.7745137060865));
#46552=CARTESIAN_POINT('Ctrl Pts',(82.523290720535,203.623453789425,56.8919662020949));
#46553=CARTESIAN_POINT('Ctrl Pts',(75.8098813557484,202.986985760768,61.4595900896012));
#46554=CARTESIAN_POINT('Ctrl Pts',(68.3270533669542,202.350517732111,58.2667255790149));
#46555=CARTESIAN_POINT('Ctrl Pts',(67.2121447459138,201.82012770823,51.6000377652461));
#46556=CARTESIAN_POINT('Ctrl Pts',(69.9720382395937,201.395815689125,47.516872378748));
#46557=CARTESIAN_POINT('Ctrl Pts',(74.294042205983,200.971503670021,45.1484271000031));
#46558=CARTESIAN_POINT('Ctrl Pts',(80.8282498308984,200.44111364614,46.8781319292539));
#46559=CARTESIAN_POINT('Ctrl Pts',(83.3118169635253,199.804645617483,54.6253245493258));
#46560=CARTESIAN_POINT('Ctrl Pts',(78.1399998377731,199.168177588826,60.8851454812851));
#46561=CARTESIAN_POINT('Ctrl Pts',(70.0762755157864,198.531709560169,59.9315205069422));
#46562=CARTESIAN_POINT('Ctrl Pts',(66.5204097940023,197.895241531512,52.614217852485));
#46563=CARTESIAN_POINT('Ctrl Pts',(70.0501892244093,197.364851507632,46.8498093669514));
#46564=CARTESIAN_POINT('Ctrl Pts',(74.8113466152267,196.940539488527,45.5767690130946));
#46565=CARTESIAN_POINT('Ctrl Pts',(79.6275037459071,196.516227469422,46.622657120516));
#46566=CARTESIAN_POINT('Ctrl Pts',(83.426597929181,195.985837445542,52.2132412945418));
#46567=CARTESIAN_POINT('Ctrl Pts',(80.2216351328844,195.349369416884,59.6908955149556));
#46568=CARTESIAN_POINT('Ctrl Pts',(72.21218812787,194.712901388228,61.02573977292));
#46569=CARTESIAN_POINT('Ctrl Pts',(66.7494156897398,194.076433359571,55.0181472593925));
#46570=CARTESIAN_POINT('Ctrl Pts',(68.8629050529468,193.439965330914,47.1619228559709));
#46571=CARTESIAN_POINT('Ctrl Pts',(75.3077621678543,192.909575307033,45.1243839511291));
#46572=CARTESIAN_POINT('Ctrl Pts',(79.7371915239832,192.485263287928,47.2852650261152));
#46573=CARTESIAN_POINT('Ctrl Pts',(82.6875597010222,192.060951268824,51.2329959010707));
#46574=CARTESIAN_POINT('Ctrl Pts',(81.8899644877527,191.530561244943,57.9450440159248));
#46575=CARTESIAN_POINT('Ctrl Pts',(74.5669202423437,190.894093216286,61.4890702778233));
#46576=CARTESIAN_POINT('Ctrl Pts',(67.6445141591816,190.257625187629,57.2448572130513));
#46577=CARTESIAN_POINT('Ctrl Pts',(67.4594805854599,189.621157158972,49.1270488206354));
#46578=CARTESIAN_POINT('Ctrl Pts',(74.2067042249644,188.984689130315,44.5814935934104));
#46579=CARTESIAN_POINT('Ctrl Pts',(80.4086254297172,188.454299106434,47.2692289580603));
#46580=CARTESIAN_POINT('Ctrl Pts',(82.3358832685874,188.02998708733,51.805188466662));
#46581=CARTESIAN_POINT('Ctrl Pts',(81.9747666998536,187.605675068225,56.7203533942049));
#46582=CARTESIAN_POINT('Ctrl Pts',(76.9713079038153,187.075285044344,61.2649268721786));
#46583=CARTESIAN_POINT('Ctrl Pts',(69.1185120770804,186.438817015687,59.1387338261796));
#46584=CARTESIAN_POINT('Ctrl Pts',(66.6751619948799,185.80234898703,51.3951499727439));
#46585=CARTESIAN_POINT('Ctrl Pts',(71.8585347015804,185.165880958374,45.1448941457544));
#46586=CARTESIAN_POINT('Ctrl Pts',(79.933317849207,184.529412929716,46.1373538598204));
#46587=CARTESIAN_POINT('Ctrl Pts',(82.853329412247,183.999022905836,52.2333591495215));
#46588=CARTESIAN_POINT('Ctrl Pts',(81.3340493427206,183.574710886731,56.9217532788052));
#46589=CARTESIAN_POINT('Ctrl Pts',(77.8383970300113,183.150398867627,60.3958958132751));
#46590=CARTESIAN_POINT('Ctrl Pts',(71.0807955528553,182.620008843746,60.5461299515229));
#46591=CARTESIAN_POINT('Ctrl Pts',(66.5461590499559,181.983540815089,53.7915632776489));
#46592=CARTESIAN_POINT('Ctrl Pts',(69.77911925036,181.347072786432,46.343005104285));
#46593=CARTESIAN_POINT('Ctrl Pts',(77.7910185814084,180.710604757775,45.0229597912255));
#46594=CARTESIAN_POINT('Ctrl Pts',(83.236675387159,180.074136729118,51.0671240112991));
#46595=CARTESIAN_POINT('Ctrl Pts',(81.4439564155797,179.543746705237,57.584324845192));
#46596=CARTESIAN_POINT('Ctrl Pts',(77.2225935943312,179.119434686133,60.1278160231877));
#46597=CARTESIAN_POINT('Ctrl Pts',(72.3052933996905,178.695122667028,60.4585882060443));
#46598=CARTESIAN_POINT('Ctrl Pts',(67.1048092041633,178.164732643147,56.1408674933977));
#46599=CARTESIAN_POINT('Ctrl Pts',(68.1103275583388,177.52826461449,48.0677000849601));
#46600=CARTESIAN_POINT('Ctrl Pts',(75.4354306841967,176.891796585833,44.5639999386958));
#46601=CARTESIAN_POINT('Ctrl Pts',(82.3499841876386,176.255328557176,48.8209942266199));
#46602=CARTESIAN_POINT('Ctrl Pts',(82.4981144191685,175.618860528519,56.9551909662954));
#46603=CARTESIAN_POINT('Ctrl Pts',(76.8711065575554,175.088470504638,60.7001249504526));
#46604=CARTESIAN_POINT('Ctrl Pts',(72.0161507801839,174.664158485534,59.8523892363709));
#46605=CARTESIAN_POINT('Ctrl Pts',(68.0867054412862,174.239846466429,56.8777109731333));
#46606=CARTESIAN_POINT('Ctrl Pts',(66.9916029022179,173.709456442548,50.2077410744549));
#46607=CARTESIAN_POINT('Ctrl Pts',(73.0445668764352,173.072988413891,44.771867060824));
#46608=CARTESIAN_POINT('Ctrl Pts',(80.8724741977796,172.436520385235,46.9298562841126));
#46609=CARTESIAN_POINT('Ctrl Pts',(83.3015145995298,171.800052356578,54.6779407729424));
#46610=CARTESIAN_POINT('Ctrl Pts',(78.0795336709331,171.16358432792,60.9163712122925));
#46611=CARTESIAN_POINT('Ctrl Pts',(71.3755001146967,170.63319430404,60.0540011657286));
#46612=CARTESIAN_POINT('Ctrl Pts',(68.2659050293063,170.208882284935,56.2304334801661));
#46613=CARTESIAN_POINT('Ctrl Pts',(67.2497632531332,169.78457026583,51.4079126319087));
#46614=CARTESIAN_POINT('Ctrl Pts',(70.7966483253109,169.25418024195,45.6540135795167));
#46615=CARTESIAN_POINT('Ctrl Pts',(78.931074007745,168.617712213293,45.5190395738844));
#46616=CARTESIAN_POINT('Ctrl Pts',(83.4260701168421,167.981244184636,52.2812921940239));
#46617=CARTESIAN_POINT('Ctrl Pts',(80.1793549532992,167.344776155979,59.7238650802109));
#46618=CARTESIAN_POINT('Ctrl Pts',(72.1460607507099,166.708308127322,61.0096657723415));
#46619=CARTESIAN_POINT('Ctrl Pts',(67.6500129020043,166.177918103441,55.9625575148834));
#46620=CARTESIAN_POINT('Ctrl Pts',(67.8094963160762,165.753606084337,51.0367259625668));
#46621=CARTESIAN_POINT('Ctrl Pts',(70.2045728718383,165.329294065232,46.7294228929882));
#46622=CARTESIAN_POINT('Ctrl Pts',(76.6554533739143,164.798904041351,44.7110352274765));
#46623=CARTESIAN_POINT('Ctrl Pts',(82.8854297614923,164.162436012694,49.9430991964524));
#46624=CARTESIAN_POINT('Ctrl Pts',(81.8449431247788,163.525967984037,57.9960761663812));
#46625=CARTESIAN_POINT('Ctrl Pts',(74.5133797567601,162.88949995538,61.4862379248261));
#46626=CARTESIAN_POINT('Ctrl Pts',(67.6051283307556,162.253031926723,57.1893598255144));
#46627=CARTESIAN_POINT('Ctrl Pts',(67.5201530810369,161.722641902843,50.430622722528));
#46628=CARTESIAN_POINT('Ctrl Pts',(70.8705672900159,161.298329883738,46.8162104508805));
#46629=CARTESIAN_POINT('Ctrl Pts',(75.5032621757575,160.874017864633,45.1347261254156));
#46630=CARTESIAN_POINT('Ctrl Pts',(81.6971730222364,160.343627840753,47.840870328193));
#46631=CARTESIAN_POINT('Ctrl Pts',(82.9699791975185,159.707159812095,55.8762336432774));
#46632=CARTESIAN_POINT('Ctrl Pts',(76.9038536928211,159.070691783439,61.2739342537818));
#46633=CARTESIAN_POINT('Ctrl Pts',(69.0799464026406,158.434223754781,59.1014874226617));
#46634=CARTESIAN_POINT('Ctrl Pts',(66.6818169764982,157.797755726125,51.3274232075481));
#46635=CARTESIAN_POINT('Ctrl Pts',(71.0495526412501,157.267365702244,46.1688736843576));
#46636=CARTESIAN_POINT('Ctrl Pts',(75.9491772112947,156.84305368314,45.6369615546028));
#46637=CARTESIAN_POINT('Ctrl Pts',(80.5494457748369,156.418741664034,47.4052320611843));
#46638=CARTESIAN_POINT('Ctrl Pts',(83.4513383514884,155.888351640154,53.5098833611299));
#46639=CARTESIAN_POINT('Ctrl Pts',(79.1432926512695,155.251883611497,60.411176095833));
#46640=CARTESIAN_POINT('Ctrl Pts',(71.0239614089819,154.61541558284,60.5086989003167));
#46641=CARTESIAN_POINT('Ctrl Pts',(66.5414655682442,153.978947554183,53.7381537555628));
#46642=CARTESIAN_POINT('Ctrl Pts',(69.8285540663259,153.342479525526,46.2962354295517));
#46643=CARTESIAN_POINT('Ctrl Pts',(76.5087873933404,152.812089501645,45.2655896528667));
#46644=CARTESIAN_POINT('Ctrl Pts',(80.5567807350017,152.387777482541,48.0768173823518));
#46645=CARTESIAN_POINT('Ctrl Pts',(82.8704673911375,151.963465463436,52.4283809517351));
#46646=CARTESIAN_POINT('Ctrl Pts',(81.0583992028712,151.433075439555,58.9402283778824));
#46647=CARTESIAN_POINT('Ctrl Pts',(73.2804664854723,150.796607410899,61.3257811039523));
#46648=CARTESIAN_POINT('Ctrl Pts',(67.0864441542822,150.160139382241,56.0753394196649));
#46649=CARTESIAN_POINT('Ctrl Pts',(68.1418060998694,149.523671353585,48.0242983886437));
#46650=CARTESIAN_POINT('Ctrl Pts',(75.5034220168983,148.887203324927,44.5611047389346));
#46651=CARTESIAN_POINT('Ctrl Pts',(81.2228038404513,148.356813301047,48.1633845138502));
#46652=CARTESIAN_POINT('Ctrl Pts',(82.4356281071999,147.932501281942,52.9402358553873));
#46653=CARTESIAN_POINT('Ctrl Pts',(81.3290143292153,147.508189262838,57.7428036464279));
#46654=CARTESIAN_POINT('Ctrl Pts',(75.6909082376934,146.977799238957,61.4710080025618));
#46655=CARTESIAN_POINT('Ctrl Pts',(68.2543160943122,146.3413312103,58.1718874442559));
#46656=CARTESIAN_POINT('Ctrl Pts',(67.0207059165395,145.704863181643,50.1462250760347));
#46657=CARTESIAN_POINT('Ctrl Pts',(73.0967927917064,145.068395152986,44.7597402477996));
#46658=CARTESIAN_POINT('Ctrl Pts',(80.925705939638,144.431927124329,46.9722542223041));
#46659=CARTESIAN_POINT('Ctrl Pts',(82.881709341265,143.901537100448,53.4423236742635));
#46660=CARTESIAN_POINT('Ctrl Pts',(80.6650743178658,143.477225081343,57.8441165606002));
#46661=CARTESIAN_POINT('Ctrl Pts',(76.680406627644,143.052913062239,60.7444053116841));
#46662=CARTESIAN_POINT('Ctrl Pts',(69.9789640188073,142.522523038358,59.8621270217908));
#46663=CARTESIAN_POINT('Ctrl Pts',(66.5276813793795,141.886055009701,52.4949194566393));
#46664=CARTESIAN_POINT('Ctrl Pts',(70.8589587750538,141.249586981044,45.6266528164233));
#46665=CARTESIAN_POINT('Ctrl Pts',(78.9784563259308,140.613118952387,45.5441298457715));
#46666=CARTESIAN_POINT('Ctrl Pts',(83.4384584367587,139.97665092373,52.3482080593613));
#46667=CARTESIAN_POINT('Ctrl Pts',(80.6726315496697,139.44626089985,58.5156994173616));
#46668=CARTESIAN_POINT('Ctrl Pts',(76.1126999566996,139.021948880745,60.3855323801142));
#46669=CARTESIAN_POINT('Ctrl Pts',(71.2024863013405,138.59763686164,59.9623854790432));
#46670=CARTESIAN_POINT('Ctrl Pts',(66.7214489996053,138.06724683776,54.9019455059963));
#46671=CARTESIAN_POINT('Ctrl Pts',(68.9466223548929,137.430778809102,47.0766210587825));
#46672=CARTESIAN_POINT('Ctrl Pts',(76.7204388137733,136.794310780446,44.7312366163038));
#46673=CARTESIAN_POINT('Ctrl Pts',(82.9047508995969,136.157842751789,49.9931121891882));
#46674=CARTESIAN_POINT('Ctrl Pts',(81.8104176813927,135.521374723132,58.0547208359023));
#46675=CARTESIAN_POINT('Ctrl Pts',(75.6780301032495,134.990984699251,60.8975311728376));
#46676=CARTESIAN_POINT('Ctrl Pts',(71.0091921999896,134.566672680146,59.3191763096188));
#46677=CARTESIAN_POINT('Ctrl Pts',(67.5794628759647,134.142360661042,55.7799379445062));
#46678=CARTESIAN_POINT('Ctrl Pts',(67.5145625264963,133.611970637161,49.0209782638311));
#46679=CARTESIAN_POINT('Ctrl Pts',(74.3258453287723,132.975502608504,44.5719867204963));
#46680=CARTESIAN_POINT('Ctrl Pts',(81.7329902478001,132.339034579847,47.8987350830714));
#46681=CARTESIAN_POINT('Ctrl Pts',(82.9517716971165,131.70256655119,55.9266627296179));
#46682=CARTESIAN_POINT('Ctrl Pts',(76.8393321334314,131.066098522533,61.2955715336061));
#46683=CARTESIAN_POINT('Ctrl Pts',(70.345285756154,130.535708498652,59.4207089599438));
#46684=CARTESIAN_POINT('Ctrl Pts',(67.8552964618423,130.111396479548,55.1675683843954));
#46685=CARTESIAN_POINT('Ctrl Pts',(67.5866367229714,129.687084460443,50.2464838102518));
#46686=CARTESIAN_POINT('Ctrl Pts',(71.9696748354462,129.156694436562,45.1009299115017));
#46687=CARTESIAN_POINT('Ctrl Pts',(80.0295029927227,128.520226407905,46.208300328485));
#46688=CARTESIAN_POINT('Ctrl Pts',(83.4404367354544,127.883758379248,53.5770574504209));
#46689=CARTESIAN_POINT('Ctrl Pts',(79.0964782825046,127.247290350591,60.4373107604981));
#46690=CARTESIAN_POINT('Ctrl Pts',(70.9610596341513,126.610822321935,60.4827264104982));
#46691=CARTESIAN_POINT('Ctrl Pts',(67.2874710471809,126.080432298054,54.8088833641994));
#46692=CARTESIAN_POINT('Ctrl Pts',(68.1964381006051,125.656120278949,49.9650181372395));
#46693=CARTESIAN_POINT('Ctrl Pts',(71.2204926199176,125.231808259844,46.0734444574296));
#46694=CARTESIAN_POINT('Ctrl Pts',(77.9037576629453,124.701418235964,45.0626445835687));
#46695=CARTESIAN_POINT('Ctrl Pts',(83.2627733484823,124.064950207307,51.1837596819317));
#46696=CARTESIAN_POINT('Ctrl Pts',(81.0061205939446,123.42848217865,58.9837961475401));
#46697=CARTESIAN_POINT('Ctrl Pts',(73.2279845331631,122.792014149993,61.3148152249716));
#46698=CARTESIAN_POINT('Ctrl Pts',(67.0559843616916,122.155546121336,56.0144838156537));
#46699=CARTESIAN_POINT('Ctrl Pts',(68.0029311293476,121.625156097455,49.3218729768572));
#46700=CARTESIAN_POINT('Ctrl Pts',(71.8654559343288,121.200844078351,46.2608023190536));
#46701=CARTESIAN_POINT('Ctrl Pts',(76.7004222277914,120.776532059246,45.3056309301169));
#46702=CARTESIAN_POINT('Ctrl Pts',(82.409079478992,120.246142035365,48.9248822903661));
#46703=CARTESIAN_POINT('Ctrl Pts',(82.4413370611576,119.609674006708,57.0603637520646));
#46704=CARTESIAN_POINT('Ctrl Pts',(75.6228694268662,118.973205978051,61.4696210182606));
#46705=CARTESIAN_POINT('Ctrl Pts',(68.221882988768,118.336737949394,58.1291943595137));
#46706=CARTESIAN_POINT('Ctrl Pts',(67.0376135633978,117.700269920737,50.0803059211407));
#46707=CARTESIAN_POINT('Ctrl Pts',(72.1410868314743,117.169879896856,45.6483415008885));
#46708=CARTESIAN_POINT('Ctrl Pts',(77.0645120916213,116.745567877752,45.8700059971645));
#46709=CARTESIAN_POINT('Ctrl Pts',(81.3412314624846,116.321255858647,48.3192758606224));
#46710=CARTESIAN_POINT('Ctrl Pts',(83.2780090997717,115.790865834766,54.7951264151101));
#46711=CARTESIAN_POINT('Ctrl Pts',(77.9677021950907,115.15439780611,60.9585458997256));
#46712=CARTESIAN_POINT('Ctrl Pts',(69.9285043781874,114.517929777452,59.8164649130708));
#46713=CARTESIAN_POINT('Ctrl Pts',(66.5311895114466,113.881461748796,52.4414190002914));
#46714=CARTESIAN_POINT('Ctrl Pts',(70.9149490262317,113.244993720139,45.5879708402938));
#46715=CARTESIAN_POINT('Ctrl Pts',(77.6742202802328,112.714603696258,45.5883385159239));
#46716=CARTESIAN_POINT('Ctrl Pts',(81.2460419438328,112.290291677153,48.9841214071873));
#46717=CARTESIAN_POINT('Ctrl Pts',(82.8688995985184,111.865979658049,53.6376775177111));
#46718=CARTESIAN_POINT('Ctrl Pts',(80.0847664798852,111.335589634168,59.7969267250482));
#46719=CARTESIAN_POINT('Ctrl Pts',(72.0339731633678,110.699121605511,60.9681765446677));
#46720=CARTESIAN_POINT('Ctrl Pts',(66.7132940162291,110.062653576854,54.8343829442452));
#46721=CARTESIAN_POINT('Ctrl Pts',(68.9843527215643,109.426185548197,47.0385287334289));
#46722=CARTESIAN_POINT('Ctrl Pts',(76.7880761542206,108.78971751954,44.7387461889578));
#46723=CARTESIAN_POINT('Ctrl Pts',(81.8910672320391,108.259327495659,49.1712657974936));
#46724=CARTESIAN_POINT('Ctrl Pts',(82.3610740579104,107.835015476555,54.0772157589995));
#46725=CARTESIAN_POINT('Ctrl Pts',(80.5348612828878,107.41070345745,58.6547913554813));
#46726=CARTESIAN_POINT('Ctrl Pts',(74.3940571549151,106.880313433569,61.4793749853676));
#46727=CARTESIAN_POINT('Ctrl Pts',(67.5477081342156,106.243845404912,57.0845366206481));
#46728=CARTESIAN_POINT('Ctrl Pts',(67.5527081847441,105.607377376255,48.9646212566263));
#46729=CARTESIAN_POINT('Ctrl Pts',(74.3793098536259,104.970909347599,44.5679679642004));
#46730=CARTESIAN_POINT('Ctrl Pts',(81.7791320279888,104.334441318941,47.948756474748));
#46731=CARTESIAN_POINT('Ctrl Pts',(82.7253506908695,103.804051295061,54.6414702936983));
#46732=CARTESIAN_POINT('Ctrl Pts',(79.8632368833852,103.379739275956,58.6536462611964));
#46733=CARTESIAN_POINT('Ctrl Pts',(75.482807461588,102.955427256852,60.9122054306265));
#46734=CARTESIAN_POINT('Ctrl Pts',(68.9943583695012,102.425037232971,59.0180627750301));
#46735=CARTESIAN_POINT('Ctrl Pts',(66.7072003664947,101.788569204314,51.2106299424965));
#46736=CARTESIAN_POINT('Ctrl Pts',(72.0354295638575,101.152101175657,45.0833936862588));
#46737=CARTESIAN_POINT('Ctrl Pts',(80.0725037797786,100.515633147,46.2403243527888));
#46738=CARTESIAN_POINT('Ctrl Pts',(83.4424732424755,99.8791651183427,53.6450799183514));
#46739=CARTESIAN_POINT('Ctrl Pts',(79.7682674113498,99.3487750944621,59.3185232758616));
#46740=CARTESIAN_POINT('Ctrl Pts',(74.9764836612738,98.9244630753574,60.4709381029394));
#46741=CARTESIAN_POINT('Ctrl Pts',(70.1882708520563,98.5001510562529,59.3037750745634));
#46742=CARTESIAN_POINT('Ctrl Pts',(66.5315506863656,97.969761032372,53.6190459121331));
#46743=CARTESIAN_POINT('Ctrl Pts',(69.9243030493936,97.3332930037152,46.2247014132335));
#46744=CARTESIAN_POINT('Ctrl Pts',(77.9649013017072,96.696824975058,45.0925219821032));
#46745=CARTESIAN_POINT('Ctrl Pts',(83.274239787846,96.0603569464012,51.2361345479301));
#46746=CARTESIAN_POINT('Ctrl Pts',(80.9630539287384,95.4238889177443,59.036488327721));
#46747=CARTESIAN_POINT('Ctrl Pts',(74.4688036207804,94.8934988938635,60.9106443932431));
#46748=CARTESIAN_POINT('Ctrl Pts',(70.0953489534175,94.4691868747589,58.6386088051227));
#46749=CARTESIAN_POINT('Ctrl Pts',(67.2456020024424,94.0448748556542,54.6176395492626));
#46750=CARTESIAN_POINT('Ctrl Pts',(68.2124227130756,93.5144848317734,47.9278708138097));
#46751=CARTESIAN_POINT('Ctrl Pts',(75.6226190920302,92.8780168031165,44.5698820123746));
#46752=CARTESIAN_POINT('Ctrl Pts',(82.4356513262645,92.2415487744595,48.9875332315941));
#46753=CARTESIAN_POINT('Ctrl Pts',(82.4156505377467,91.6050807458026,57.1074255022982));
#46754=CARTESIAN_POINT('Ctrl Pts',(75.5558024799644,90.9686127171457,61.4811634676289));
#46755=CARTESIAN_POINT('Ctrl Pts',(69.4237242117114,90.4382226932648,58.6376859958749));
#46756=CARTESIAN_POINT('Ctrl Pts',(67.6116142203724,90.0139106741602,54.0545092787436));
#46757=CARTESIAN_POINT('Ctrl Pts',(68.0967239942248,89.5895986550556,49.1500296989643));
#46758=CARTESIAN_POINT('Ctrl Pts',(73.2133383912805,89.0592086311748,44.7332429560714));
#46759=CARTESIAN_POINT('Ctrl Pts',(81.0099439184418,88.4227406025178,47.0570418757459));
#46760=CARTESIAN_POINT('Ctrl Pts',(83.2569888118268,87.7862725738611,54.8598516111228));
#46761=CARTESIAN_POINT('Ctrl Pts',(77.9174492393249,87.1498045452039,60.9772340311672));
#46762=CARTESIAN_POINT('Ctrl Pts',(69.870300303306,86.513336516547,59.7812017712456));
#46763=CARTESIAN_POINT('Ctrl Pts',(67.1051444032194,85.9829464926663,53.6134095512882));
#46764=CARTESIAN_POINT('Ctrl Pts',(68.74232243329,85.5586344735616,48.9648721964835));
#46765=CARTESIAN_POINT('Ctrl Pts',(72.3245826130747,85.1343224544571,45.5801028623201));
#46766=CARTESIAN_POINT('Ctrl Pts',(79.0838229603303,84.6039324305761,45.6005466482718));
#46767=CARTESIAN_POINT('Ctrl Pts',(83.4464602703434,83.9674644019194,52.4674597004751));
#46768=CARTESIAN_POINT('Ctrl Pts',(80.0264541074312,83.3309963732621,59.8320104922767));
#46769=CARTESIAN_POINT('Ctrl Pts',(71.9837779856266,82.6945283446056,60.9493337754575));
#46770=CARTESIAN_POINT('Ctrl Pts',(66.6924731135778,82.0580603159483,54.7695933346078));
#46771=CARTESIAN_POINT('Ctrl Pts',(68.6491803921887,81.5276702920678,48.2997367174807));
#46772=CARTESIAN_POINT('Ctrl Pts',(72.9334206715241,81.103358272963,45.8636462696356));
#46773=CARTESIAN_POINT('Ctrl Pts',(77.857505088695,80.6790462538584,45.6571418054232));
#46774=CARTESIAN_POINT('Ctrl Pts',(82.9473083685091,80.1486562299776,50.1047985584944));
#46775=CARTESIAN_POINT('Ctrl Pts',(81.738262429575,79.5121882013206,58.1500025386794));
#46776=CARTESIAN_POINT('Ctrl Pts',(74.327026064536,78.8757201726637,61.4676260949181));
#46777=CARTESIAN_POINT('Ctrl Pts',(67.5221666333459,78.2392521440068,57.0373960059586));
#46778=CARTESIAN_POINT('Ctrl Pts',(67.5794728051966,77.6027841153498,48.9020524257583));
#46779=CARTESIAN_POINT('Ctrl Pts',(73.299246492323,77.0723940914689,45.3003948922867));
#46780=CARTESIAN_POINT('Ctrl Pts',(78.1312489429735,76.6480820723644,46.2704483743535));
#46781=CARTESIAN_POINT('Ctrl Pts',(81.9843305554388,76.2237700532597,49.3433970444166));
#46782=CARTESIAN_POINT('Ctrl Pts',(82.9106666188498,75.693380029379,56.0388917623577));
#46783=CARTESIAN_POINT('Ctrl Pts',(76.7223762458708,75.0569120007221,61.3201947668195));
#46784=CARTESIAN_POINT('Ctrl Pts',(68.951454145031,74.4204439720651,58.9652382444899));
#46785=CARTESIAN_POINT('Ctrl Pts',(66.7188280111139,73.7839759434081,51.1582906293505));
#46786=CARTESIAN_POINT('Ctrl Pts',(72.0966649038226,73.1475079147512,45.0537046875637));
#46787=CARTESIAN_POINT('Ctrl Pts',(78.776786065805,72.6171178908704,46.0850772107525));
#46788=CARTESIAN_POINT('Ctrl Pts',(81.788844289455,72.1928058717658,49.9859433579692));
#46789=CARTESIAN_POINT('Ctrl Pts',(82.6828930144,71.7684938526612,54.8325842894381));
#46790=CARTESIAN_POINT('Ctrl Pts',(78.9918523597607,71.2381038287804,60.4950896453872));
#46791=CARTESIAN_POINT('Ctrl Pts',(70.8566121056435,70.6016358001233,60.4246256614701));
#46792=CARTESIAN_POINT('Ctrl Pts',(66.5337966215277,69.9651677714665,53.5510300369317));
#46793=CARTESIAN_POINT('Ctrl Pts',(69.9674022330036,69.3286997428095,46.1928099380068));
#46794=CARTESIAN_POINT('Ctrl Pts',(78.0306017252772,68.6922317141527,45.1102605797613));
#46795=CARTESIAN_POINT('Ctrl Pts',(82.3977761578423,68.1618416902719,50.2692852449376));
#46796=CARTESIAN_POINT('Ctrl Pts',(82.1139659178903,67.7375296711671,55.1895193032789));
#46797=CARTESIAN_POINT('Ctrl Pts',(79.6108932178857,67.3132176520626,59.4349731659012));
#46798=CARTESIAN_POINT('Ctrl Pts',(73.1111050136803,66.7828276281817,61.289832007114));
#46799=CARTESIAN_POINT('Ctrl Pts',(67.0152250258696,66.1463595995248,55.9021287543866));
#46800=CARTESIAN_POINT('Ctrl Pts',(68.2587182879284,65.5098915708679,47.8779917274786));
#46801=CARTESIAN_POINT('Ctrl Pts',(75.6760709899128,64.8734235422109,44.5740653642333));
#46802=CARTESIAN_POINT('Ctrl Pts',(82.4736232832814,64.236955513554,49.0440074202512));
#46803=CARTESIAN_POINT('Ctrl Pts',(82.3879127409199,63.7065654896732,55.8027352386563));
#46804=CARTESIAN_POINT('Ctrl Pts',(78.9473025349299,63.2822534705685,59.3313968619353));
#46805=CARTESIAN_POINT('Ctrl Pts',(74.2736270857796,62.857941451464,60.8953691242108));
#46806=CARTESIAN_POINT('Ctrl Pts',(68.1500214465859,62.3275514275831,58.03369094594));
#46807=CARTESIAN_POINT('Ctrl Pts',(67.0805147073622,61.6910833989263,49.9687511135548));
#46808=CARTESIAN_POINT('Ctrl Pts',(73.2809985327285,61.0546153702692,44.7259416710183));
#46809=CARTESIAN_POINT('Ctrl Pts',(81.0475568218978,60.4181473416123,47.095250190464));
#46810=CARTESIAN_POINT('Ctrl Pts',(83.2486258453396,59.7816793129554,54.9273887438406));
#46811=CARTESIAN_POINT('Ctrl Pts',(78.7520289407639,59.2512892890746,59.9740078396425));
#46812=CARTESIAN_POINT('Ctrl Pts',(73.8405357114601,58.8269772699699,60.3820344315018));
#46813=CARTESIAN_POINT('Ctrl Pts',(69.2863828551142,58.4026652508654,58.4981705292525));
#46814=CARTESIAN_POINT('Ctrl Pts',(66.5395584769716,57.8722752269845,52.3221925616754));
#46815=CARTESIAN_POINT('Ctrl Pts',(71.0204888657229,57.2358071983275,45.5318787238324));
#46816=CARTESIAN_POINT('Ctrl Pts',(79.1396938462357,56.5993391696707,45.6394008322464));
#46817=CARTESIAN_POINT('Ctrl Pts',(83.4498036605393,55.9628711410136,52.5209707045959));
#46818=CARTESIAN_POINT('Ctrl Pts',(79.9758541146286,55.3264031123569,59.8775170218364));
#46819=CARTESIAN_POINT('Ctrl Pts',(73.2717267795347,54.7960130884759,60.7391577214321));
#46820=CARTESIAN_POINT('Ctrl Pts',(69.2960078212935,54.3717010693713,57.8266141241198));
#46821=CARTESIAN_POINT('Ctrl Pts',(67.0929362059535,53.9473890502667,53.4180171932531));
#46822=CARTESIAN_POINT('Ctrl Pts',(69.0688513580473,53.416999026386,46.9540008464241));
#46823=CARTESIAN_POINT('Ctrl Pts',(76.9045396175281,52.780530997729,44.7656021931905));
#46824=CARTESIAN_POINT('Ctrl Pts',(82.9640129734279,52.1440629690721,50.1707694587362));
#46825=CARTESIAN_POINT('Ctrl Pts',(81.7056980278796,51.5075949404151,58.1925955611392));
#46826=CARTESIAN_POINT('Ctrl Pts',(74.2589833057556,50.871126911758,61.4688035845323));
#46827=CARTESIAN_POINT('Ctrl Pts',(68.6323828944269,50.3407368878774,57.7232574519121));
#46828=CARTESIAN_POINT('Ctrl Pts',(67.5405612290126,49.9164248687727,52.9173052161848));
#46829=CARTESIAN_POINT('Ctrl Pts',(68.7680874345769,49.4921128496681,48.1442107423851));
#46830=CARTESIAN_POINT('Ctrl Pts',(74.4985333885546,48.9617228257873,44.5595577342274));
#46831=CARTESIAN_POINT('Ctrl Pts',(81.8494514107689,48.3252547971304,48.0454010175555));
#46832=CARTESIAN_POINT('Ctrl Pts',(82.8800195992615,47.6887867684733,56.0996532937291));
#46833=CARTESIAN_POINT('Ctrl Pts',(76.6698607789289,47.0523187398166,61.3309990045025));
#46834=CARTESIAN_POINT('Ctrl Pts',(68.8993099268987,46.4158507111594,58.9215097181071));
#46835=CARTESIAN_POINT('Ctrl Pts',(67.1072999819816,45.8854606872789,52.4041138901965));
#46836=CARTESIAN_POINT('Ctrl Pts',(69.4343739189814,45.4611486681741,48.0596946732126));
#46837=CARTESIAN_POINT('Ctrl Pts',(73.4910037035292,45.0368366490696,45.2609438389505));
#46838=CARTESIAN_POINT('Ctrl Pts',(80.1680320593212,44.5064466251886,46.3121528363915));
#46839=CARTESIAN_POINT('Ctrl Pts',(83.4321916804705,43.8699785965318,53.7641566697841));
#46840=CARTESIAN_POINT('Ctrl Pts',(78.9288709150793,43.2335105678747,60.5208683406622));
#46841=CARTESIAN_POINT('Ctrl Pts',(70.8098784261097,42.5970425392179,60.3983469815706));
#46842=CARTESIAN_POINT('Ctrl Pts',(66.5231018828453,41.9605745105609,53.4838227005111));
#46843=CARTESIAN_POINT('Ctrl Pts',(69.4437766221635,41.4301844866802,47.3881351193222));
#46844=CARTESIAN_POINT('Ctrl Pts',(74.0494677974295,41.0058724675754,45.6340369922952));
#46845=CARTESIAN_POINT('Ctrl Pts',(78.9474314123798,40.5815604484709,46.1810323010362));
#46846=CARTESIAN_POINT('Ctrl Pts',(83.2992634568746,40.05117042459,51.3530054135783));
#46847=CARTESIAN_POINT('Ctrl Pts',(80.8772094409459,39.4147023959332,59.1196490586266));
#46848=CARTESIAN_POINT('Ctrl Pts',(73.0466503802297,38.7782343672763,61.267996171179));
#46849=CARTESIAN_POINT('Ctrl Pts',(66.9971728804178,38.1417663386192,55.8516438470915));
#46850=CARTESIAN_POINT('Ctrl Pts',(68.2947135064205,37.5052983099623,47.8202375263325));
#46851=CARTESIAN_POINT('Ctrl Pts',(74.4969270772327,36.9749082860815,45.1331768938991));
#46852=CARTESIAN_POINT('Ctrl Pts',(79.1244227975359,36.5505962669769,46.8289170861851));
#46853=CARTESIAN_POINT('Ctrl Pts',(82.4636925300972,36.1262842478722,50.453627984227));
#46854=CARTESIAN_POINT('Ctrl Pts',(82.3579078679477,35.5958942239916,57.2120714163713));
#46855=CARTESIAN_POINT('Ctrl Pts',(75.4364593130539,34.9594261953344,61.4876589862132));
#46856=CARTESIAN_POINT('Ctrl Pts',(68.1156767308743,34.3229581666776,57.9749402522543));
#46857=CARTESIAN_POINT('Ctrl Pts',(67.0999897413908,33.6864901380206,49.9187978467345));
#46858=CARTESIAN_POINT('Ctrl Pts',(73.3460458636487,33.0500221093637,44.7059404648168));
#46859=CARTESIAN_POINT('Ctrl Pts',(79.7906812734519,32.519632085483,46.7441805034492));
#46860=CARTESIAN_POINT('Ctrl Pts',(82.17248450487,32.0953200663783,51.0588374777756));
#46861=CARTESIAN_POINT('Ctrl Pts',(82.3168007726042,31.6710080472736,55.985136723764));
#46862=CARTESIAN_POINT('Ctrl Pts',(77.805234440245,31.1406180233928,61.0183779493088));
#46863=CARTESIAN_POINT('Ctrl Pts',(69.775937231011,30.5041499947359,59.7078492408087));
#46864=CARTESIAN_POINT('Ctrl Pts',(66.5521527695141,29.867681966079,52.255315154175));
#46865=CARTESIAN_POINT('Ctrl Pts',(71.0679482096409,29.2312139374221,45.5069344631459));
#46866=CARTESIAN_POINT('Ctrl Pts',(79.2019197609294,28.5947459087651,45.6669533075484));
#46867=CARTESIAN_POINT('Ctrl Pts',(82.7310720445922,28.0643558848842,51.4317457936056));
#46868=CARTESIAN_POINT('Ctrl Pts',(81.7000867943277,27.6400438657796,56.2511150970413));
#46869=CARTESIAN_POINT('Ctrl Pts',(78.5787338518511,27.215731846675,60.0650904415566));
#46870=CARTESIAN_POINT('Ctrl Pts',(71.8720769265383,26.6853418227943,60.9068148573381));
#46871=CARTESIAN_POINT('Ctrl Pts',(66.6693284787701,26.0488737941373,54.6523360552579));
#46872=CARTESIAN_POINT('Ctrl Pts',(69.1222134897098,25.4124057654804,46.9117666786429));
#46873=CARTESIAN_POINT('Ctrl Pts',(76.9567277562455,24.7759377368234,44.7778903714537));
#46874=CARTESIAN_POINT('Ctrl Pts',(82.992926824387,24.1394697081665,50.2323735386687));
#46875=CARTESIAN_POINT('Ctrl Pts',(81.8772919287,23.6090796842857,56.8989434446722));
#46876=CARTESIAN_POINT('Ctrl Pts',(77.9387078763277,23.1847676651811,59.8615040083881));
#46877=CARTESIAN_POINT('Ctrl Pts',(73.0811619366474,22.7604556460765,60.6942974202152));
#46878=CARTESIAN_POINT('Ctrl Pts',(67.4657179403036,22.2300656221957,56.9320340266631));
#46879=CARTESIAN_POINT('Ctrl Pts',(67.6388800071612,21.5935975935386,48.7983717706867));
#46880=CARTESIAN_POINT('Ctrl Pts',(74.5665295192065,20.9571295648818,44.5626166146362));
#46881=CARTESIAN_POINT('Ctrl Pts',(81.8807696047214,20.3206615362248,48.0889858384696));
#46882=CARTESIAN_POINT('Ctrl Pts',(82.8615055928374,19.6841935075679,56.1649530568178));
#46883=CARTESIAN_POINT('Ctrl Pts',(77.6476071831429,19.1538034836871,60.4671122954246));
#46884=CARTESIAN_POINT('Ctrl Pts',(72.7315637908718,18.7294914645825,60.1205020584682));
#46885=CARTESIAN_POINT('Ctrl Pts',(68.5176299076658,18.3051794454778,57.5653992266505));
#46886=CARTESIAN_POINT('Ctrl Pts',(66.7459211088642,17.774789421597,51.0396675832774));
#46887=CARTESIAN_POINT('Ctrl Pts',(72.2084562434742,17.1383213929401,45.0178404474499));
#46888=CARTESIAN_POINT('Ctrl Pts',(80.2192932876998,16.5018533642832,46.3527031218275));
#46889=CARTESIAN_POINT('Ctrl Pts',(83.4234792908833,15.8653853356262,53.8297790170139));
#46890=CARTESIAN_POINT('Ctrl Pts',(79.6377596034834,15.3349953117454,59.4154059749504));
#46891=CARTESIAN_POINT('Ctrl Pts',(74.8056885960671,14.9106832926407,60.4766449025428));
#46892=CARTESIAN_POINT('Ctrl Pts',(72.4431871575855,14.6985272830884,59.8257072724431));
#46893=CARTESIAN_POINT('Ctrl Pts',(71.4090089980051,14.5924492783123,59.2293593014411));
#46894=CARTESIAN_POINT('Ctrl Pts',(82.1675194498639,416.000000000001,49.6673071229103));
#46895=CARTESIAN_POINT('Ctrl Pts',(82.7266367873617,415.893921995224,50.8636168302151));
#46896=CARTESIAN_POINT('Ctrl Pts',(83.2199114808876,415.681765985672,53.5290146892342));
#46897=CARTESIAN_POINT('Ctrl Pts',(81.5919790563639,415.257453966567,58.7536428520482));
#46898=CARTESIAN_POINT('Ctrl Pts',(75.0770954668831,414.727063942687,62.3959325671766));
#46899=CARTESIAN_POINT('Ctrl Pts',(67.140757194596,414.090595914029,58.1554105274575));
#46900=CARTESIAN_POINT('Ctrl Pts',(66.4295467677559,413.454127885373,49.2002551082192));
#46901=CARTESIAN_POINT('Ctrl Pts',(73.5842173300634,412.817659856715,43.7513695000057));
#46902=CARTESIAN_POINT('Ctrl Pts',(80.6079888575398,412.287269832835,46.322952169211));
#46903=CARTESIAN_POINT('Ctrl Pts',(83.02416694298,411.86295781373,51.2093932239552));
#46904=CARTESIAN_POINT('Ctrl Pts',(82.9398220702424,411.438645794626,56.6601133855912));
#46905=CARTESIAN_POINT('Ctrl Pts',(77.7039374267809,410.908255770745,61.9981103880748));
#46906=CARTESIAN_POINT('Ctrl Pts',(68.8966609576623,410.271787742088,60.1511828265501));
#46907=CARTESIAN_POINT('Ctrl Pts',(65.7041703612452,409.635319713431,51.7558425715054));
#46908=CARTESIAN_POINT('Ctrl Pts',(71.029438885837,408.998851684774,44.5228669413054));
#46909=CARTESIAN_POINT('Ctrl Pts',(80.0097580407648,408.362383656117,45.1035870573125));
#46910=CARTESIAN_POINT('Ctrl Pts',(83.6233687599763,407.831993632237,51.6491061535822));
#46911=CARTESIAN_POINT('Ctrl Pts',(82.2447835214442,407.407681613132,56.9234798541325));
#46912=CARTESIAN_POINT('Ctrl Pts',(78.6062110227621,406.983369594028,60.983060830221));
#46913=CARTESIAN_POINT('Ctrl Pts',(71.1533325950583,406.452979570146,61.5801830353272));
#46914=CARTESIAN_POINT('Ctrl Pts',(65.7146841645151,405.81651154149,54.4104373561892));
#46915=CARTESIAN_POINT('Ctrl Pts',(68.8095528552745,405.180043512832,45.9786464084971));
#46916=CARTESIAN_POINT('Ctrl Pts',(77.5729088149027,404.543575484176,44.0096557413621));
#46917=CARTESIAN_POINT('Ctrl Pts',(83.9722721207543,403.907107455519,50.3367650503416));
#46918=CARTESIAN_POINT('Ctrl Pts',(82.4084379950837,403.376717431638,57.648147639214));
#46919=CARTESIAN_POINT('Ctrl Pts',(77.9090662557975,402.952405412533,60.7263149046133));
#46920=CARTESIAN_POINT('Ctrl Pts',(72.4999683740037,402.528093393429,61.4053720313486));
#46921=CARTESIAN_POINT('Ctrl Pts',(66.4815183774652,401.997703369548,56.9691401200638));
#46922=CARTESIAN_POINT('Ctrl Pts',(67.0767526293748,401.361235340891,47.9897268622084));
#46923=CARTESIAN_POINT('Ctrl Pts',(74.9423310373525,400.724767312234,43.6531386257255));
#46924=CARTESIAN_POINT('Ctrl Pts',(82.8497633290917,400.088299283577,47.9129315749583));
#46925=CARTESIAN_POINT('Ctrl Pts',(83.5324048115291,399.45183125492,56.8861231368181));
#46926=CARTESIAN_POINT('Ctrl Pts',(77.5574372048307,398.921441231039,61.3807483418143));
#46927=CARTESIAN_POINT('Ctrl Pts',(72.141983520554,398.497129211935,60.7543935454473));
#46928=CARTESIAN_POINT('Ctrl Pts',(67.6128520565103,398.07281719283,57.7201840750103));
#46929=CARTESIAN_POINT('Ctrl Pts',(65.9778985815363,397.542427168948,50.424375635435));
#46930=CARTESIAN_POINT('Ctrl Pts',(72.3153497046489,396.905959140293,44.0352536724918));
#46931=CARTESIAN_POINT('Ctrl Pts',(81.0974623299774,396.269491111635,45.9188192264581));
#46932=CARTESIAN_POINT('Ctrl Pts',(84.2742884644266,395.633023082978,54.3200749107313));
#46933=CARTESIAN_POINT('Ctrl Pts',(78.9057099164933,394.996555054322,61.5424381367421));
#46934=CARTESIAN_POINT('Ctrl Pts',(71.447374289968,394.46616503044,61.0179161312433));
#46935=CARTESIAN_POINT('Ctrl Pts',(67.7694391264492,394.041853011337,56.9939564067508));
#46936=CARTESIAN_POINT('Ctrl Pts',(66.3395721561712,393.617540992231,51.7332587934419));
#46937=CARTESIAN_POINT('Ctrl Pts',(69.8892509040224,393.087150968351,45.1528580123862));
#46938=CARTESIAN_POINT('Ctrl Pts',(78.8635348149744,392.450682939693,44.4847304204006));
#46939=CARTESIAN_POINT('Ctrl Pts',(84.2589006674125,391.814214911037,51.6654928227725));
#46940=CARTESIAN_POINT('Ctrl Pts',(81.1484592765518,391.177746882379,60.0915521457887));
#46941=CARTESIAN_POINT('Ctrl Pts',(72.3592921800129,390.541278853723,62.0240913931654));
#46942=CARTESIAN_POINT('Ctrl Pts',(67.0722118849917,390.010888829841,56.7374406948235));
#46943=CARTESIAN_POINT('Ctrl Pts',(66.9340026511513,389.586576810738,51.2876372911175));
#46944=CARTESIAN_POINT('Ctrl Pts',(69.3040424467103,389.162264791632,46.3782207984136));
#46945=CARTESIAN_POINT('Ctrl Pts',(76.2989923201939,388.631874767753,43.7376583735257));
#46946=CARTESIAN_POINT('Ctrl Pts',(83.5126631044287,387.995406739094,49.1179111566402));
#46947=CARTESIAN_POINT('Ctrl Pts',(82.8775247809523,387.358938710439,58.0772593846658));
#46948=CARTESIAN_POINT('Ctrl Pts',(75.0039483663863,386.722470681781,62.3993093386759));
#46949=CARTESIAN_POINT('Ctrl Pts',(67.1009304314964,386.086002653124,58.0950702985737));
#46950=CARTESIAN_POINT('Ctrl Pts',(66.5758023831447,385.555612629243,50.6367773179301));
#46951=CARTESIAN_POINT('Ctrl Pts',(70.045042324282,385.131300610139,46.4315623219777));
#46952=CARTESIAN_POINT('Ctrl Pts',(75.053657026783,384.706988591034,44.2790666324918));
#46953=CARTESIAN_POINT('Ctrl Pts',(82.0663161112484,384.176598567154,46.8722319217373));
#46954=CARTESIAN_POINT('Ctrl Pts',(83.9846374672821,383.540130538496,55.6645131597617));
#46955=CARTESIAN_POINT('Ctrl Pts',(77.6302160584578,382.90366250984,62.0123198612961));
#46956=CARTESIAN_POINT('Ctrl Pts',(68.8515981217496,382.267194481182,60.1125334305931));
#46957=CARTESIAN_POINT('Ctrl Pts',(65.7072493485604,381.630726452526,51.6806156780251));
#46958=CARTESIAN_POINT('Ctrl Pts',(70.2013890289615,381.100336428644,45.7052828684384));
#46959=CARTESIAN_POINT('Ctrl Pts',(75.5781324828351,380.67602440954,44.8052335572377));
#46960=CARTESIAN_POINT('Ctrl Pts',(80.7710747695743,380.251712390435,46.4643927834609));
#46961=CARTESIAN_POINT('Ctrl Pts',(84.3652035446419,379.721322366556,53.020621272502));
#46962=CARTESIAN_POINT('Ctrl Pts',(80.0481880045269,379.084854337897,60.9166673095976));
#46963=CARTESIAN_POINT('Ctrl Pts',(71.0881831371497,378.448386309242,61.542474098911));
#46964=CARTESIAN_POINT('Ctrl Pts',(65.7060922452434,377.811918280583,54.3517565413768));
#46965=CARTESIAN_POINT('Ctrl Pts',(68.8611599294873,377.175450251927,45.9238437451164));
#46966=CARTESIAN_POINT('Ctrl Pts',(76.1724154596052,376.645060228046,44.3594153429182));
#46967=CARTESIAN_POINT('Ctrl Pts',(80.8220300956532,376.220748208942,47.2055605724546));
#46968=CARTESIAN_POINT('Ctrl Pts',(83.6547311664345,375.796436189837,51.8633780415016));
#46969=CARTESIAN_POINT('Ctrl Pts',(82.0691877899781,375.266046165956,59.1700835818705));
#46970=CARTESIAN_POINT('Ctrl Pts',(73.6321954803594,374.629578137299,62.3007906842619));
#46971=CARTESIAN_POINT('Ctrl Pts',(66.4570562632811,373.993110108642,56.8979489711891));
#46972=CARTESIAN_POINT('Ctrl Pts',(67.1087450192595,373.356642079985,47.9397893875299));
#46973=CARTESIAN_POINT('Ctrl Pts',(75.017229542891,372.720174051328,43.6456027668752));
#46974=CARTESIAN_POINT('Ctrl Pts',(81.5630475868822,372.189784027447,47.2586568471847));
#46975=CARTESIAN_POINT('Ctrl Pts',(83.2071979870441,371.765472008343,52.4563706131603));
#46976=CARTESIAN_POINT('Ctrl Pts',(82.2916195454673,371.341159989238,57.8304914760256));
#46977=CARTESIAN_POINT('Ctrl Pts',(76.303328540101,370.810769965358,62.3073502505834));
#46978=CARTESIAN_POINT('Ctrl Pts',(67.8805296891691,370.1743019367,59.1386556123655));
#46979=CARTESIAN_POINT('Ctrl Pts',(66.0061117550362,369.537833908044,50.3545860105709));
#46980=CARTESIAN_POINT('Ctrl Pts',(72.3722492701013,368.901365879387,44.0185293109938));
#46981=CARTESIAN_POINT('Ctrl Pts',(81.1589519760789,368.26489785073,45.9622427030081));
#46982=CARTESIAN_POINT('Ctrl Pts',(83.731847557838,367.734507826849,52.9823639254405));
#46983=CARTESIAN_POINT('Ctrl Pts',(81.564891452265,367.310195807745,57.9847393779517));
#46984=CARTESIAN_POINT('Ctrl Pts',(77.3496717091796,366.885883788639,61.4418163873436));
#46985=CARTESIAN_POINT('Ctrl Pts',(69.8929268947405,366.35549376476,60.8951442510317));
#46986=CARTESIAN_POINT('Ctrl Pts',(65.6115368619148,365.719025736101,52.9797247687586));
#46987=CARTESIAN_POINT('Ctrl Pts',(69.9563147730001,365.082557707445,45.1186671895065));
#46988=CARTESIAN_POINT('Ctrl Pts',(78.9174604672025,364.446089678788,44.5094141975096));
#46989=CARTESIAN_POINT('Ctrl Pts',(84.2768512094807,363.809621650131,51.738597904202));
#46990=CARTESIAN_POINT('Ctrl Pts',(81.6160920770388,363.27923162625,58.7258902618615));
#46991=CARTESIAN_POINT('Ctrl Pts',(76.6998492575118,362.854919607146,61.081737343235));
#46992=CARTESIAN_POINT('Ctrl Pts',(71.2504678681829,362.430607588041,60.9277847368937));
#46993=CARTESIAN_POINT('Ctrl Pts',(65.979113088516,361.90021756416,55.6254538872424));
#46994=CARTESIAN_POINT('Ctrl Pts',(67.9370353160928,361.263749535503,46.8419063838533));
#46995=CARTESIAN_POINT('Ctrl Pts',(76.3720452392034,360.627281506846,43.7558200341216));
#46996=CARTESIAN_POINT('Ctrl Pts',(83.5371909925975,359.99081347819,49.1719078928615));
#46997=CARTESIAN_POINT('Ctrl Pts',(82.8431403597864,359.354345449532,58.1442241998485));
#46998=CARTESIAN_POINT('Ctrl Pts',(76.2525123631298,358.823955425652,61.6748780007709));
#46999=CARTESIAN_POINT('Ctrl Pts',(70.995967448003,358.399643406547,60.2298193560718));
#47000=CARTESIAN_POINT('Ctrl Pts',(66.9826497101512,357.975331387442,56.5402747139229));
#47001=CARTESIAN_POINT('Ctrl Pts',(66.4796762958856,357.444941363562,49.0804549173847));
#47002=CARTESIAN_POINT('Ctrl Pts',(73.7175186823536,356.808473334904,43.7327634732031));
#47003=CARTESIAN_POINT('Ctrl Pts',(82.1095617690253,356.172005306248,46.9338467574087));
#47004=CARTESIAN_POINT('Ctrl Pts',(83.9677487982834,355.53553727759,55.7213641727699));
#47005=CARTESIAN_POINT('Ctrl Pts',(77.5603452197334,354.899069248934,62.04033130159));
#47006=CARTESIAN_POINT('Ctrl Pts',(70.2692904454451,354.368679225053,60.3843077719843));
#47007=CARTESIAN_POINT('Ctrl Pts',(67.2481778544935,353.944367205949,55.8464296726782));
#47008=CARTESIAN_POINT('Ctrl Pts',(66.637470387959,353.520055186844,50.4291891092842));
#47009=CARTESIAN_POINT('Ctrl Pts',(71.1493379349456,352.989665162963,44.4672309669677));
#47010=CARTESIAN_POINT('Ctrl Pts',(80.1205199676786,352.353197134306,45.1757922763084));
#47011=CARTESIAN_POINT('Ctrl Pts',(84.3574513433622,351.716729105648,53.0954976924663));
#47012=CARTESIAN_POINT('Ctrl Pts',(79.9981583142393,351.080261076993,60.9485153065569));
#47013=CARTESIAN_POINT('Ctrl Pts',(71.0170629561984,350.443793048334,61.5178064125007));
#47014=CARTESIAN_POINT('Ctrl Pts',(66.5982362644239,349.913403024455,55.4865657175575));
#47015=CARTESIAN_POINT('Ctrl Pts',(67.292916921443,349.48909100535,50.0794520960279));
#47016=CARTESIAN_POINT('Ctrl Pts',(70.3840695694908,349.064778986245,45.5889917367961));
#47017=CARTESIAN_POINT('Ctrl Pts',(77.6999394516204,348.534388962364,44.046285828326));
#47018=CARTESIAN_POINT('Ctrl Pts',(84.0085351524569,347.897920933708,50.4639011546693));
#47019=CARTESIAN_POINT('Ctrl Pts',(82.0142363486943,347.26145290505,59.2215317498864));
#47020=CARTESIAN_POINT('Ctrl Pts',(73.5735395779143,346.624984876393,62.2920299805842));
#47021=CARTESIAN_POINT('Ctrl Pts',(66.4195359996401,345.988516847736,56.8326894530505));
#47022=CARTESIAN_POINT('Ctrl Pts',(67.0381855122534,345.458126823856,49.3815709844699));
#47023=CARTESIAN_POINT('Ctrl Pts',(71.1082622727451,345.033814804751,45.7547357118015));
#47024=CARTESIAN_POINT('Ctrl Pts',(76.3865941183634,344.609502785648,44.3914045492091));
#47025=CARTESIAN_POINT('Ctrl Pts',(82.9216519432451,344.079112761765,48.0238848145009));
#47026=CARTESIAN_POINT('Ctrl Pts',(83.4764165212709,343.44264473311,57.0058891819291));
#47027=CARTESIAN_POINT('Ctrl Pts',(76.2281043515981,342.806176704451,62.3101602960356));
#47028=CARTESIAN_POINT('Ctrl Pts',(67.8419892726382,342.169708675796,59.0935789985375));
#47029=CARTESIAN_POINT('Ctrl Pts',(66.0205765335468,341.533240647137,50.2807121649013));
#47030=CARTESIAN_POINT('Ctrl Pts',(71.373560763289,341.002850623258,45.0608028277178));
#47031=CARTESIAN_POINT('Ctrl Pts',(76.8246747903378,340.578538604152,44.9914141004164));
#47032=CARTESIAN_POINT('Ctrl Pts',(81.7037757041983,340.154226585048,47.4232515135116));
#47033=CARTESIAN_POINT('Ctrl Pts',(84.2558090592015,339.623836561167,54.4509836802375));
#47034=CARTESIAN_POINT('Ctrl Pts',(78.784904978247,338.987368532511,61.5961481101528));
#47035=CARTESIAN_POINT('Ctrl Pts',(69.8342902036576,338.350900503853,60.8479392369952));
#47036=CARTESIAN_POINT('Ctrl Pts',(65.6119969363752,337.714432475197,52.9204200206177));
#47037=CARTESIAN_POINT('Ctrl Pts',(70.0156767767625,337.077964446539,45.0723775859148));
#47038=CARTESIAN_POINT('Ctrl Pts',(77.4800055367938,336.547574422659,44.6414601756678));
#47039=CARTESIAN_POINT('Ctrl Pts',(81.641082531161,336.123262403554,48.1635188319527));
#47040=CARTESIAN_POINT('Ctrl Pts',(83.7301676223705,335.698950384449,53.1989118069898));
#47041=CARTESIAN_POINT('Ctrl Pts',(81.0486668554268,335.168560360569,60.1782704658609));
#47042=CARTESIAN_POINT('Ctrl Pts',(72.232865644344,334.532092331911,61.985427127637));
#47043=CARTESIAN_POINT('Ctrl Pts',(65.9657961792567,333.895624303255,55.5513645167554));
#47044=CARTESIAN_POINT('Ctrl Pts',(67.9762704426601,333.259156274598,46.7974331372456));
#47045=CARTESIAN_POINT('Ctrl Pts',(76.4472167768183,332.622688245941,43.7597968197546));
#47046=CARTESIAN_POINT('Ctrl Pts',(82.3653300504053,332.09229822206,48.3290231145748));
#47047=CARTESIAN_POINT('Ctrl Pts',(83.1974205860366,331.667986202955,53.7167020463484));
#47048=CARTESIAN_POINT('Ctrl Pts',(81.4728272659272,331.243674183851,58.8882817674393));
#47049=CARTESIAN_POINT('Ctrl Pts',(74.871741736091,330.71328415997,62.39934478027));
#47050=CARTESIAN_POINT('Ctrl Pts',(67.0308319601666,330.076816131312,57.9829774858364));
#47051=CARTESIAN_POINT('Ctrl Pts',(66.5182045234311,329.440348102657,49.0157853683406));
#47052=CARTESIAN_POINT('Ctrl Pts',(73.7763034444097,328.803880073998,43.7249138508815));
#47053=CARTESIAN_POINT('Ctrl Pts',(82.1637083950636,328.167412045343,46.9861412865685));
#47054=CARTESIAN_POINT('Ctrl Pts',(83.6356998168977,327.637022021461,54.316566574799));
#47055=CARTESIAN_POINT('Ctrl Pts',(80.7310751922223,327.212710002357,58.929875010303));
#47056=CARTESIAN_POINT('Ctrl Pts',(76.0378631809033,326.788397983252,61.7035404458194));
#47057=CARTESIAN_POINT('Ctrl Pts',(68.7517592205485,326.258007959371,60.0258686271432));
#47058=CARTESIAN_POINT('Ctrl Pts',(65.7278275580644,325.621539930714,51.5500203808521));
#47059=CARTESIAN_POINT('Ctrl Pts',(71.2208322668849,324.985071902058,44.4436696556311));
#47060=CARTESIAN_POINT('Ctrl Pts',(80.1700495252707,324.3486038734,45.208412634144));
#47061=CARTESIAN_POINT('Ctrl Pts',(84.364040928706,323.712135844744,53.1704853731638));
#47062=CARTESIAN_POINT('Ctrl Pts',(80.6686270260788,323.181745820862,59.6701630375215));
#47063=CARTESIAN_POINT('Ctrl Pts',(75.4505684539656,322.757433801758,61.2485557862883));
#47064=CARTESIAN_POINT('Ctrl Pts',(70.0884361107281,322.333121782653,60.2651964089632));
#47065=CARTESIAN_POINT('Ctrl Pts',(65.6875426553555,321.802731758773,54.2208576985052));
#47066=CARTESIAN_POINT('Ctrl Pts',(68.9623313898591,321.166263730115,45.8387383401391));
#47067=CARTESIAN_POINT('Ctrl Pts',(77.7693672924811,320.529795701459,44.0753779201171));
#47068=CARTESIAN_POINT('Ctrl Pts',(84.0245397640824,319.893327672802,50.5210073472171));
#47069=CARTESIAN_POINT('Ctrl Pts',(81.9700399621623,319.256859644145,59.2824682275405));
#47070=CARTESIAN_POINT('Ctrl Pts',(74.917992817877,318.726469620264,61.7665223185493));
#47071=CARTESIAN_POINT('Ctrl Pts',(69.9433762093293,318.302157601159,59.536578702821));
#47072=CARTESIAN_POINT('Ctrl Pts',(66.5397963443308,317.877845582055,55.2780457354786));
#47073=CARTESIAN_POINT('Ctrl Pts',(67.1805741364608,317.347455558174,47.8287976208435));
#47074=CARTESIAN_POINT('Ctrl Pts',(75.1494197109682,316.710987529517,43.6476893463325));
#47075=CARTESIAN_POINT('Ctrl Pts',(82.9549932889592,316.07451950086,48.0913750327353));
#47076=CARTESIAN_POINT('Ctrl Pts',(83.4510538437739,315.438051472203,57.0594988770483));
#47077=CARTESIAN_POINT('Ctrl Pts',(76.1547784530625,314.801583443546,62.3271863788299));
#47078=CARTESIAN_POINT('Ctrl Pts',(69.201637942207,314.271193419666,59.5784174382707));
#47079=CARTESIAN_POINT('Ctrl Pts',(66.9080513766019,313.846881400561,54.6328214582659));
#47080=CARTESIAN_POINT('Ctrl Pts',(67.130795872377,313.422569381456,49.1858182619233));
#47081=CARTESIAN_POINT('Ctrl Pts',(72.4992604523953,312.892179357576,43.9818311649589));
#47082=CARTESIAN_POINT('Ctrl Pts',(81.2573869801701,312.255711328918,46.050498832085));
#47083=CARTESIAN_POINT('Ctrl Pts',(84.2367264765035,311.619243300262,54.5238014660385));
#47084=CARTESIAN_POINT('Ctrl Pts',(78.7306028558601,310.982775271604,61.6199922776759));
#47085=CARTESIAN_POINT('Ctrl Pts',(69.767764865774,310.346307242948,60.8127120555743));
#47086=CARTESIAN_POINT('Ctrl Pts',(66.3206060972866,309.815917219067,54.1780311983573));
#47087=CARTESIAN_POINT('Ctrl Pts',(67.8319189521616,309.391605199962,48.9401506741324));
#47088=CARTESIAN_POINT('Ctrl Pts',(71.5718418442326,308.967293180858,44.9737372195454));
#47089=CARTESIAN_POINT('Ctrl Pts',(79.0374175729379,308.436903156977,44.5649919550533));
#47090=CARTESIAN_POINT('Ctrl Pts',(84.2932973842717,307.80043512832,51.8697776194207));
#47091=CARTESIAN_POINT('Ctrl Pts',(80.9865109093489,307.163967099662,60.2207347244622));
#47092=CARTESIAN_POINT('Ctrl Pts',(72.1762324002069,306.527499071007,61.9678220011371));
#47093=CARTESIAN_POINT('Ctrl Pts',(65.9386691644986,305.891031042348,55.4811455737152));
#47094=CARTESIAN_POINT('Ctrl Pts',(67.6866179108752,305.360641018469,48.2115810178204));
#47095=CARTESIAN_POINT('Ctrl Pts',(72.2622790062819,304.936328999363,45.2480047202793));
#47096=CARTESIAN_POINT('Ctrl Pts',(77.6867985749163,304.512016980259,44.7057442838956));
#47097=CARTESIAN_POINT('Ctrl Pts',(83.5913144144231,303.981626956378,49.2925281629657));
#47098=CARTESIAN_POINT('Ctrl Pts',(82.7695389938667,303.345158927721,58.2540487566874));
#47099=CARTESIAN_POINT('Ctrl Pts',(74.7969691643367,302.708690899064,62.3906478035181));
#47100=CARTESIAN_POINT('Ctrl Pts',(66.9996181792322,302.072222870408,57.9325496691043));
#47101=CARTESIAN_POINT('Ctrl Pts',(66.5437682104894,301.43575484175,48.9449823119422));
#47102=CARTESIAN_POINT('Ctrl Pts',(72.6303204709577,300.90536481787,44.602658598437));
#47103=CARTESIAN_POINT('Ctrl Pts',(78.028232009396,300.481052798765,45.365554367569));
#47104=CARTESIAN_POINT('Ctrl Pts',(82.4793053786608,300.05674077966,48.5131573909484));
#47105=CARTESIAN_POINT('Ctrl Pts',(83.9295177772661,299.52635075578,55.8479223940833));
#47106=CARTESIAN_POINT('Ctrl Pts',(77.4327613662142,298.889882727122,62.074986094495));
#47107=CARTESIAN_POINT('Ctrl Pts',(68.7010089731946,298.253414698466,59.9702719789989));
#47108=CARTESIAN_POINT('Ctrl Pts',(65.7373281557615,297.616946669808,51.4914797670529));
#47109=CARTESIAN_POINT('Ctrl Pts',(71.2865603157941,296.980478641152,44.4069763527274));
#47110=CARTESIAN_POINT('Ctrl Pts',(78.7292737431128,296.450088617271,45.1196547451927));
#47111=CARTESIAN_POINT('Ctrl Pts',(82.3044309221991,296.025776598167,49.2351996758424));
#47112=CARTESIAN_POINT('Ctrl Pts',(83.6010089300926,295.601464579062,54.5303242636882));
#47113=CARTESIAN_POINT('Ctrl Pts',(79.8863062500415,295.071074555181,61.0189972906718));
#47114=CARTESIAN_POINT('Ctrl Pts',(70.8980133686167,294.434606526524,61.4603104122333));
#47115=CARTESIAN_POINT('Ctrl Pts',(65.6856826182534,293.798138497867,54.1456040264796));
#47116=CARTESIAN_POINT('Ctrl Pts',(69.0078910237733,293.16167046921,45.8007701353069));
#47117=CARTESIAN_POINT('Ctrl Pts',(77.8430526165225,292.525202440553,44.0907742804756));
#47118=CARTESIAN_POINT('Ctrl Pts',(82.9949588197056,291.994812416672,49.5092386501921));
#47119=CARTESIAN_POINT('Ctrl Pts',(82.9955159782755,291.570500397568,54.9607942649627));
#47120=CARTESIAN_POINT('Ctrl Pts',(80.5022686396504,291.146188378463,59.8088017566861));
#47121=CARTESIAN_POINT('Ctrl Pts',(73.442874565269,290.615798354583,62.2718991877407));
#47122=CARTESIAN_POINT('Ctrl Pts',(66.3673555967205,289.979330325925,56.711215999567));
#47123=CARTESIAN_POINT('Ctrl Pts',(67.2285157374899,289.342862297269,47.7707616166553));
#47124=CARTESIAN_POINT('Ctrl Pts',(75.2087139229012,288.706394268612,43.6488981688282));
#47125=CARTESIAN_POINT('Ctrl Pts',(83.0005296951049,288.069926239954,48.1513167594931));
#47126=CARTESIAN_POINT('Ctrl Pts',(83.3371677688902,287.539536216074,55.6204913095729));
#47127=CARTESIAN_POINT('Ctrl Pts',(79.7628518963391,287.115224196969,59.73676692894));
#47128=CARTESIAN_POINT('Ctrl Pts',(74.7014834086863,286.690912177865,61.7621083726375));
#47129=CARTESIAN_POINT('Ctrl Pts',(67.7565378491218,286.160522153984,58.9926996222055));
#47130=CARTESIAN_POINT('Ctrl Pts',(66.0608339848255,285.524054125327,50.1547838838573));
#47131=CARTESIAN_POINT('Ctrl Pts',(72.5735120570497,284.88758609667,43.9694507733014));
#47132=CARTESIAN_POINT('Ctrl Pts',(81.3013612970727,284.251118068013,46.090292352582));
#47133=CARTESIAN_POINT('Ctrl Pts',(84.2318008882829,283.614650039356,54.5989168005053));
#47134=CARTESIAN_POINT('Ctrl Pts',(79.5882164210452,283.084260015475,60.4588670518221));
#47135=CARTESIAN_POINT('Ctrl Pts',(74.190460933948,282.659947996371,61.2228661571073));
#47136=CARTESIAN_POINT('Ctrl Pts',(69.0410682497914,282.235635977266,59.433113683797));
#47137=CARTESIAN_POINT('Ctrl Pts',(65.6136307451155,281.705245953385,52.7882234812563));
#47138=CARTESIAN_POINT('Ctrl Pts',(70.1286457211821,281.068777924728,45.0036999917018));
#47139=CARTESIAN_POINT('Ctrl Pts',(79.1015955077365,280.432309896071,44.6043336323989));
#47140=CARTESIAN_POINT('Ctrl Pts',(84.3004041615478,279.795841867414,51.9286568053638));
#47141=CARTESIAN_POINT('Ctrl Pts',(80.9335368906759,279.159373838757,60.2742167610446));
#47142=CARTESIAN_POINT('Ctrl Pts',(73.585110486313,278.628983814877,61.6535365325057));
#47143=CARTESIAN_POINT('Ctrl Pts',(69.0088437210826,278.204671795772,58.6908955780847));
#47144=CARTESIAN_POINT('Ctrl Pts',(66.2946561082543,277.780359776667,53.9630372327307));
#47145=CARTESIAN_POINT('Ctrl Pts',(68.0641889088541,277.249969752787,46.6986964285089));
#47146=CARTESIAN_POINT('Ctrl Pts',(76.5775418425126,276.613501724129,43.7820222916706));
#47147=CARTESIAN_POINT('Ctrl Pts',(83.6139711566449,275.977033695473,49.3643142822595));
#47148=CARTESIAN_POINT('Ctrl Pts',(82.7362958735918,275.340565666816,58.3031624999266));
#47149=CARTESIAN_POINT('Ctrl Pts',(74.7219042606049,274.704097638158,62.3962900653973));
#47150=CARTESIAN_POINT('Ctrl Pts',(68.2694031771755,274.173707614279,58.6191054762326));
#47151=CARTESIAN_POINT('Ctrl Pts',(66.7570197126837,273.749395595173,53.3815339790885));
#47152=CARTESIAN_POINT('Ctrl Pts',(67.8080032551739,273.32508357607,48.0322450053293));
#47153=CARTESIAN_POINT('Ctrl Pts',(73.9074260611533,272.794693552187,43.7080184749338));
#47154=CARTESIAN_POINT('Ctrl Pts',(82.247529620235,272.158225523532,47.0883792274754));
#47155=CARTESIAN_POINT('Ctrl Pts',(83.8995514050742,271.521757494873,55.9169773825275));
#47156=CARTESIAN_POINT('Ctrl Pts',(77.375457650676,270.885289466217,62.090268404729));
#47157=CARTESIAN_POINT('Ctrl Pts',(68.6406353786743,270.24882143756,59.9253097284314));
#47158=CARTESIAN_POINT('Ctrl Pts',(66.2458187949878,269.718431413679,52.8424609242579));
#47159=CARTESIAN_POINT('Ctrl Pts',(68.5383944154785,269.294119394575,47.8963962304133));
#47160=CARTESIAN_POINT('Ctrl Pts',(72.8395616968912,268.86980737547,44.5468561203877));
#47161=CARTESIAN_POINT('Ctrl Pts',(80.2801255265928,268.339417351589,45.2816374133041));
#47162=CARTESIAN_POINT('Ctrl Pts',(84.360285475917,267.702949322933,53.3026386588755));
#47163=CARTESIAN_POINT('Ctrl Pts',(79.8184004420758,267.066481294275,61.0514838438268));
#47164=CARTESIAN_POINT('Ctrl Pts',(70.8447281772513,266.430013265619,61.4342728777548));
#47165=CARTESIAN_POINT('Ctrl Pts',(65.6695837090906,265.793545236961,54.0720690007085));
#47166=CARTESIAN_POINT('Ctrl Pts',(68.5059242394298,265.263155213081,47.1541888305816));
#47167=CARTESIAN_POINT('Ctrl Pts',(73.4800849357431,264.838843193976,44.9232284323187));
#47168=CARTESIAN_POINT('Ctrl Pts',(78.9238415588416,264.414531174872,45.2147293068233));
#47169=CARTESIAN_POINT('Ctrl Pts',(84.0596313353204,263.88414115099,50.6484717578505));
#47170=CARTESIAN_POINT('Ctrl Pts',(81.8805480228633,263.247673122334,59.3797810589176));
#47171=CARTESIAN_POINT('Ctrl Pts',(73.3703035215419,262.611205093677,62.2518987251529));
#47172=CARTESIAN_POINT('Ctrl Pts',(66.3441989511637,261.97473706502,56.6566171480483));
#47173=CARTESIAN_POINT('Ctrl Pts',(67.2645800631255,261.338269036363,47.7046863617726));
#47174=CARTESIAN_POINT('Ctrl Pts',(73.9422560569281,260.807879012482,44.3415721838004));
#47175=CARTESIAN_POINT('Ctrl Pts',(79.1606371490594,260.383566993378,45.9188983100824));
#47176=CARTESIAN_POINT('Ctrl Pts',(83.0795139809074,259.959254974273,49.7086032205166));
#47177=CARTESIAN_POINT('Ctrl Pts',(83.3939659320291,259.428864950392,57.1787446932546));
#47178=CARTESIAN_POINT('Ctrl Pts',(76.0234015441845,258.792396921735,62.3419749610388));
#47179=CARTESIAN_POINT('Ctrl Pts',(67.7148617594967,258.155928893078,58.9300124748392));
#47180=CARTESIAN_POINT('Ctrl Pts',(66.0791527621555,257.519460864421,50.0983774372604));
#47181=CARTESIAN_POINT('Ctrl Pts',(72.6440679098571,256.882992835764,43.9432125087627));
#47182=CARTESIAN_POINT('Ctrl Pts',(79.8909833080085,256.352602811884,45.7828078078208));
#47183=CARTESIAN_POINT('Ctrl Pts',(82.796550848464,255.928290792779,50.3955224314691));
#47184=CARTESIAN_POINT('Ctrl Pts',(83.2702778056452,255.503978773674,55.8264562095043));
#47185=CARTESIAN_POINT('Ctrl Pts',(78.6093088355845,254.973588749794,61.6725884276815));
#47186=CARTESIAN_POINT('Ctrl Pts',(69.6588783577597,254.337120721137,60.7377299062148));
#47187=CARTESIAN_POINT('Ctrl Pts',(65.6232711108373,253.70065269248,52.7135666782166));
#47188=CARTESIAN_POINT('Ctrl Pts',(70.1794636249799,253.064184663823,44.9731254030021));
#47189=CARTESIAN_POINT('Ctrl Pts',(79.1720701519117,252.427716635165,44.6307892446532));
#47190=CARTESIAN_POINT('Ctrl Pts',(83.437198618748,251.897326611285,50.771682731245));
#47191=CARTESIAN_POINT('Ctrl Pts',(82.6062093610088,251.47301459218,56.159531632698));
#47192=CARTESIAN_POINT('Ctrl Pts',(79.4026577641557,251.048702573076,60.5705084063462));
#47193=CARTESIAN_POINT('Ctrl Pts',(72.0501669738483,250.518312549195,61.9279960971656));
#47194=CARTESIAN_POINT('Ctrl Pts',(65.9056280140869,249.881844520538,55.3531343369834));
#47195=CARTESIAN_POINT('Ctrl Pts',(68.1204219004477,249.245376491881,46.6486521925987));
#47196=CARTESIAN_POINT('Ctrl Pts',(76.6359578349168,248.608908463224,43.7922612687687));
#47197=CARTESIAN_POINT('Ctrl Pts',(83.6498316490372,247.972440434567,49.4305003833438));
#47198=CARTESIAN_POINT('Ctrl Pts',(82.8432379943956,247.442050410686,56.863622226054));
#47199=CARTESIAN_POINT('Ctrl Pts',(78.6828810081231,247.017738391582,60.3865313475242));
#47200=CARTESIAN_POINT('Ctrl Pts',(73.3718078452896,246.593426372477,61.6161494957285));
#47201=CARTESIAN_POINT('Ctrl Pts',(66.9305540631015,246.063036348596,57.8198166117822));
#47202=CARTESIAN_POINT('Ctrl Pts',(66.602762753682,245.426568319939,48.8266681613785));
#47203=CARTESIAN_POINT('Ctrl Pts',(73.9826972194987,244.790100291282,43.7071087427155));
#47204=CARTESIAN_POINT('Ctrl Pts',(82.2849195603449,244.153632262626,47.1344146181999));
#47205=CARTESIAN_POINT('Ctrl Pts',(83.8832259174092,243.517164233968,55.9904624377692));
#47206=CARTESIAN_POINT('Ctrl Pts',(78.4001452382172,242.986774210088,61.0735441720867));
#47207=CARTESIAN_POINT('Ctrl Pts',(72.9490171417447,242.562462190983,61.0052696731008));
#47208=CARTESIAN_POINT('Ctrl Pts',(68.1328759584309,242.138150171878,58.4510098911372));
#47209=CARTESIAN_POINT('Ctrl Pts',(65.7591071269122,241.607760147998,51.3610793423386));
#47210=CARTESIAN_POINT('Ctrl Pts',(71.4086829187869,240.971292119341,44.3563338390819));
#47211=CARTESIAN_POINT('Ctrl Pts',(80.3375515915834,240.334824090684,45.3303079583086));
#47212=CARTESIAN_POINT('Ctrl Pts',(84.3583280981011,239.698356062027,53.3619128817103));
#47213=CARTESIAN_POINT('Ctrl Pts',(79.7578885484422,239.06188803337,61.0962597929539));
#47214=CARTESIAN_POINT('Ctrl Pts',(72.2850589701853,238.531498009489,61.3385648622608));
#47215=CARTESIAN_POINT('Ctrl Pts',(68.2142409568424,238.107185990385,57.7125616033534));
#47216=CARTESIAN_POINT('Ctrl Pts',(66.2529660476571,237.68287397128,52.6260245041113));
#47217=CARTESIAN_POINT('Ctrl Pts',(69.1098412727704,237.152483947399,45.7165992313107));
#47218=CARTESIAN_POINT('Ctrl Pts',(77.9684625670151,236.516015918742,44.1326184995208));
#47219=CARTESIAN_POINT('Ctrl Pts',(84.0710732356509,235.879547890085,50.7228737592228));
#47220=CARTESIAN_POINT('Ctrl Pts',(81.8402024524585,235.243079861428,59.4232494355754));
#47221=CARTESIAN_POINT('Ctrl Pts',(73.295256365372,234.606611832771,62.2460251195998));
#47222=CARTESIAN_POINT('Ctrl Pts',(67.4944033500437,234.076221808891,57.5288227763841));
#47223=CARTESIAN_POINT('Ctrl Pts',(66.7986174745077,233.651909789786,52.1218512629794));
#47224=CARTESIAN_POINT('Ctrl Pts',(68.6532437724353,233.227597770681,46.9954665499086));
#47225=CARTESIAN_POINT('Ctrl Pts',(75.3408792960931,232.697207746801,43.6522009674354));
#47226=CARTESIAN_POINT('Ctrl Pts',(83.0677754633829,232.060739718143,48.2651438256912));
#47227=CARTESIAN_POINT('Ctrl Pts',(83.3538170768646,231.424271689487,57.2424207823375));
#47228=CARTESIAN_POINT('Ctrl Pts',(75.9644373210915,230.787803660829,62.3483377602821));
#47229=CARTESIAN_POINT('Ctrl Pts',(67.6620528386393,230.151335632173,58.8763674119568));
#47230=CARTESIAN_POINT('Ctrl Pts',(66.3756246135881,229.620945608292,51.5111114032393));
#47231=CARTESIAN_POINT('Ctrl Pts',(69.3958095830978,229.196633589187,46.9726158727042));
#47232=CARTESIAN_POINT('Ctrl Pts',(74.1575605310016,228.772321570083,44.3183387878161));
#47233=CARTESIAN_POINT('Ctrl Pts',(81.3989800721073,228.241931546202,46.1794504652647));
#47234=CARTESIAN_POINT('Ctrl Pts',(84.2079316976986,227.605463517545,54.7289508578227));
#47235=CARTESIAN_POINT('Ctrl Pts',(78.5372423724498,226.968995488888,61.6943369888106));
#47236=CARTESIAN_POINT('Ctrl Pts',(69.6101882604234,226.332527460231,60.703869323161));
#47237=CARTESIAN_POINT('Ctrl Pts',(65.6185770686265,225.696059431574,52.6384365187058));
#47238=CARTESIAN_POINT('Ctrl Pts',(69.4769301814605,225.165669407694,46.2341406960417));
#47239=CARTESIAN_POINT('Ctrl Pts',(74.7331795982254,224.741357388588,44.788007625873));
#47240=CARTESIAN_POINT('Ctrl Pts',(80.0687724266707,224.317045369484,45.9064477808886));
#47241=CARTESIAN_POINT('Ctrl Pts',(84.3156425901752,223.786655345603,52.0599822937235));
#47242=CARTESIAN_POINT('Ctrl Pts',(80.8302488352503,223.150187316947,60.3567404403693));
#47243=CARTESIAN_POINT('Ctrl Pts',(71.9814957245066,222.513719288289,61.8971602273444));
#47244=CARTESIAN_POINT('Ctrl Pts',(65.8910706731163,221.877251259633,55.2956422237384));
#47245=CARTESIAN_POINT('Ctrl Pts',(68.1661423876409,221.240783230975,46.5888511265689));
#47246=CARTESIAN_POINT('Ctrl Pts',(75.2786649412196,220.710393207095,44.2836537842132));
#47247=CARTESIAN_POINT('Ctrl Pts',(80.1953873273415,220.28608118799,46.6384960022359));
#47248=CARTESIAN_POINT('Ctrl Pts',(83.4903573672587,219.861769168885,50.9816117272898));
#47249=CARTESIAN_POINT('Ctrl Pts',(82.6616815663088,219.331379145005,58.412305433049));
#47250=CARTESIAN_POINT('Ctrl Pts',(74.5898182217719,218.694911116348,62.3908659254138));
#47251=CARTESIAN_POINT('Ctrl Pts',(66.8989104837742,218.058443087691,57.7515067942423));
#47252=CARTESIAN_POINT('Ctrl Pts',(66.6295031705657,217.421975059034,48.773714540667));
#47253=CARTESIAN_POINT('Ctrl Pts',(74.0563658043794,216.785507030377,43.6919424072075));
#47254=CARTESIAN_POINT('Ctrl Pts',(80.9380581568106,216.255117006496,46.6153945638555));
#47255=CARTESIAN_POINT('Ctrl Pts',(83.1057762484532,215.830804987391,51.6173385382644));
#47256=CARTESIAN_POINT('Ctrl Pts',(82.7460769485554,215.406492968287,57.0569580266549));
#47257=CARTESIAN_POINT('Ctrl Pts',(77.246790500885,214.876102944406,62.1237819597051));
#47258=CARTESIAN_POINT('Ctrl Pts',(68.545751476127,214.239634915749,59.8345390185409));
#47259=CARTESIAN_POINT('Ctrl Pts',(65.7776657511149,213.603166887092,51.2888705940134));
#47260=CARTESIAN_POINT('Ctrl Pts',(71.467994410054,212.966698858435,44.333676878713));
#47261=CARTESIAN_POINT('Ctrl Pts',(80.3946783686388,212.330230829778,45.3675402002628));
#47262=CARTESIAN_POINT('Ctrl Pts',(84.3546705587473,211.693762801122,53.4303690622235));
#47263=CARTESIAN_POINT('Ctrl Pts',(79.7000908952398,211.057294772464,61.1299535646553));
#47264=CARTESIAN_POINT('Ctrl Pts',(72.2248594979382,210.526904748583,61.3190877996643));
#47265=CARTESIAN_POINT('Ctrl Pts',(68.1806921804899,210.102592729479,57.6634682251856));
#47266=CARTESIAN_POINT('Ctrl Pts',(66.2559726813135,209.678280710374,52.5630858770229));
#47267=CARTESIAN_POINT('Ctrl Pts',(69.1627565133466,209.147890686494,45.6743363606337));
#47268=CARTESIAN_POINT('Ctrl Pts',(78.0325037599698,208.511422657836,44.1543757101699));
#47269=CARTESIAN_POINT('Ctrl Pts',(84.0874436263853,207.87495462918,50.7884572037047));
#47270=CARTESIAN_POINT('Ctrl Pts',(81.7938378778077,207.238486600523,59.4725281184584));
#47271=CARTESIAN_POINT('Ctrl Pts',(73.2287589465603,206.602018571866,62.2335685646996));
#47272=CARTESIAN_POINT('Ctrl Pts',(67.4620855006973,206.071628547985,57.4746411749747));
#47273=CARTESIAN_POINT('Ctrl Pts',(66.8053318710369,205.64731652888,52.0627878477779));
#47274=CARTESIAN_POINT('Ctrl Pts',(68.69689543346,205.223004509776,46.9499189678551));
#47275=CARTESIAN_POINT('Ctrl Pts',(75.408479543298,204.692614485895,43.654990956662));
#47276=CARTESIAN_POINT('Ctrl Pts',(83.1018916223794,204.056146457238,48.3235638753832));
#47277=CARTESIAN_POINT('Ctrl Pts',(83.3231548698706,203.419678428581,57.3026707259473));
#47278=CARTESIAN_POINT('Ctrl Pts',(75.8971280409304,202.783210399924,62.3551404458827));
#47279=CARTESIAN_POINT('Ctrl Pts',(67.6200100548619,202.146742371267,58.8233585704684));
#47280=CARTESIAN_POINT('Ctrl Pts',(66.3867557005124,201.616352347387,51.4490127090517));
#47281=CARTESIAN_POINT('Ctrl Pts',(69.4396073911285,201.192040328282,46.9324259705503));
#47282=CARTESIAN_POINT('Ctrl Pts',(74.2203850355754,200.767728309177,44.3125740849968));
#47283=CARTESIAN_POINT('Ctrl Pts',(81.4481881519756,200.237338285296,46.225884263212));
#47284=CARTESIAN_POINT('Ctrl Pts',(84.1953818886021,199.600870256639,54.795428755371));
#47285=CARTESIAN_POINT('Ctrl Pts',(78.4745848027485,198.964402227983,61.7197194784877));
#47286=CARTESIAN_POINT('Ctrl Pts',(69.5549092843256,198.327934199325,60.6648687671083));
#47287=CARTESIAN_POINT('Ctrl Pts',(65.6215942106805,197.691466170669,52.570846359881));
#47288=CARTESIAN_POINT('Ctrl Pts',(69.5260539756305,197.161076146787,46.1945553070724));
#47289=CARTESIAN_POINT('Ctrl Pts',(74.7926004648802,196.736764127683,44.7863837941532));
#47290=CARTESIAN_POINT('Ctrl Pts',(80.1199848267535,196.312452108578,45.9432912198386));
#47291=CARTESIAN_POINT('Ctrl Pts',(84.3223466667195,195.782062084698,52.1273067937318));
#47292=CARTESIAN_POINT('Ctrl Pts',(80.7771822922816,195.145594056041,60.3987018243377));
#47293=CARTESIAN_POINT('Ctrl Pts',(71.9175455395786,194.509126027384,61.8752376250712));
#47294=CARTESIAN_POINT('Ctrl Pts',(65.8749087090707,193.872657998727,55.2299489559789));
#47295=CARTESIAN_POINT('Ctrl Pts',(68.2127415241208,193.236189970069,46.5397991343424));
#47296=CARTESIAN_POINT('Ctrl Pts',(75.3417097194792,192.705799946189,44.28597879505));
#47297=CARTESIAN_POINT('Ctrl Pts',(80.2413157837291,192.281487927084,46.676233874856));
#47298=CARTESIAN_POINT('Ctrl Pts',(83.5048607349508,191.85717590798,51.0430099491149));
#47299=CARTESIAN_POINT('Ctrl Pts',(82.6226020895228,191.326785884099,58.467531033659));
#47300=CARTESIAN_POINT('Ctrl Pts',(74.5222286308205,190.690317855442,62.3877499080446));
#47301=CARTESIAN_POINT('Ctrl Pts',(66.8650204224245,190.053849826785,57.6930205426558));
#47302=CARTESIAN_POINT('Ctrl Pts',(66.6603458363777,189.417381798128,48.7135200178606));
#47303=CARTESIAN_POINT('Ctrl Pts',(74.1237762701942,188.780913769471,43.6854615105328));
#47304=CARTESIAN_POINT('Ctrl Pts',(80.9840213044134,188.250523745591,46.658495604309));
#47305=CARTESIAN_POINT('Ctrl Pts',(83.1158544222917,187.826211726486,51.6759398231201));
#47306=CARTESIAN_POINT('Ctrl Pts',(82.7164059182478,187.401899707381,57.1128414981536));
#47307=CARTESIAN_POINT('Ctrl Pts',(77.1818381244577,186.8715096835,62.1398140451468));
#47308=CARTESIAN_POINT('Ctrl Pts',(68.4954808173363,186.235041654843,59.787929072078));
#47309=CARTESIAN_POINT('Ctrl Pts',(65.7927731055032,185.598573626187,51.2223764112526));
#47310=CARTESIAN_POINT('Ctrl Pts',(71.5263523783918,184.96210559753,44.3086661134114));
#47311=CARTESIAN_POINT('Ctrl Pts',(80.4582605987755,184.325637568872,45.4064738088519));
#47312=CARTESIAN_POINT('Ctrl Pts',(83.6882266308899,183.795247544992,52.1495601262344));
#47313=CARTESIAN_POINT('Ctrl Pts',(82.0076774577441,183.370935525887,57.3356196523102));
#47314=CARTESIAN_POINT('Ctrl Pts',(78.1409673484235,182.946623506783,61.1785367554813));
#47315=CARTESIAN_POINT('Ctrl Pts',(70.6660574864011,182.416233482902,61.3447180026869));
#47316=CARTESIAN_POINT('Ctrl Pts',(65.6500767081934,181.779765454245,53.8731650833682));
#47317=CARTESIAN_POINT('Ctrl Pts',(69.2262103655614,181.143297425588,45.6339545977931));
#47318=CARTESIAN_POINT('Ctrl Pts',(78.0885597547107,180.506829396931,44.1737886258499));
#47319=CARTESIAN_POINT('Ctrl Pts',(84.1122641563528,179.870361368274,50.8595310285428));
#47320=CARTESIAN_POINT('Ctrl Pts',(82.1292509872868,179.339971344393,58.0685221107672));
#47321=CARTESIAN_POINT('Ctrl Pts',(77.4597973815361,178.915659325288,60.8820007325289));
#47322=CARTESIAN_POINT('Ctrl Pts',(72.0205337842822,178.491347306184,61.2478838435807));
#47323=CARTESIAN_POINT('Ctrl Pts',(66.268026665914,177.960957282303,56.4718441132811));
#47324=CARTESIAN_POINT('Ctrl Pts',(67.3802791548321,177.324489253646,47.5417231401684));
#47325=CARTESIAN_POINT('Ctrl Pts',(75.4829300407876,176.688021224989,43.6661109328775));
#47326=CARTESIAN_POINT('Ctrl Pts',(83.1314521309226,176.051553196332,48.3749782274283));
#47327=CARTESIAN_POINT('Ctrl Pts',(83.2953061451401,175.415085167676,57.372606695839));
#47328=CARTESIAN_POINT('Ctrl Pts',(77.0710005685769,174.884695143794,61.5150593198097));
#47329=CARTESIAN_POINT('Ctrl Pts',(71.7006991468909,174.46038312469,60.5773378411154));
#47330=CARTESIAN_POINT('Ctrl Pts',(67.3541495885463,174.036071105585,57.2869023276584));
#47331=CARTESIAN_POINT('Ctrl Pts',(66.1428036994951,173.505681081705,49.9089259933674));
#47332=CARTESIAN_POINT('Ctrl Pts',(72.8382799358942,172.869213053048,43.8960428112868));
#47333=CARTESIAN_POINT('Ctrl Pts',(81.4971068633349,172.232745024391,46.2830990740509));
#47334=CARTESIAN_POINT('Ctrl Pts',(84.1839859454567,171.596276995734,54.8536301053831));
#47335=CARTESIAN_POINT('Ctrl Pts',(78.4077002508318,170.959808967077,61.7542597699573));
#47336=CARTESIAN_POINT('Ctrl Pts',(70.9920444572424,170.429418943196,60.8003505482352));
#47337=CARTESIAN_POINT('Ctrl Pts',(67.5523709208179,170.005106924091,56.5709173835918));
#47338=CARTESIAN_POINT('Ctrl Pts',(66.4283673509715,169.580794904987,51.2364938058905));
#47339=CARTESIAN_POINT('Ctrl Pts',(70.3517484936913,169.050404881106,44.8718277454255));
#47340=CARTESIAN_POINT('Ctrl Pts',(79.3496302067614,168.413936852449,44.7225264690454));
#47341=CARTESIAN_POINT('Ctrl Pts',(84.3217628279609,167.777468823792,52.2025811853009));
#47342=CARTESIAN_POINT('Ctrl Pts',(80.7304141405317,167.141000795135,60.4351710552188));
#47343=CARTESIAN_POINT('Ctrl Pts',(71.8443988490916,166.504532766478,61.8574573955251));
#47344=CARTESIAN_POINT('Ctrl Pts',(66.8711028478376,165.974142742598,56.2746068211148));
#47345=CARTESIAN_POINT('Ctrl Pts',(67.0475151664259,165.549830723493,50.8259062764698));
#47346=CARTESIAN_POINT('Ctrl Pts',(69.6968251956563,165.125518704388,46.0613900050752));
#47347=CARTESIAN_POINT('Ctrl Pts',(76.8324561509156,164.595128680507,43.8287537779593));
#47348=CARTESIAN_POINT('Ctrl Pts',(83.7237343798985,163.95866065185,49.6161928112686));
#47349=CARTESIAN_POINT('Ctrl Pts',(82.5728017822342,163.322192623194,58.5239801637262));
#47350=CARTESIAN_POINT('Ctrl Pts',(74.46300490994,162.685724594536,62.3846169053924));
#47351=CARTESIAN_POINT('Ctrl Pts',(66.8214538524927,162.04925656588,57.6316321978683));
#47352=CARTESIAN_POINT('Ctrl Pts',(66.7274586184903,161.518866541999,50.1554661651839));
#47353=CARTESIAN_POINT('Ctrl Pts',(70.4335138360439,161.094554522894,46.1573899208122));
#47354=CARTESIAN_POINT('Ctrl Pts',(75.5579617346419,160.670242503789,44.2974187742837));
#47355=CARTESIAN_POINT('Ctrl Pts',(82.4093461241096,160.139852479909,47.2908157743563));
#47356=CARTESIAN_POINT('Ctrl Pts',(83.8172586007792,159.503384451252,56.179119811211));
#47357=CARTESIAN_POINT('Ctrl Pts',(77.1072237588872,158.866916422595,62.1497775456292));
#47358=CARTESIAN_POINT('Ctrl Pts',(68.4528214593998,158.230448393938,59.7467290235218));
#47359=CARTESIAN_POINT('Ctrl Pts',(65.8001345025756,157.593980365281,51.1474605602964));
#47360=CARTESIAN_POINT('Ctrl Pts',(70.631498190644,157.0635903414,45.4413394113987));
#47361=CARTESIAN_POINT('Ctrl Pts',(76.0512099245549,156.639278322296,44.8529656758553));
#47362=CARTESIAN_POINT('Ctrl Pts',(81.1397894996918,156.214966303191,46.8089352152041));
#47363=CARTESIAN_POINT('Ctrl Pts',(84.3497132445386,155.68457627931,53.5615853027291));
#47364=CARTESIAN_POINT('Ctrl Pts',(79.5843755134694,155.048108250653,61.1954390151329));
#47365=CARTESIAN_POINT('Ctrl Pts',(70.6031904907703,154.411640221996,61.3033137063913));
#47366=CARTESIAN_POINT('Ctrl Pts',(65.6448850210462,153.775172193339,53.8140862275469));
#47367=CARTESIAN_POINT('Ctrl Pts',(69.280892606685,153.138704164683,45.5822203983009));
#47368=CARTESIAN_POINT('Ctrl Pts',(76.670221815505,152.608314140801,44.4421732519235));
#47369=CARTESIAN_POINT('Ctrl Pts',(81.1479030539253,152.184002121697,47.5518082238235));
#47370=CARTESIAN_POINT('Ctrl Pts',(83.7071837783121,151.759690102592,52.3652831749524));
#47371=CARTESIAN_POINT('Ctrl Pts',(81.7027675047384,151.229300078712,59.5683525939235));
#47372=CARTESIAN_POINT('Ctrl Pts',(73.099219904014,150.592832050055,62.2071278544567));
#47373=CARTESIAN_POINT('Ctrl Pts',(66.2477121959153,149.956364021397,56.3993603413037));
#47374=CARTESIAN_POINT('Ctrl Pts',(67.4150990922498,149.319895992741,47.4937144245136));
#47375=CARTESIAN_POINT('Ctrl Pts',(75.5581385426594,148.683427964083,43.6629084123797));
#47376=CARTESIAN_POINT('Ctrl Pts',(81.884623426692,148.153037940203,47.6475643152638));
#47377=CARTESIAN_POINT('Ctrl Pts',(83.2261870129823,147.728725921098,52.931470642528));
#47378=CARTESIAN_POINT('Ctrl Pts',(82.0021079857598,147.304413901994,58.2438231785031));
#47379=CARTESIAN_POINT('Ctrl Pts',(75.7655261202681,146.774023878113,62.3677703516982));
#47380=CARTESIAN_POINT('Ctrl Pts',(67.5395518392587,146.137555849456,58.7184535222492));
#47381=CARTESIAN_POINT('Ctrl Pts',(66.1749959513619,145.501087820799,49.8408801719592));
#47382=CARTESIAN_POINT('Ctrl Pts',(72.8960495469659,144.864619792142,43.8826287568211));
#47383=CARTESIAN_POINT('Ctrl Pts',(81.5559890678473,144.228151763485,46.3299974842915));
#47384=CARTESIAN_POINT('Ctrl Pts',(83.7196190431261,143.697761739604,53.4868542651944));
#47385=CARTESIAN_POINT('Ctrl Pts',(81.2676918241373,143.2734497205,58.3558902934191));
#47386=CARTESIAN_POINT('Ctrl Pts',(76.8600581518627,142.849137701395,61.5640399692282));
#47387=CARTESIAN_POINT('Ctrl Pts',(69.4472683305171,142.318747677514,60.5881092765891));
#47388=CARTESIAN_POINT('Ctrl Pts',(65.6296376629961,141.682279648857,52.4388846337205));
#47389=CARTESIAN_POINT('Ctrl Pts',(70.4206730961357,141.0458116202,44.8415626819159));
#47390=CARTESIAN_POINT('Ctrl Pts',(79.4020420808101,140.409343591544,44.7502800324071));
#47391=CARTESIAN_POINT('Ctrl Pts',(84.3354661478493,139.772875562886,52.2766000607004));
#47392=CARTESIAN_POINT('Ctrl Pts',(81.2760512437821,139.242485539006,59.0987605760395));
#47393=CARTESIAN_POINT('Ctrl Pts',(76.2320903429111,138.818173519901,61.1670732607779));
#47394=CARTESIAN_POINT('Ctrl Pts',(70.8006655095353,138.393861500797,60.6990100057015));
#47395=CARTESIAN_POINT('Ctrl Pts',(65.8439734003519,137.863471476916,55.1014125758177));
#47396=CARTESIAN_POINT('Ctrl Pts',(68.3053452812459,137.227003448259,46.4454426903871));
#47397=CARTESIAN_POINT('Ctrl Pts',(76.9043396893177,136.590535419602,43.8510995112914));
#47398=CARTESIAN_POINT('Ctrl Pts',(83.745106425328,135.954067390945,49.6715146016838));
#47399=CARTESIAN_POINT('Ctrl Pts',(82.534611519294,135.317599362288,58.588849869352));
#47400=CARTESIAN_POINT('Ctrl Pts',(75.7512809928387,134.787209338407,61.7334198910148));
#47401=CARTESIAN_POINT('Ctrl Pts',(70.586853554311,134.362897319302,59.9875252310921));
#47402=CARTESIAN_POINT('Ctrl Pts',(66.7930640514994,133.938585300198,56.0726024809321));
#47403=CARTESIAN_POINT('Ctrl Pts',(66.7212746356957,133.408195276317,48.5961902443));
#47404=CARTESIAN_POINT('Ctrl Pts',(74.2555640080234,132.77172724766,43.6749454985511));
#47405=CARTESIAN_POINT('Ctrl Pts',(82.4489652898005,132.135259219003,47.3548227786709));
#47406=CARTESIAN_POINT('Ctrl Pts',(83.7971184038797,131.498791190346,56.2349018628892));
#47407=CARTESIAN_POINT('Ctrl Pts',(77.0358533411102,130.862323161689,62.1737115874476));
#47408=CARTESIAN_POINT('Ctrl Pts',(69.8524745233392,130.331933137809,60.0998354067952));
#47409=CARTESIAN_POINT('Ctrl Pts',(67.0981769230303,129.907621118704,55.39523088991));
#47410=CARTESIAN_POINT('Ctrl Pts',(66.8009993906768,129.483309099599,49.9517812074355));
#47411=CARTESIAN_POINT('Ctrl Pts',(71.6492898563576,128.952919075718,44.2600351473352));
#47412=CARTESIAN_POINT('Ctrl Pts',(80.5646556385358,128.316451047062,45.4849511295538));
#47413=CARTESIAN_POINT('Ctrl Pts',(84.3376544397274,127.679983018405,53.6358898121339));
#47414=CARTESIAN_POINT('Ctrl Pts',(79.5325918757471,127.043514989748,61.2243478318641));
#47415=CARTESIAN_POINT('Ctrl Pts',(70.5336117950437,126.407046961091,61.2745842791024));
#47416=CARTESIAN_POINT('Ctrl Pts',(66.4700777659095,125.87665693721,54.9984720393197));
#47417=CARTESIAN_POINT('Ctrl Pts',(67.475530190837,125.452344918105,49.6404384118989));
#47418=CARTESIAN_POINT('Ctrl Pts',(70.8205831694898,125.028032899,45.3357805275401));
#47419=CARTESIAN_POINT('Ctrl Pts',(78.2132659060374,124.49764287512,44.2176858942317));
#47420=CARTESIAN_POINT('Ctrl Pts',(84.1411323737424,123.861174846463,50.9885473855479));
#47421=CARTESIAN_POINT('Ctrl Pts',(81.6449396066654,123.224706817806,59.6165450113336));
#47422=CARTESIAN_POINT('Ctrl Pts',(73.0411670779897,122.588238789149,62.1949979652921));
#47423=CARTESIAN_POINT('Ctrl Pts',(66.2140191459775,121.951770760492,56.3320450140946));
#47424=CARTESIAN_POINT('Ctrl Pts',(67.2614827699121,121.421380736611,48.9290244407872));
#47425=CARTESIAN_POINT('Ctrl Pts',(71.5340082887178,120.997068717507,45.5430261208643));
#47426=CARTESIAN_POINT('Ctrl Pts',(76.8821983753521,120.572756698402,44.4864648455043));
#47427=CARTESIAN_POINT('Ctrl Pts',(83.1968202911535,120.042366674521,48.4898938398491));
#47428=CARTESIAN_POINT('Ctrl Pts',(83.2325019630988,119.405898645864,57.4889434014319));
#47429=CARTESIAN_POINT('Ctrl Pts',(75.690265100545,118.769430617208,62.3662361412734));
#47430=CARTESIAN_POINT('Ctrl Pts',(67.5036760124128,118.13296258855,58.6712286361326));
#47431=CARTESIAN_POINT('Ctrl Pts',(66.1936983173821,117.496494559894,49.7679638061925));
#47432=CARTESIAN_POINT('Ctrl Pts',(71.8388969564375,116.966104536013,44.8655535848941));
#47433=CARTESIAN_POINT('Ctrl Pts',(77.2849357849202,116.541792516908,45.1107474062347));
#47434=CARTESIAN_POINT('Ctrl Pts',(82.0156219478191,116.117480497803,47.8200032744614));
#47435=CARTESIAN_POINT('Ctrl Pts',(84.1579853752027,115.587090473923,54.9832548125056));
#47436=CARTESIAN_POINT('Ctrl Pts',(78.2839980460653,114.950622445266,61.8009112317351));
#47437=CARTESIAN_POINT('Ctrl Pts',(69.3914524812726,114.314154416609,60.5376002094376));
#47438=CARTESIAN_POINT('Ctrl Pts',(65.6335181775654,113.677686387952,52.3797051911137));
#47439=CARTESIAN_POINT('Ctrl Pts',(70.4826066212365,113.041218359295,44.798774677055));
#47440=CARTESIAN_POINT('Ctrl Pts',(77.9593635041953,112.510828335414,44.7991813808552));
#47441=CARTESIAN_POINT('Ctrl Pts',(81.9103282168794,112.086516316309,48.5554210923868));
#47442=CARTESIAN_POINT('Ctrl Pts',(83.7054495670612,111.662204297205,53.7029446007828));
#47443=CARTESIAN_POINT('Ctrl Pts',(80.6257852548025,111.131814273324,60.5159880745971));
#47444=CARTESIAN_POINT('Ctrl Pts',(71.720413347007,110.495346244667,61.8115641539429));
#47445=CARTESIAN_POINT('Ctrl Pts',(65.8349527787794,109.85887821601,55.0266783582341));
#47446=CARTESIAN_POINT('Ctrl Pts',(68.3470806648557,109.222410187353,46.4033069267711));
#47447=CARTESIAN_POINT('Ctrl Pts',(76.9791566232342,108.585942158696,43.8594062128452));
#47448=CARTESIAN_POINT('Ctrl Pts',(82.6238218883199,108.055552134816,48.7624305547607));
#47449=CARTESIAN_POINT('Ctrl Pts',(83.1437191728509,107.631240115711,54.1891391101288));
#47450=CARTESIAN_POINT('Ctrl Pts',(81.1236568876865,107.206928096606,59.2526168967316));
#47451=CARTESIAN_POINT('Ctrl Pts',(74.3310164083526,106.676538072725,62.3770254760937));
#47452=CARTESIAN_POINT('Ctrl Pts',(66.7579385956598,106.040070044068,57.5156821806215));
#47453=CARTESIAN_POINT('Ctrl Pts',(66.7634693934056,105.403602015411,48.5338510326177));
#47454=CARTESIAN_POINT('Ctrl Pts',(74.3147037050667,104.767133986755,43.6705001578233));
#47455=CARTESIAN_POINT('Ctrl Pts',(82.5000049447651,104.130665958098,47.4101538595609));
#47456=CARTESIAN_POINT('Ctrl Pts',(83.5466631767871,103.600275934217,54.813288344198));
#47457=CARTESIAN_POINT('Ctrl Pts',(80.3807406526305,103.175963915112,59.2513502525542));
#47458=CARTESIAN_POINT('Ctrl Pts',(75.5353357858924,102.751651896008,61.7496517973554));
#47459=CARTESIAN_POINT('Ctrl Pts',(68.3581483960137,102.221261872127,59.6544489854898));
#47460=CARTESIAN_POINT('Ctrl Pts',(65.8282122980566,101.58479384347,51.0182698804815));
#47461=CARTESIAN_POINT('Ctrl Pts',(71.7220243420383,100.948325814813,44.2406374803592));
#47462=CARTESIAN_POINT('Ctrl Pts',(80.6122208890652,100.311857786156,45.5203744518521));
#47463=CARTESIAN_POINT('Ctrl Pts',(84.3399071186501,99.6753897574987,53.7111327541886));
#47464=CARTESIAN_POINT('Ctrl Pts',(80.2756903258973,99.1449997336185,59.9868028788675));
#47465=CARTESIAN_POINT('Ctrl Pts',(74.975266539261,98.7206877145133,61.2615446619069));
#47466=CARTESIAN_POINT('Ctrl Pts',(69.6787927430372,98.2963756954092,59.9704891800327));
#47467=CARTESIAN_POINT('Ctrl Pts',(65.6339176906133,97.765985671528,53.6823352806308));
#47468=CARTESIAN_POINT('Ctrl Pts',(69.3868051882764,97.1295176428713,45.5030931627196));
#47469=CARTESIAN_POINT('Ctrl Pts',(78.2808998424165,96.4930496142142,44.2507347299335));
#47470=CARTESIAN_POINT('Ctrl Pts',(84.1538159569591,95.8565815855574,51.0464817582238));
#47471=CARTESIAN_POINT('Ctrl Pts',(81.5973014851276,95.2201135569003,59.6748303805756));
#47472=CARTESIAN_POINT('Ctrl Pts',(74.4136970897655,94.6897235330197,61.7479250583973));
#47473=CARTESIAN_POINT('Ctrl Pts',(69.57600733628,94.265411513915,59.234716595021));
#47474=CARTESIAN_POINT('Ctrl Pts',(66.4237643903003,93.8410994948103,54.786928005071));
#47475=CARTESIAN_POINT('Ctrl Pts',(67.4932115438736,93.3107094709297,47.387051219746));
#47476=CARTESIAN_POINT('Ctrl Pts',(75.6899881930776,92.6742414422725,43.6726173790922));
#47477=CARTESIAN_POINT('Ctrl Pts',(83.2262126967134,92.0377734136157,48.5591950763949));
#47478=CARTESIAN_POINT('Ctrl Pts',(83.2040888570857,91.4013053849587,57.5410006797626));
#47479=CARTESIAN_POINT('Ctrl Pts',(75.6160791065193,90.7648373563018,62.3790038028331));
#47480=CARTESIAN_POINT('Ctrl Pts',(68.8330907226962,90.234447332421,59.2336958310749));
#47481=CARTESIAN_POINT('Ctrl Pts',(66.8286282087238,89.8101353133163,54.1640223739926));
#47482=CARTESIAN_POINT('Ctrl Pts',(67.365231594555,89.3858232942118,48.7389402789752));
#47483=CARTESIAN_POINT('Ctrl Pts',(73.0249662720164,88.8554332703308,43.8533188207551));
#47484=CARTESIAN_POINT('Ctrl Pts',(81.64916877083,88.2189652416742,46.4237852089792));
#47485=CARTESIAN_POINT('Ctrl Pts',(84.1347338179463,87.582497213017,55.0548504826013));
#47486=CARTESIAN_POINT('Ctrl Pts',(78.2284108209353,86.9460291843602,61.8215830778757));
#47487=CARTESIAN_POINT('Ctrl Pts',(69.3270701386897,86.3095611557031,60.4985939425711));
#47488=CARTESIAN_POINT('Ctrl Pts',(66.2683974458044,85.7791711318225,53.6761006292671));
#47489=CARTESIAN_POINT('Ctrl Pts',(68.0793592558839,85.3548591127177,48.534128609332));
#47490=CARTESIAN_POINT('Ctrl Pts',(72.041870516237,84.9305470936133,44.7900715260408));
#47491=CARTESIAN_POINT('Ctrl Pts',(79.5185932117496,84.4001570697323,44.8126853865582));
#47492=CARTESIAN_POINT('Ctrl Pts',(84.3443173630294,83.7636890410754,52.4085100691904));
#47493=CARTESIAN_POINT('Ctrl Pts',(80.5612831190361,83.1272210124184,60.5547959265457));
#47494=CARTESIAN_POINT('Ctrl Pts',(71.6648900329446,82.4907529837615,61.7907212554865));
#47495=CARTESIAN_POINT('Ctrl Pts',(65.8119217712407,81.8542849551046,54.9550114371124));
#47496=CARTESIAN_POINT('Ctrl Pts',(67.9763303389007,81.3238949312238,47.798390083113));
#47497=CARTESIAN_POINT('Ctrl Pts',(72.7153357424512,80.8995829121191,45.1037126039912));
#47498=CARTESIAN_POINT('Ctrl Pts',(78.1621036964017,80.4752708930144,44.8752880274158));
#47499=CARTESIAN_POINT('Ctrl Pts',(83.7921813002151,79.9448808691338,49.7950562970919));
#47500=CARTESIAN_POINT('Ctrl Pts',(82.4547971050774,79.3084128404767,58.6942455696115));
#47501=CARTESIAN_POINT('Ctrl Pts',(74.256870076961,78.6719448118199,62.3640294600686));
#47502=CARTESIAN_POINT('Ctrl Pts',(66.7296859060944,78.0354767831629,57.4635376665013));
#47503=CARTESIAN_POINT('Ctrl Pts',(66.7930750347046,77.3990087545059,48.4646406223128));
#47504=CARTESIAN_POINT('Ctrl Pts',(73.1199933779918,76.8686187306251,44.4806730107902));
#47505=CARTESIAN_POINT('Ctrl Pts',(78.4649050147291,76.4443067115205,45.5536960892167));
#47506=CARTESIAN_POINT('Ctrl Pts',(82.72698496152,76.0199946924159,48.952833253046));
#47507=CARTESIAN_POINT('Ctrl Pts',(83.7516500885383,75.489604668535,56.3590438245701));
#47508=CARTESIAN_POINT('Ctrl Pts',(76.9064827766719,74.8531366398783,62.2009485367414));
#47509=CARTESIAN_POINT('Ctrl Pts',(68.3106899580314,74.2166686112211,59.5960172171136));
#47510=CARTESIAN_POINT('Ctrl Pts',(65.8410741982038,73.5802005825644,50.9603748345353));
#47511=CARTESIAN_POINT('Ctrl Pts',(71.7897597135541,72.9437325539072,44.2077970428327));
#47512=CARTESIAN_POINT('Ctrl Pts',(79.1789648512062,72.4133425300267,45.3486480786734));
#47513=CARTESIAN_POINT('Ctrl Pts',(82.510748146959,71.9890305109218,49.6635848107129));
#47514=CARTESIAN_POINT('Ctrl Pts',(83.4996986871477,71.5647184918175,55.0246887791533));
#47515=CARTESIAN_POINT('Ctrl Pts',(79.4168600817985,71.0343284679364,61.2882598512299));
#47516=CARTESIAN_POINT('Ctrl Pts',(70.4180773315886,70.3978604392796,61.2103162302436));
#47517=CARTESIAN_POINT('Ctrl Pts',(65.6364020281329,69.7613924106226,53.6070996311131));
#47518=CARTESIAN_POINT('Ctrl Pts',(69.4344792799938,69.1249243819657,45.4678164593667));
#47519=CARTESIAN_POINT('Ctrl Pts',(78.3535742588854,68.4884563533086,44.2703562508269));
#47520=CARTESIAN_POINT('Ctrl Pts',(83.1843171408831,67.9580663294281,49.9770029772597));
#47521=CARTESIAN_POINT('Ctrl Pts',(82.8703809064456,67.5337543103232,55.4195118630653));
#47522=CARTESIAN_POINT('Ctrl Pts',(80.1016111182479,67.1094422912187,60.1156137349725));
#47523=CARTESIAN_POINT('Ctrl Pts',(72.9118809879765,66.5790522673378,62.1673628195703));
#47524=CARTESIAN_POINT('Ctrl Pts',(66.1689332730775,65.942584238681,56.2077636461637));
#47525=CARTESIAN_POINT('Ctrl Pts',(67.5444213185558,65.306116210024,47.3318775496817));
#47526=CARTESIAN_POINT('Ctrl Pts',(75.7491139228169,64.6696481813672,43.6772447869338));
#47527=CARTESIAN_POINT('Ctrl Pts',(83.2682153150902,64.03318015271,48.6216639081496));
#47528=CARTESIAN_POINT('Ctrl Pts',(83.1734067383262,63.5027901288294,56.0978196707095));
#47529=CARTESIAN_POINT('Ctrl Pts',(79.367581365659,63.0784781097246,60.0010429751245));
#47530=CARTESIAN_POINT('Ctrl Pts',(74.1978028836267,62.6541660906201,61.7310283444492));
#47531=CARTESIAN_POINT('Ctrl Pts',(67.424186484631,62.1237760667393,58.5655876908371));
#47532=CARTESIAN_POINT('Ctrl Pts',(66.2411533478682,61.4873080380824,49.6445676375667));
#47533=CARTESIAN_POINT('Ctrl Pts',(73.0998084272228,60.8508400094254,43.8452425161916));
#47534=CARTESIAN_POINT('Ctrl Pts',(81.6907742226954,60.2143719807683,46.4660492740419));
#47535=CARTESIAN_POINT('Ctrl Pts',(84.1254831361944,59.5779039521116,55.129556571901));
#47536=CARTESIAN_POINT('Ctrl Pts',(79.1515797976825,59.0475139282307,60.7118660609407));
#47537=CARTESIAN_POINT('Ctrl Pts',(73.7187395656729,58.6232019091261,61.16320401062));
#47538=CARTESIAN_POINT('Ctrl Pts',(68.6811708049024,58.1988898900216,59.0793710250198));
#47539=CARTESIAN_POINT('Ctrl Pts',(65.6427754951433,57.6684998661406,52.2478230603257));
#47540=CARTESIAN_POINT('Ctrl Pts',(70.5993493427058,57.0320318374837,44.7367284738365));
#47541=CARTESIAN_POINT('Ctrl Pts',(79.5803947011489,56.3955638088268,44.8556638788466));
#47542=CARTESIAN_POINT('Ctrl Pts',(84.3480156486463,55.7590957801698,52.4677011791989));
#47543=CARTESIAN_POINT('Ctrl Pts',(80.5053120194535,55.122627751513,60.6051329000625));
#47544=CARTESIAN_POINT('Ctrl Pts',(73.0895524925331,54.5922377276321,61.5582353558216));
#47545=CARTESIAN_POINT('Ctrl Pts',(68.6918174455575,54.1679257085274,58.3365300018253));
#47546=CARTESIAN_POINT('Ctrl Pts',(66.2548933682926,53.7436136894228,53.4599676908307));
#47547=CARTESIAN_POINT('Ctrl Pts',(68.4405486939056,53.2132236655421,46.3098065423043));
#47548=CARTESIAN_POINT('Ctrl Pts',(77.1079824933874,52.5767556368851,43.8891129381638));
#47549=CARTESIAN_POINT('Ctrl Pts',(83.8106590717248,51.9402876082283,49.8680299008908));
#47550=CARTESIAN_POINT('Ctrl Pts',(82.4187760452078,51.3038195795712,58.7413597719972));
#47551=CARTESIAN_POINT('Ctrl Pts',(74.181604690216,50.6673515509143,62.3653319382867));
#47552=CARTESIAN_POINT('Ctrl Pts',(67.9577498141223,50.1369615270334,58.2222021872887));
#47553=CARTESIAN_POINT('Ctrl Pts',(66.7500330581167,49.7126495079289,52.9061059533381));
#47554=CARTESIAN_POINT('Ctrl Pts',(68.107859170072,49.2883374888242,47.6263552792002));
#47555=CARTESIAN_POINT('Ctrl Pts',(74.4465826239457,48.7579474649434,43.6611971956435));
#47556=CARTESIAN_POINT('Ctrl Pts',(82.5777886154376,48.1214794362866,47.5170570630991));
#47557=CARTESIAN_POINT('Ctrl Pts',(83.717749937762,47.4850114076295,56.4262550934819));
#47558=CARTESIAN_POINT('Ctrl Pts',(76.8483928784914,46.8485433789726,62.2128996266483));
#47559=CARTESIAN_POINT('Ctrl Pts',(68.2530107161164,46.2120753503157,59.5476469789136));
#47560=CARTESIAN_POINT('Ctrl Pts',(66.2707818357398,45.6816853264349,52.3384402043735));
#47561=CARTESIAN_POINT('Ctrl Pts',(68.8448708790405,45.2573733073303,47.5328679670094));
#47562=CARTESIAN_POINT('Ctrl Pts',(73.3321053046874,44.8330612882256,44.4370342924303));
#47563=CARTESIAN_POINT('Ctrl Pts',(80.7178893398119,44.3026712643448,45.5998274119405));
#47564=CARTESIAN_POINT('Ctrl Pts',(84.3285341855929,43.6662032356878,53.8428493087427));
#47565=CARTESIAN_POINT('Ctrl Pts',(79.3471932593963,43.029735207031,61.3167749130004));
#47566=CARTESIAN_POINT('Ctrl Pts',(70.3663829481276,42.393267178374,61.1812481112956));
#47567=CARTESIAN_POINT('Ctrl Pts',(65.6245720603672,41.7567991497171,53.5327583454499));
#47568=CARTESIAN_POINT('Ctrl Pts',(68.8552716638434,41.2264091258363,46.7900234608216));
#47569=CARTESIAN_POINT('Ctrl Pts',(73.949849452103,40.8020971067316,44.8497306760242));
#47570=CARTESIAN_POINT('Ctrl Pts',(79.3677239232426,40.377785087627,45.4547886454258));
#47571=CARTESIAN_POINT('Ctrl Pts',(84.1814958476775,39.8473950637462,51.1757582758122));
#47572=CARTESIAN_POINT('Ctrl Pts',(81.5023447448448,39.2109270350893,59.7668184875512));
#47573=CARTESIAN_POINT('Ctrl Pts',(72.8405846002177,38.5744590064323,62.1432091452338));
#47574=CARTESIAN_POINT('Ctrl Pts',(66.1489649218033,37.9379909777754,56.1519198482274));
#47575=CARTESIAN_POINT('Ctrl Pts',(67.5842373708341,37.3015229491184,47.2679928341982));
#47576=CARTESIAN_POINT('Ctrl Pts',(74.4448058052946,36.7711329252377,44.2957050943661));
#47577=CARTESIAN_POINT('Ctrl Pts',(79.5635026555143,36.346820906133,46.1714453447497));
#47578=CARTESIAN_POINT('Ctrl Pts',(83.2572304286379,35.9225088870284,50.1809133979266));
#47579=CARTESIAN_POINT('Ctrl Pts',(83.1402168969827,35.3921188631477,57.6567545870878));
#47580=CARTESIAN_POINT('Ctrl Pts',(75.4840678569184,34.7556508344906,62.38618881013));
#47581=CARTESIAN_POINT('Ctrl Pts',(67.3861961333135,34.1191828058337,58.5006007067545));
#47582=CARTESIAN_POINT('Ctrl Pts',(66.2626956250231,33.4827147771767,49.5893119128753));
#47583=CARTESIAN_POINT('Ctrl Pts',(73.1717604263215,32.8462467485199,43.8231182145451));
#47584=CARTESIAN_POINT('Ctrl Pts',(80.300483382939,32.315856724639,46.0777141118401));
#47585=CARTESIAN_POINT('Ctrl Pts',(82.9351111460744,31.8915447055345,50.8503648929889));
#47586=CARTESIAN_POINT('Ctrl Pts',(83.0947463504551,31.4672326864297,56.2995827762267));
#47587=CARTESIAN_POINT('Ctrl Pts',(78.1042846037941,30.936842662549,61.8670943558816));
#47588=CARTESIAN_POINT('Ctrl Pts',(69.2226905800411,30.3003746338921,60.4174551605608));
#47589=CARTESIAN_POINT('Ctrl Pts',(65.6567066513159,29.6639066052351,52.1738467249999));
#47590=CARTESIAN_POINT('Ctrl Pts',(70.6518464186429,29.0274385765782,44.7091364205264));
#47591=CARTESIAN_POINT('Ctrl Pts',(79.6492257952861,28.3909705479212,44.8861410045034));
#47592=CARTESIAN_POINT('Ctrl Pts',(83.552991842885,27.8605805240404,51.2628568188668));
#47593=CARTESIAN_POINT('Ctrl Pts',(82.4125691883584,27.4362685049358,56.5937943203991));
#47594=CARTESIAN_POINT('Ctrl Pts',(78.959889717477,27.0119564858311,60.812616932623));
#47595=CARTESIAN_POINT('Ctrl Pts',(71.5413320884577,26.4815664619504,61.743689023496));
#47596=CARTESIAN_POINT('Ctrl Pts',(65.7863203711639,25.8450984332935,54.8253074886375));
#47597=CARTESIAN_POINT('Ctrl Pts',(68.4995751288869,25.2086304046365,46.2630892864365));
#47598=CARTESIAN_POINT('Ctrl Pts',(77.1657103179859,24.5721623759795,43.9027054865252));
#47599=CARTESIAN_POINT('Ctrl Pts',(83.8426420808462,23.9356943473226,49.9361731535205));
#47600=CARTESIAN_POINT('Ctrl Pts',(82.6085843589776,23.4053043234418,57.3103885914542));
#47601=CARTESIAN_POINT('Ctrl Pts',(78.2519260276138,22.9809923043372,60.5874201313303));
#47602=CARTESIAN_POINT('Ctrl Pts',(72.8787595021107,22.5566802852326,61.5086132067331));
#47603=CARTESIAN_POINT('Ctrl Pts',(66.6672452762723,22.0262902613518,57.3469916847974));
#47604=CARTESIAN_POINT('Ctrl Pts',(66.85878821435,21.3898222326947,48.3499544346595));
#47605=CARTESIAN_POINT('Ctrl Pts',(74.5217964330623,20.7533542040379,43.664580771223));
#47606=CARTESIAN_POINT('Ctrl Pts',(82.6124311846432,20.1168861753809,47.5652683417291));
#47607=CARTESIAN_POINT('Ctrl Pts',(83.6972706997256,19.480418146724,56.4984863200123));
#47608=CARTESIAN_POINT('Ctrl Pts',(77.9299254702141,18.9500281228433,61.2573127511593));
#47609=CARTESIAN_POINT('Ctrl Pts',(72.4920520828531,18.5257161037386,60.8739104023719));
#47610=CARTESIAN_POINT('Ctrl Pts',(67.8308159848136,18.1014040846339,58.0475875686556));
#47611=CARTESIAN_POINT('Ctrl Pts',(65.8710431841307,17.5710140607531,50.8291601454251));
#47612=CARTESIAN_POINT('Ctrl Pts',(71.9134175217386,16.9345460320962,44.1681258720739));
#47613=CARTESIAN_POINT('Ctrl Pts',(80.7745918640496,16.2980780034393,45.6446820440961));
#47614=CARTESIAN_POINT('Ctrl Pts',(84.3188969900482,15.6616099747824,53.9154373611954));
#47615=CARTESIAN_POINT('Ctrl Pts',(80.1313293268964,15.1312199509016,60.0939695185882));
#47616=CARTESIAN_POINT('Ctrl Pts',(74.786341856204,14.7069079317969,61.2678572289885));
#47617=CARTESIAN_POINT('Ctrl Pts',(72.1730647398712,14.4947519222446,60.5478236301968));
#47618=CARTESIAN_POINT('Ctrl Pts',(71.0291102539094,14.3886739174684,59.8881742938589));
#47619=CARTESIAN_POINT('Ctrl Pts',(82.9129498948689,15.7216677763616,53.0228109606368));
#47620=CARTESIAN_POINT('Ctrl Pts',(82.9129498948686,15.5454469188779,55.216507035084));
#47621=CARTESIAN_POINT('Ctrl Pts',(81.9532970624634,15.3692260613942,57.3933791504626));
#47622=CARTESIAN_POINT('Ctrl Pts',(80.33387643929,15.1930052039106,58.8731694438102));
#47623=CARTESIAN_POINT('Ctrl Pts',(79.7426550745104,15.1286701359404,59.413414284651));
#47624=CARTESIAN_POINT('Ctrl Pts',(79.0690015640715,15.0643350679702,59.8632823964012));
#47625=CARTESIAN_POINT('Ctrl Pts',(78.3434537325938,15.,60.2023805156308));
#47626=CARTESIAN_POINT('Origin',(74.9879498948689,255.,53.0228109606356));
#47627=CARTESIAN_POINT('',(0.,0.,0.));
#47628=CARTESIAN_POINT('Origin',(54.380525740571,212.,66.9996518063507));
#47629=CARTESIAN_POINT('',(90.6194742594292,212.,37.9996518063507));
#47630=CARTESIAN_POINT('',(95.6194742594292,212.,42.9996518063507));
#47631=CARTESIAN_POINT('Origin',(90.6194742594292,212.,42.9996518063507));
#47632=CARTESIAN_POINT('',(59.380525740571,212.,37.9996518063507));
#47633=CARTESIAN_POINT('',(54.380525740571,212.,37.9996518063507));
#47634=CARTESIAN_POINT('',(54.380525740571,212.,42.9996518063507));
#47635=CARTESIAN_POINT('Origin',(59.380525740571,212.,42.9996518063507));
#47636=CARTESIAN_POINT('',(54.380525740571,212.,66.9996518063507));
#47637=CARTESIAN_POINT('',(54.380525740571,212.,66.9996518063507));
#47638=CARTESIAN_POINT('',(95.6194742594292,212.,66.9996518063507));
#47639=CARTESIAN_POINT('',(45.7696402469604,212.,66.9996518063507));
#47640=CARTESIAN_POINT('',(95.6194742594292,212.,66.9996518063507));
#47641=CARTESIAN_POINT('',(66.8941998948689,212.,53.0228109606356));
#47642=CARTESIAN_POINT('Origin',(74.9879498948689,212.,53.0228109606356));
#47643=CARTESIAN_POINT('Origin',(118.97074981153,135.774646529765,79.9996518063507));
#47644=CARTESIAN_POINT('',(121.97074981153,135.774646529765,79.9996518063507));
#47645=CARTESIAN_POINT('Origin',(118.97074981153,135.774646529765,79.9996518063507));
#47646=CARTESIAN_POINT('',(121.97074981153,135.774646529765,59.9996518063507));
#47647=CARTESIAN_POINT('',(121.97074981153,135.774646529765,79.9996518063507));
#47648=CARTESIAN_POINT('Origin',(118.97074981153,135.774646529765,59.9996518063507));
#47649=CARTESIAN_POINT('Origin',(150.97074981153,273.774646529765,79.9996518063507));
#47650=CARTESIAN_POINT('',(153.97074981153,273.774646529765,79.9996518063507));
#47651=CARTESIAN_POINT('Origin',(150.97074981153,273.774646529765,79.9996518063507));
#47652=CARTESIAN_POINT('',(153.97074981153,273.774646529765,59.9996518063507));
#47653=CARTESIAN_POINT('',(153.97074981153,273.774646529765,79.9996518063507));
#47654=CARTESIAN_POINT('Origin',(150.97074981153,273.774646529765,59.9996518063507));
#47655=CARTESIAN_POINT('Origin',(-1.02925018847036,273.774646529765,79.9996518063507));
#47656=CARTESIAN_POINT('',(1.97074981152964,273.774646529765,79.9996518063507));
#47657=CARTESIAN_POINT('Origin',(-1.02925018847036,273.774646529765,79.9996518063507));
#47658=CARTESIAN_POINT('',(1.97074981152964,273.774646529765,59.9996518063507));
#47659=CARTESIAN_POINT('',(1.97074981152964,273.774646529765,79.9996518063507));
#47660=CARTESIAN_POINT('Origin',(-1.02925018847036,273.774646529765,59.9996518063507));
#47661=CARTESIAN_POINT('Origin',(-1.02925018847036,171.774646529765,79.9996518063507));
#47662=CARTESIAN_POINT('',(1.97074981152964,171.774646529765,79.9996518063507));
#47663=CARTESIAN_POINT('Origin',(-1.02925018847036,171.774646529765,79.9996518063507));
#47664=CARTESIAN_POINT('',(1.97074981152964,171.774646529765,59.9996518063507));
#47665=CARTESIAN_POINT('',(1.97074981152964,171.774646529765,79.9996518063507));
#47666=CARTESIAN_POINT('Origin',(-1.02925018847036,171.774646529765,59.9996518063507));
#47667=CARTESIAN_POINT('Origin',(30.9707498115296,135.774646529765,79.9996518063507));
#47668=CARTESIAN_POINT('',(33.9707498115296,135.774646529765,79.9996518063507));
#47669=CARTESIAN_POINT('Origin',(30.9707498115296,135.774646529765,79.9996518063507));
#47670=CARTESIAN_POINT('',(33.9707498115296,135.774646529765,59.9996518063507));
#47671=CARTESIAN_POINT('',(33.9707498115296,135.774646529765,79.9996518063507));
#47672=CARTESIAN_POINT('Origin',(30.9707498115296,135.774646529765,59.9996518063507));
#47673=CARTESIAN_POINT('Origin',(30.9707498115296,237.774646529765,79.9996518063507));
#47674=CARTESIAN_POINT('',(33.9707498115296,237.774646529765,79.9996518063507));
#47675=CARTESIAN_POINT('Origin',(30.9707498115296,237.774646529765,79.9996518063507));
#47676=CARTESIAN_POINT('',(33.9707498115296,237.774646529765,59.9996518063507));
#47677=CARTESIAN_POINT('',(33.9707498115296,237.774646529765,79.9996518063507));
#47678=CARTESIAN_POINT('Origin',(30.9707498115296,237.774646529765,59.9996518063507));
#47679=CARTESIAN_POINT('Origin',(118.97074981153,273.774646529765,79.9996518063507));
#47680=CARTESIAN_POINT('',(121.97074981153,273.774646529765,79.9996518063507));
#47681=CARTESIAN_POINT('Origin',(118.97074981153,273.774646529765,79.9996518063507));
#47682=CARTESIAN_POINT('',(121.97074981153,273.774646529765,59.9996518063507));
#47683=CARTESIAN_POINT('',(121.97074981153,273.774646529765,79.9996518063507));
#47684=CARTESIAN_POINT('Origin',(118.97074981153,273.774646529765,59.9996518063507));
#47685=CARTESIAN_POINT('Origin',(118.97074981153,171.774646529765,79.9996518063507));
#47686=CARTESIAN_POINT('',(121.97074981153,171.774646529765,79.9996518063507));
#47687=CARTESIAN_POINT('Origin',(118.97074981153,171.774646529765,79.9996518063507));
#47688=CARTESIAN_POINT('',(121.97074981153,171.774646529765,59.9996518063507));
#47689=CARTESIAN_POINT('',(121.97074981153,171.774646529765,79.9996518063507));
#47690=CARTESIAN_POINT('Origin',(118.97074981153,171.774646529765,59.9996518063507));
#47691=CARTESIAN_POINT('Origin',(150.97074981153,171.774646529765,79.9996518063507));
#47692=CARTESIAN_POINT('',(153.97074981153,171.774646529765,79.9996518063507));
#47693=CARTESIAN_POINT('Origin',(150.97074981153,171.774646529765,79.9996518063507));
#47694=CARTESIAN_POINT('',(153.97074981153,171.774646529765,59.9996518063507));
#47695=CARTESIAN_POINT('',(153.97074981153,171.774646529765,79.9996518063507));
#47696=CARTESIAN_POINT('Origin',(150.97074981153,171.774646529765,59.9996518063507));
#47697=CARTESIAN_POINT('Origin',(118.97074981153,237.774646529765,79.9996518063507));
#47698=CARTESIAN_POINT('',(121.97074981153,237.774646529765,79.9996518063507));
#47699=CARTESIAN_POINT('Origin',(118.97074981153,237.774646529765,79.9996518063507));
#47700=CARTESIAN_POINT('',(121.97074981153,237.774646529765,59.9996518063507));
#47701=CARTESIAN_POINT('',(121.97074981153,237.774646529765,79.9996518063507));
#47702=CARTESIAN_POINT('Origin',(118.97074981153,237.774646529765,59.9996518063507));
#47703=CARTESIAN_POINT('Origin',(30.9707498115296,273.774646529765,79.9996518063507));
#47704=CARTESIAN_POINT('',(33.9707498115296,273.774646529765,79.9996518063507));
#47705=CARTESIAN_POINT('Origin',(30.9707498115296,273.774646529765,79.9996518063507));
#47706=CARTESIAN_POINT('',(33.9707498115296,273.774646529765,59.9996518063507));
#47707=CARTESIAN_POINT('',(33.9707498115296,273.774646529765,79.9996518063507));
#47708=CARTESIAN_POINT('Origin',(30.9707498115296,273.774646529765,59.9996518063507));
#47709=CARTESIAN_POINT('Origin',(-1.02925018847036,135.774646529765,79.9996518063507));
#47710=CARTESIAN_POINT('',(1.97074981152964,135.774646529765,79.9996518063507));
#47711=CARTESIAN_POINT('Origin',(-1.02925018847036,135.774646529765,79.9996518063507));
#47712=CARTESIAN_POINT('',(1.97074981152964,135.774646529765,59.9996518063507));
#47713=CARTESIAN_POINT('',(1.97074981152964,135.774646529765,79.9996518063507));
#47714=CARTESIAN_POINT('Origin',(-1.02925018847036,135.774646529765,59.9996518063507));
#47715=CARTESIAN_POINT('Origin',(30.9707498115296,171.774646529765,79.9996518063507));
#47716=CARTESIAN_POINT('',(33.9707498115296,171.774646529765,79.9996518063507));
#47717=CARTESIAN_POINT('Origin',(30.9707498115296,171.774646529765,79.9996518063507));
#47718=CARTESIAN_POINT('',(33.9707498115296,171.774646529765,59.9996518063507));
#47719=CARTESIAN_POINT('',(33.9707498115296,171.774646529765,79.9996518063507));
#47720=CARTESIAN_POINT('Origin',(30.9707498115296,171.774646529765,59.9996518063507));
#47721=CARTESIAN_POINT('Origin',(-1.02925018847036,237.774646529765,79.9996518063507));
#47722=CARTESIAN_POINT('',(1.97074981152964,237.774646529765,79.9996518063507));
#47723=CARTESIAN_POINT('Origin',(-1.02925018847036,237.774646529765,79.9996518063507));
#47724=CARTESIAN_POINT('',(1.97074981152964,237.774646529765,59.9996518063507));
#47725=CARTESIAN_POINT('',(1.97074981152964,237.774646529765,79.9996518063507));
#47726=CARTESIAN_POINT('Origin',(-1.02925018847036,237.774646529765,59.9996518063507));
#47727=CARTESIAN_POINT('Origin',(150.97074981153,237.774646529765,79.9996518063507));
#47728=CARTESIAN_POINT('',(153.97074981153,237.774646529765,79.9996518063507));
#47729=CARTESIAN_POINT('Origin',(150.97074981153,237.774646529765,79.9996518063507));
#47730=CARTESIAN_POINT('',(153.97074981153,237.774646529765,59.9996518063507));
#47731=CARTESIAN_POINT('',(153.97074981153,237.774646529765,79.9996518063507));
#47732=CARTESIAN_POINT('Origin',(150.97074981153,237.774646529765,59.9996518063507));
#47733=CARTESIAN_POINT('Origin',(150.97074981153,135.774646529765,79.9996518063507));
#47734=CARTESIAN_POINT('',(153.97074981153,135.774646529765,79.9996518063507));
#47735=CARTESIAN_POINT('Origin',(150.97074981153,135.774646529765,79.9996518063507));
#47736=CARTESIAN_POINT('',(153.97074981153,135.774646529765,59.9996518063507));
#47737=CARTESIAN_POINT('',(153.97074981153,135.774646529765,79.9996518063507));
#47738=CARTESIAN_POINT('Origin',(150.97074981153,135.774646529765,59.9996518063507));
#47739=CARTESIAN_POINT('Origin',(74.9879498948689,189.688844000289,53.0228109606356));
#47740=CARTESIAN_POINT('',(66.8941998948689,198.,53.0228109606356));
#47741=CARTESIAN_POINT('Origin',(74.9879498948689,198.,53.0228109606356));
#47742=CARTESIAN_POINT('',(66.8941998948689,189.688844000289,53.0228109606356));
#47743=CARTESIAN_POINT('Origin',(90.6194742594292,208.5,42.9996518063507));
#47744=CARTESIAN_POINT('',(95.6194742594292,198.,42.9996518063507));
#47745=CARTESIAN_POINT('',(90.6194742594292,198.,37.9996518063507));
#47746=CARTESIAN_POINT('Origin',(90.6194742594292,198.,42.9996518063507));
#47747=CARTESIAN_POINT('',(90.6194742594292,208.5,37.9996518063507));
#47748=CARTESIAN_POINT('',(95.6194742594292,208.5,42.9996518063507));
#47749=CARTESIAN_POINT('Origin',(75.0000000000001,205.,37.9996518063507));
#47750=CARTESIAN_POINT('',(59.380525740571,198.,37.9996518063507));
#47751=CARTESIAN_POINT('',(95.6194742594292,198.,37.9996518063507));
#47752=CARTESIAN_POINT('',(59.380525740571,201.5,37.9996518063507));
#47753=CARTESIAN_POINT('Origin',(59.380525740571,201.5,42.9996518063507));
#47754=CARTESIAN_POINT('',(54.380525740571,198.,42.9996518063507));
#47755=CARTESIAN_POINT('Origin',(59.380525740571,198.,42.9996518063507));
#47756=CARTESIAN_POINT('',(54.380525740571,201.5,42.9996518063507));
#47757=CARTESIAN_POINT('Origin',(54.380525740571,198.,66.9996518063507));
#47758=CARTESIAN_POINT('',(54.380525740571,198.,66.9996518063507));
#47759=CARTESIAN_POINT('',(54.380525740571,198.,66.9996518063507));
#47760=CARTESIAN_POINT('',(54.380525740571,157.,66.9996518063507));
#47761=CARTESIAN_POINT('Origin',(95.6194742594292,198.,66.9996518063507));
#47762=CARTESIAN_POINT('',(95.6194742594292,198.,66.9996518063507));
#47763=CARTESIAN_POINT('',(95.6194742594292,198.,66.9996518063507));
#47764=CARTESIAN_POINT('',(66.3891145063896,198.,66.9996518063507));
#47765=CARTESIAN_POINT('Origin',(95.6194742594292,212.,66.9996518063507));
#47766=CARTESIAN_POINT('',(95.6194742594292,164.,66.9996518063507));
#47767=CARTESIAN_POINT('Origin',(112.84124524665,116.,66.9996518063507));
#47768=CARTESIAN_POINT('',(112.84124524665,116.,66.9996518063507));
#47769=CARTESIAN_POINT('',(112.84124524665,116.,59.9996518063507));
#47770=CARTESIAN_POINT('',(112.84124524665,116.,63.4996518063507));
#47771=CARTESIAN_POINT('',(112.84124524665,294.,66.9996518063507));
#47772=CARTESIAN_POINT('',(112.84124524665,116.,66.9996518063507));
#47773=CARTESIAN_POINT('',(112.84124524665,294.,59.9996518063507));
#47774=CARTESIAN_POINT('',(112.84124524665,294.,63.4996518063507));
#47775=CARTESIAN_POINT('',(112.84124524665,160.5,59.9996518063507));
#47776=CARTESIAN_POINT('Origin',(37.1587547533499,116.,66.9996518063507));
#47777=CARTESIAN_POINT('',(37.1587547533499,116.,66.9996518063507));
#47778=CARTESIAN_POINT('',(15.3915723951113,116.,66.9996518063507));
#47779=CARTESIAN_POINT('',(37.1587547533499,294.,66.9996518063507));
#47780=CARTESIAN_POINT('',(37.1587547533499,116.,66.9996518063507));
#47781=CARTESIAN_POINT('',(96.7671823582386,294.,66.9996518063507));
#47782=CARTESIAN_POINT('Origin',(37.1587547533499,116.,59.9996518063507));
#47783=CARTESIAN_POINT('',(37.1587547533499,116.,59.9996518063507));
#47784=CARTESIAN_POINT('',(37.1587547533499,116.,59.9996518063507));
#47785=CARTESIAN_POINT('',(37.1587547533499,294.,59.9996518063507));
#47786=CARTESIAN_POINT('',(37.1587547533499,160.5,59.9996518063507));
#47787=CARTESIAN_POINT('',(37.1587547533499,294.,59.9996518063507));
#47788=CARTESIAN_POINT('Origin',(75.,205.,59.9996518063507));
#47789=CARTESIAN_POINT('',(156.375609963127,294.,59.9996518063507));
#47790=CARTESIAN_POINT('',(156.375609963127,294.,59.9996518063507));
#47791=CARTESIAN_POINT('',(156.375609963127,116.,59.9996518063507));
#47792=CARTESIAN_POINT('',(156.375609963127,116.,59.9996518063507));
#47793=CARTESIAN_POINT('',(-6.37560996312729,116.,59.9996518063507));
#47794=CARTESIAN_POINT('Origin',(75.,205.,59.9996518063507));
#47795=CARTESIAN_POINT('',(-6.37560996312729,116.,59.9996518063507));
#47796=CARTESIAN_POINT('',(-6.37560996312729,116.,59.9996518063507));
#47797=CARTESIAN_POINT('',(-6.37560996312729,294.,59.9996518063507));
#47798=CARTESIAN_POINT('',(-6.37560996312729,294.,59.9996518063507));
#47799=CARTESIAN_POINT('',(156.375609963127,294.,59.9996518063507));
#47800=CARTESIAN_POINT('Origin',(-6.37560996312729,116.,59.9996518063507));
#47801=CARTESIAN_POINT('',(156.375609963127,116.,79.9996518063507));
#47802=CARTESIAN_POINT('',(156.375609963127,116.,59.9996518063507));
#47803=CARTESIAN_POINT('',(-6.37560996312729,116.,79.9996518063507));
#47804=CARTESIAN_POINT('',(-6.37560996312729,116.,79.9996518063507));
#47805=CARTESIAN_POINT('',(-6.37560996312729,116.,59.9996518063507));
#47806=CARTESIAN_POINT('Origin',(156.375609963127,294.,59.9996518063507));
#47807=CARTESIAN_POINT('',(-6.37560996312729,294.,79.9996518063507));
#47808=CARTESIAN_POINT('',(-6.37560996312729,294.,59.9996518063507));
#47809=CARTESIAN_POINT('',(156.375609963127,294.,79.9996518063507));
#47810=CARTESIAN_POINT('',(156.375609963127,294.,79.9996518063507));
#47811=CARTESIAN_POINT('',(156.375609963127,294.,59.9996518063507));
#47812=CARTESIAN_POINT('Origin',(156.375609963127,116.,59.9996518063507));
#47813=CARTESIAN_POINT('',(156.375609963127,116.,79.9996518063507));
#47814=CARTESIAN_POINT('Origin',(-6.37560996312729,294.,59.9996518063507));
#47815=CARTESIAN_POINT('',(-6.37560996312729,294.,79.9996518063507));
#47816=CARTESIAN_POINT('Origin',(75.,205.,79.9996518063507));
#47817=CARTESIAN_POINT('',(0.,0.,0.));
#47818=CARTESIAN_POINT('Origin',(142.5822836287,255.,47.007169160326));
#47819=CARTESIAN_POINT('',(142.094409841973,15.,47.5000804575095));
#47820=CARTESIAN_POINT('',(142.094409841973,495.,47.5000804575095));
#47821=CARTESIAN_POINT('',(142.094409841973,255.,47.5000804575095));
#47822=CARTESIAN_POINT('',(142.5822836287,15.,47.007169160326));
#47823=CARTESIAN_POINT('',(142.094409841973,15.,47.5000804575095));
#47824=CARTESIAN_POINT('',(142.5822836287,495.,47.007169160326));
#47825=CARTESIAN_POINT('',(142.5822836287,255.,47.007169160326));
#47826=CARTESIAN_POINT('',(142.094409841973,495.,47.5000804575095));
#47827=CARTESIAN_POINT('Origin',(142.262455466246,255.,46.690609613792));
#47828=CARTESIAN_POINT('',(142.695977084858,15.,46.8112703207193));
#47829=CARTESIAN_POINT('Origin',(142.262455466246,15.,46.690609613792));
#47830=CARTESIAN_POINT('',(142.695977084858,495.,46.8112703207193));
#47831=CARTESIAN_POINT('',(142.695977084858,255.,46.8112703207193));
#47832=CARTESIAN_POINT('Origin',(142.262455466246,495.,46.690609613792));
#47833=CARTESIAN_POINT('Origin',(145.073060872192,255.,47.4728765656934));
#47834=CARTESIAN_POINT('',(144.344825886597,15.,45.1153516005764));
#47835=CARTESIAN_POINT('Origin',(145.073060872192,15.,47.4728765656934));
#47836=CARTESIAN_POINT('',(144.344825886597,495.,45.1153516005764));
#47837=CARTESIAN_POINT('',(144.344825886597,255.,45.1153516005764));
#47838=CARTESIAN_POINT('Origin',(145.073060872192,495.,47.4728765656934));
#47839=CARTESIAN_POINT('Origin',(144.130850755256,255.,44.4226470147914));
#47840=CARTESIAN_POINT('',(144.855850755256,15.,44.4226470147914));
#47841=CARTESIAN_POINT('Origin',(144.130850755256,15.,44.4226470147914));
#47842=CARTESIAN_POINT('',(144.855850755256,495.,44.4226470147914));
#47843=CARTESIAN_POINT('',(144.855850755256,255.,44.4226470147914));
#47844=CARTESIAN_POINT('Origin',(144.130850755256,495.,44.4226470147914));
#47845=CARTESIAN_POINT('Origin',(144.855850755256,255.,43.5036225521864));
#47846=CARTESIAN_POINT('',(144.855850755256,15.,43.5036225521864));
#47847=CARTESIAN_POINT('',(144.855850755256,15.,44.4226470147914));
#47848=CARTESIAN_POINT('',(144.855850755256,495.,43.5036225521864));
#47849=CARTESIAN_POINT('',(144.855850755256,255.,43.5036225521864));
#47850=CARTESIAN_POINT('',(144.855850755256,495.,44.4226470147914));
#47851=CARTESIAN_POINT('Origin',(144.255850755256,255.,43.5036225521863));
#47852=CARTESIAN_POINT('',(144.403306787367,15.,42.9220241352404));
#47853=CARTESIAN_POINT('Origin',(144.255850755256,15.,43.5036225521863));
#47854=CARTESIAN_POINT('',(144.403306787367,495.,42.9220241352404));
#47855=CARTESIAN_POINT('',(144.403306787367,255.,42.9220241352404));
#47856=CARTESIAN_POINT('Origin',(144.255850755256,495.,43.5036225521863));
#47857=CARTESIAN_POINT('Origin',(144.984289187873,255.,40.6305041508116));
#47858=CARTESIAN_POINT('',(142.734368503612,15.,41.3560806824536));
#47859=CARTESIAN_POINT('Origin',(144.984289187873,15.,40.6305041508116));
#47860=CARTESIAN_POINT('',(142.734368503612,495.,41.3560806824536));
#47861=CARTESIAN_POINT('',(142.734368503612,255.,41.3560806824536));
#47862=CARTESIAN_POINT('Origin',(144.984289187873,495.,40.6305041508116));
#47863=CARTESIAN_POINT('Origin',(141.401941087198,255.,41.7857749691141));
#47864=CARTESIAN_POINT('',(142.398712869122,15.,40.8026951072716));
#47865=CARTESIAN_POINT('Origin',(141.401941087198,15.,41.7857749691141));
#47866=CARTESIAN_POINT('',(142.398712869122,495.,40.8026951072716));
#47867=CARTESIAN_POINT('',(142.398712869122,255.,40.8026951072716));
#47868=CARTESIAN_POINT('Origin',(141.401941087198,495.,41.7857749691141));
#47869=CARTESIAN_POINT('Origin',(141.760942367476,255.,40.1560420081102));
#47870=CARTESIAN_POINT('',(141.760942367476,15.,40.1560420081102));
#47871=CARTESIAN_POINT('',(141.760942367476,15.,40.1560420081102));
#47872=CARTESIAN_POINT('',(141.760942367476,495.,40.1560420081102));
#47873=CARTESIAN_POINT('',(141.760942367476,255.,40.1560420081102));
#47874=CARTESIAN_POINT('',(141.760942367476,495.,40.1560420081102));
#47875=CARTESIAN_POINT('Origin',(142.508521203919,255.,39.4187321117283));
#47876=CARTESIAN_POINT('',(141.458521203919,15.,39.4187321117283));
#47877=CARTESIAN_POINT('Origin',(142.508521203919,15.,39.4187321117283));
#47878=CARTESIAN_POINT('',(141.458521203919,495.,39.4187321117283));
#47879=CARTESIAN_POINT('',(141.458521203919,255.,39.4187321117283));
#47880=CARTESIAN_POINT('Origin',(142.508521203919,495.,39.4187321117283));
#47881=CARTESIAN_POINT('Origin',(141.458521203919,255.,37.9151793916432));
#47882=CARTESIAN_POINT('',(141.458521203919,15.,37.9151793916432));
#47883=CARTESIAN_POINT('',(141.458521203919,15.,39.4187321117283));
#47884=CARTESIAN_POINT('',(141.458521203919,495.,37.9151793916432));
#47885=CARTESIAN_POINT('',(141.458521203919,255.,37.9151793916432));
#47886=CARTESIAN_POINT('',(141.458521203919,495.,39.4187321117283));
#47887=CARTESIAN_POINT('Origin',(142.508521203919,255.,37.9151793916432));
#47888=CARTESIAN_POINT('',(141.763569006683,15.,37.1752157277839));
#47889=CARTESIAN_POINT('Origin',(142.508521203919,15.,37.9151793916432));
#47890=CARTESIAN_POINT('',(141.763569006683,495.,37.1752157277839));
#47891=CARTESIAN_POINT('',(141.763569006683,255.,37.1752157277839));
#47892=CARTESIAN_POINT('Origin',(142.508521203919,495.,37.9151793916432));
#47893=CARTESIAN_POINT('Origin',(144.544688744748,255.,34.375346814161));
#47894=CARTESIAN_POINT('',(144.544688744748,15.,34.375346814161));
#47895=CARTESIAN_POINT('',(144.544688744748,15.,34.375346814161));
#47896=CARTESIAN_POINT('',(144.544688744748,495.,34.375346814161));
#47897=CARTESIAN_POINT('',(144.544688744748,255.,34.375346814161));
#47898=CARTESIAN_POINT('',(144.544688744748,495.,34.375346814161));
#47899=CARTESIAN_POINT('Origin',(143.764262633357,255.,33.6001467853559));
#47900=CARTESIAN_POINT('',(144.864262633357,15.,33.6001467853559));
#47901=CARTESIAN_POINT('Origin',(143.764262633357,15.,33.6001467853559));
#47902=CARTESIAN_POINT('',(144.864262633357,495.,33.6001467853559));
#47903=CARTESIAN_POINT('',(144.864262633357,255.,33.6001467853559));
#47904=CARTESIAN_POINT('Origin',(143.764262633357,495.,33.6001467853559));
#47905=CARTESIAN_POINT('Origin',(144.864262633357,255.,31.0022770426652));
#47906=CARTESIAN_POINT('',(144.864262633357,15.,31.0022770426652));
#47907=CARTESIAN_POINT('',(144.864262633357,15.,31.0022770426652));
#47908=CARTESIAN_POINT('',(144.864262633357,495.,31.0022770426652));
#47909=CARTESIAN_POINT('',(144.864262633357,255.,31.0022770426652));
#47910=CARTESIAN_POINT('',(144.864262633357,495.,31.0022770426652));
#47911=CARTESIAN_POINT('Origin',(143.862749870693,255.,30.));
#47912=CARTESIAN_POINT('',(143.862749870693,15.,30.));
#47913=CARTESIAN_POINT('',(143.862749870693,15.,30.));
#47914=CARTESIAN_POINT('',(143.862749870693,495.,30.));
#47915=CARTESIAN_POINT('',(143.862749870693,255.,30.));
#47916=CARTESIAN_POINT('',(143.862749870693,495.,30.));
#47917=CARTESIAN_POINT('Origin',(129.866920906812,495.,38.7500402287547));
#47918=CARTESIAN_POINT('',(127.637659789347,495.,47.5000804575095));
#47919=CARTESIAN_POINT('',(144.864262633357,495.,47.5000804575095));
#47920=CARTESIAN_POINT('',(125.869319760628,495.,30.));
#47921=CARTESIAN_POINT('',(144.864262633357,495.,30.));
#47922=CARTESIAN_POINT('',(124.867806997963,495.,31.0022770426652));
#47923=CARTESIAN_POINT('',(125.869319760628,495.,30.));
#47924=CARTESIAN_POINT('',(124.867806997963,495.,33.6001467853559));
#47925=CARTESIAN_POINT('',(124.867806997963,495.,31.0022770426652));
#47926=CARTESIAN_POINT('',(125.187380886572,495.,34.375346814161));
#47927=CARTESIAN_POINT('Origin',(125.967806997963,495.,33.6001467853559));
#47928=CARTESIAN_POINT('',(127.968500624638,495.,37.1752157277839));
#47929=CARTESIAN_POINT('',(125.187380886572,495.,34.375346814161));
#47930=CARTESIAN_POINT('',(128.273548427401,495.,37.9151793916432));
#47931=CARTESIAN_POINT('Origin',(127.223548427401,495.,37.9151793916432));
#47932=CARTESIAN_POINT('',(128.273548427401,495.,39.4187321117283));
#47933=CARTESIAN_POINT('',(128.273548427401,495.,39.4187321117283));
#47934=CARTESIAN_POINT('',(127.971127263844,495.,40.1560420081102));
#47935=CARTESIAN_POINT('Origin',(127.223548427401,495.,39.4187321117283));
#47936=CARTESIAN_POINT('',(127.333356762198,495.,40.8026951072716));
#47937=CARTESIAN_POINT('',(127.971127263844,495.,40.1560420081102));
#47938=CARTESIAN_POINT('',(126.997701127708,495.,41.3560806824536));
#47939=CARTESIAN_POINT('Origin',(128.330128544122,495.,41.7857749691141));
#47940=CARTESIAN_POINT('',(125.328762843953,495.,42.9220241352404));
#47941=CARTESIAN_POINT('Origin',(124.747780443448,495.,40.6305041508116));
#47942=CARTESIAN_POINT('',(124.876218876064,495.,43.5036225521864));
#47943=CARTESIAN_POINT('Origin',(125.476218876064,495.,43.5036225521863));
#47944=CARTESIAN_POINT('',(124.876218876064,495.,44.4226470147914));
#47945=CARTESIAN_POINT('',(124.876218876064,495.,44.4226470147914));
#47946=CARTESIAN_POINT('',(125.387243744723,495.,45.1153516005764));
#47947=CARTESIAN_POINT('Origin',(125.601218876064,495.,44.4226470147914));
#47948=CARTESIAN_POINT('',(127.036092546462,495.,46.8112703207193));
#47949=CARTESIAN_POINT('Origin',(124.659008759128,495.,47.4728765656934));
#47950=CARTESIAN_POINT('',(127.149786002621,495.,47.007169160326));
#47951=CARTESIAN_POINT('Origin',(127.469614165074,495.,46.690609613792));
#47952=CARTESIAN_POINT('',(127.637659789347,495.,47.5000804575095));
#47953=CARTESIAN_POINT('Origin',(127.149786002621,255.,47.007169160326));
#47954=CARTESIAN_POINT('',(127.637659789347,15.,47.5000804575095));
#47955=CARTESIAN_POINT('',(127.637659789347,255.,47.5000804575095));
#47956=CARTESIAN_POINT('',(127.149786002621,15.,47.007169160326));
#47957=CARTESIAN_POINT('',(127.149786002621,255.,47.007169160326));
#47958=CARTESIAN_POINT('',(127.637659789347,15.,47.5000804575095));
#47959=CARTESIAN_POINT('Origin',(127.469614165074,255.,46.690609613792));
#47960=CARTESIAN_POINT('',(127.036092546462,15.,46.8112703207193));
#47961=CARTESIAN_POINT('',(127.036092546462,255.,46.8112703207193));
#47962=CARTESIAN_POINT('Origin',(127.469614165074,15.,46.690609613792));
#47963=CARTESIAN_POINT('Origin',(124.659008759128,255.,47.4728765656934));
#47964=CARTESIAN_POINT('',(125.387243744723,15.,45.1153516005764));
#47965=CARTESIAN_POINT('',(125.387243744723,255.,45.1153516005764));
#47966=CARTESIAN_POINT('Origin',(124.659008759128,15.,47.4728765656934));
#47967=CARTESIAN_POINT('Origin',(125.601218876064,255.,44.4226470147914));
#47968=CARTESIAN_POINT('',(124.876218876064,15.,44.4226470147914));
#47969=CARTESIAN_POINT('',(124.876218876064,255.,44.4226470147914));
#47970=CARTESIAN_POINT('Origin',(125.601218876064,15.,44.4226470147914));
#47971=CARTESIAN_POINT('Origin',(124.876218876064,255.,43.5036225521864));
#47972=CARTESIAN_POINT('',(124.876218876064,15.,43.5036225521864));
#47973=CARTESIAN_POINT('',(124.876218876064,255.,43.5036225521864));
#47974=CARTESIAN_POINT('',(124.876218876064,15.,44.4226470147914));
#47975=CARTESIAN_POINT('Origin',(125.476218876064,255.,43.5036225521863));
#47976=CARTESIAN_POINT('',(125.328762843953,15.,42.9220241352404));
#47977=CARTESIAN_POINT('',(125.328762843953,255.,42.9220241352404));
#47978=CARTESIAN_POINT('Origin',(125.476218876064,15.,43.5036225521863));
#47979=CARTESIAN_POINT('Origin',(124.747780443448,255.,40.6305041508116));
#47980=CARTESIAN_POINT('',(126.997701127708,15.,41.3560806824536));
#47981=CARTESIAN_POINT('',(126.997701127708,255.,41.3560806824536));
#47982=CARTESIAN_POINT('Origin',(124.747780443448,15.,40.6305041508116));
#47983=CARTESIAN_POINT('Origin',(128.330128544122,255.,41.7857749691141));
#47984=CARTESIAN_POINT('',(127.333356762198,15.,40.8026951072716));
#47985=CARTESIAN_POINT('',(127.333356762198,255.,40.8026951072716));
#47986=CARTESIAN_POINT('Origin',(128.330128544122,15.,41.7857749691141));
#47987=CARTESIAN_POINT('Origin',(127.971127263844,255.,40.1560420081102));
#47988=CARTESIAN_POINT('',(127.971127263844,15.,40.1560420081102));
#47989=CARTESIAN_POINT('',(127.971127263844,255.,40.1560420081102));
#47990=CARTESIAN_POINT('',(127.971127263844,15.,40.1560420081102));
#47991=CARTESIAN_POINT('Origin',(127.223548427401,255.,39.4187321117283));
#47992=CARTESIAN_POINT('',(128.273548427401,15.,39.4187321117283));
#47993=CARTESIAN_POINT('',(128.273548427401,255.,39.4187321117283));
#47994=CARTESIAN_POINT('Origin',(127.223548427401,15.,39.4187321117283));
#47995=CARTESIAN_POINT('Origin',(128.273548427401,255.,37.9151793916432));
#47996=CARTESIAN_POINT('',(128.273548427401,15.,37.9151793916432));
#47997=CARTESIAN_POINT('',(128.273548427401,255.,37.9151793916432));
#47998=CARTESIAN_POINT('',(128.273548427401,15.,39.4187321117283));
#47999=CARTESIAN_POINT('Origin',(127.223548427401,255.,37.9151793916432));
#48000=CARTESIAN_POINT('',(127.968500624638,15.,37.1752157277839));
#48001=CARTESIAN_POINT('',(127.968500624638,255.,37.1752157277839));
#48002=CARTESIAN_POINT('Origin',(127.223548427401,15.,37.9151793916432));
#48003=CARTESIAN_POINT('Origin',(125.187380886572,255.,34.375346814161));
#48004=CARTESIAN_POINT('',(125.187380886572,15.,34.375346814161));
#48005=CARTESIAN_POINT('',(125.187380886572,255.,34.375346814161));
#48006=CARTESIAN_POINT('',(125.187380886572,15.,34.375346814161));
#48007=CARTESIAN_POINT('Origin',(125.967806997963,255.,33.6001467853559));
#48008=CARTESIAN_POINT('',(124.867806997963,15.,33.6001467853559));
#48009=CARTESIAN_POINT('',(124.867806997963,255.,33.6001467853559));
#48010=CARTESIAN_POINT('Origin',(125.967806997963,15.,33.6001467853559));
#48011=CARTESIAN_POINT('Origin',(124.867806997963,255.,31.0022770426652));
#48012=CARTESIAN_POINT('',(124.867806997963,15.,31.0022770426652));
#48013=CARTESIAN_POINT('',(124.867806997963,255.,31.0022770426652));
#48014=CARTESIAN_POINT('',(124.867806997963,15.,31.0022770426652));
#48015=CARTESIAN_POINT('Origin',(125.869319760628,255.,30.));
#48016=CARTESIAN_POINT('',(125.869319760628,15.,30.));
#48017=CARTESIAN_POINT('',(125.869319760628,255.,30.));
#48018=CARTESIAN_POINT('',(125.869319760628,15.,30.));
#48019=CARTESIAN_POINT('Origin',(134.86603481566,255.,30.));
#48020=CARTESIAN_POINT('',(124.867806997963,15.,30.));
#48021=CARTESIAN_POINT('Origin',(127.637659789347,255.,47.5000804575095));
#48022=CARTESIAN_POINT('',(124.867806997963,15.,47.5000804575095));
#48023=CARTESIAN_POINT('Origin',(129.866920906812,15.,38.7500402287547));
#48024=CARTESIAN_POINT('',(0.,0.,0.));
#48025=CARTESIAN_POINT('Origin',(74.9879498948689,0.,53.0228109606356));
#48026=CARTESIAN_POINT('',(57.4879498948689,0.,53.0228109606356));
#48027=CARTESIAN_POINT('Origin',(74.9879498948689,0.,53.0228109606356));
#48028=CARTESIAN_POINT('',(57.4879498948689,15.,53.0228109606356));
#48029=CARTESIAN_POINT('',(57.4879498948689,0.,53.0228109606356));
#48030=CARTESIAN_POINT('Origin',(74.9879498948689,15.,53.0228109606356));
#48031=CARTESIAN_POINT('Origin',(0.,0.,0.));
#48032=CARTESIAN_POINT('',(0.,0.,85.));
#48033=CARTESIAN_POINT('',(0.,0.,0.));
#48034=CARTESIAN_POINT('',(0.,0.,85.));
#48035=CARTESIAN_POINT('',(0.,15.,85.));
#48036=CARTESIAN_POINT('',(0.,0.,85.));
#48037=CARTESIAN_POINT('',(0.,15.,0.));
#48038=CARTESIAN_POINT('',(0.,15.,85.));
#48039=CARTESIAN_POINT('',(0.,0.,0.));
#48040=CARTESIAN_POINT('Origin',(150.,0.,0.));
#48041=CARTESIAN_POINT('',(150.,0.,0.));
#48042=CARTESIAN_POINT('',(0.,0.,0.));
#48043=CARTESIAN_POINT('',(150.,15.,0.));
#48044=CARTESIAN_POINT('',(0.,15.,0.));
#48045=CARTESIAN_POINT('',(150.,0.,0.));
#48046=CARTESIAN_POINT('Origin',(150.,0.,85.));
#48047=CARTESIAN_POINT('',(150.,0.,85.));
#48048=CARTESIAN_POINT('',(150.,0.,0.));
#48049=CARTESIAN_POINT('',(150.,15.,85.));
#48050=CARTESIAN_POINT('',(150.,15.,0.));
#48051=CARTESIAN_POINT('',(150.,0.,85.));
#48052=CARTESIAN_POINT('Origin',(0.,0.,85.));
#48053=CARTESIAN_POINT('',(150.,0.,85.));
#48054=CARTESIAN_POINT('',(150.,15.,85.));
#48055=CARTESIAN_POINT('Origin',(75.,15.,42.5));
#48056=CARTESIAN_POINT('Origin',(75.,0.,42.5));
#48057=CARTESIAN_POINT('',(0.,0.,0.));
#48058=CARTESIAN_POINT('Origin',(74.9879498948689,510.,53.0228109606356));
#48059=CARTESIAN_POINT('',(79.9879498948689,510.,53.0228109606356));
#48060=CARTESIAN_POINT('Origin',(74.9879498948689,510.,53.0228109606356));
#48061=CARTESIAN_POINT('',(79.9879498948689,495.,53.0228109606356));
#48062=CARTESIAN_POINT('',(79.9879498948689,510.,53.0228109606356));
#48063=CARTESIAN_POINT('Origin',(74.9879498948689,495.,53.0228109606356));
#48064=CARTESIAN_POINT('Origin',(0.,495.,0.));
#48065=CARTESIAN_POINT('',(0.,495.,95.));
#48066=CARTESIAN_POINT('',(0.,495.,0.));
#48067=CARTESIAN_POINT('',(0.,495.,85.));
#48068=CARTESIAN_POINT('',(0.,510.,95.));
#48069=CARTESIAN_POINT('',(0.,495.,95.));
#48070=CARTESIAN_POINT('',(0.,510.,0.));
#48071=CARTESIAN_POINT('',(0.,510.,85.));
#48072=CARTESIAN_POINT('',(0.,495.,0.));
#48073=CARTESIAN_POINT('Origin',(150.,495.,0.));
#48074=CARTESIAN_POINT('',(150.,495.,0.));
#48075=CARTESIAN_POINT('',(0.,495.,0.));
#48076=CARTESIAN_POINT('',(150.,510.,0.));
#48077=CARTESIAN_POINT('',(0.,510.,0.));
#48078=CARTESIAN_POINT('',(150.,495.,0.));
#48079=CARTESIAN_POINT('Origin',(150.,495.,85.));
#48080=CARTESIAN_POINT('',(150.,495.,95.));
#48081=CARTESIAN_POINT('',(150.,495.,0.));
#48082=CARTESIAN_POINT('',(150.,510.,95.));
#48083=CARTESIAN_POINT('',(150.,510.,0.));
#48084=CARTESIAN_POINT('',(150.,495.,95.));
#48085=CARTESIAN_POINT('Origin',(0.,495.,95.));
#48086=CARTESIAN_POINT('',(37.5,495.,95.));
#48087=CARTESIAN_POINT('',(37.5,510.,95.));
#48088=CARTESIAN_POINT('Origin',(75.,510.,42.5));
#48089=CARTESIAN_POINT('Origin',(75.,495.,42.5));
#48090=CARTESIAN_POINT('',(0.,0.,0.));
#48091=CARTESIAN_POINT('Origin',(74.9879498948689,415.,53.0228109606356));
#48092=CARTESIAN_POINT('',(92.4879498948689,435.,53.0228109606356));
#48093=CARTESIAN_POINT('Origin',(74.9879498948689,435.,53.0228109606356));
#48094=CARTESIAN_POINT('',(92.4879498948689,415.,53.0228109606356));
#48095=CARTESIAN_POINT('',(92.4879498948689,415.,53.0228109606356));
#48096=CARTESIAN_POINT('Origin',(74.9879498948689,415.,53.0228109606356));
#48097=CARTESIAN_POINT('Origin',(37.9634359091503,415.,30.));
#48098=CARTESIAN_POINT('',(37.9634359091503,415.,30.));
#48099=CARTESIAN_POINT('',(37.9634359091503,415.,76.0456219212711));
#48100=CARTESIAN_POINT('',(37.9634359091503,415.,30.));
#48101=CARTESIAN_POINT('',(37.9634359091503,435.,76.0456219212711));
#48102=CARTESIAN_POINT('',(37.9634359091503,415.,76.0456219212711));
#48103=CARTESIAN_POINT('',(37.9634359091503,435.,30.));
#48104=CARTESIAN_POINT('',(37.9634359091503,435.,30.));
#48105=CARTESIAN_POINT('',(37.9634359091503,415.,30.));
#48106=CARTESIAN_POINT('Origin',(112.012463880588,415.,30.));
#48107=CARTESIAN_POINT('',(112.012463880588,415.,30.));
#48108=CARTESIAN_POINT('',(112.012463880588,415.,30.));
#48109=CARTESIAN_POINT('',(112.012463880588,435.,30.));
#48110=CARTESIAN_POINT('',(112.012463880588,435.,30.));
#48111=CARTESIAN_POINT('',(112.012463880588,415.,30.));
#48112=CARTESIAN_POINT('Origin',(112.012463880588,415.,76.0456219212711));
#48113=CARTESIAN_POINT('',(112.012463880588,415.,76.0456219212711));
#48114=CARTESIAN_POINT('',(112.012463880588,415.,76.0456219212711));
#48115=CARTESIAN_POINT('',(112.012463880588,435.,76.0456219212711));
#48116=CARTESIAN_POINT('',(112.012463880588,435.,76.0456219212711));
#48117=CARTESIAN_POINT('',(112.012463880588,415.,76.0456219212711));
#48118=CARTESIAN_POINT('Origin',(37.9634359091503,415.,76.0456219212711));
#48119=CARTESIAN_POINT('',(37.9634359091503,415.,76.0456219212711));
#48120=CARTESIAN_POINT('',(37.9634359091503,435.,76.0456219212711));
#48121=CARTESIAN_POINT('Origin',(74.9879498948689,415.,53.0228109606356));
#48122=CARTESIAN_POINT('Origin',(74.9879498948689,435.,53.0228109606356));
#48123=CARTESIAN_POINT('',(0.,0.,0.));
#48124=CARTESIAN_POINT('Origin',(7.41771637130031,255.,47.007169160326));
#48125=CARTESIAN_POINT('',(7.90559015802673,15.,47.5000804575095));
#48126=CARTESIAN_POINT('',(7.90559015802673,495.,47.5000804575095));
#48127=CARTESIAN_POINT('',(7.90559015802673,255.,47.5000804575095));
#48128=CARTESIAN_POINT('',(7.41771637130031,495.,47.007169160326));
#48129=CARTESIAN_POINT('',(7.90559015802673,495.,47.5000804575095));
#48130=CARTESIAN_POINT('',(7.41771637130031,15.,47.007169160326));
#48131=CARTESIAN_POINT('',(7.41771637130031,255.,47.007169160326));
#48132=CARTESIAN_POINT('',(7.90559015802673,15.,47.5000804575095));
#48133=CARTESIAN_POINT('Origin',(7.73754453375374,255.,46.690609613792));
#48134=CARTESIAN_POINT('',(7.30402291514177,495.,46.8112703207193));
#48135=CARTESIAN_POINT('Origin',(7.73754453375374,495.,46.690609613792));
#48136=CARTESIAN_POINT('',(7.30402291514177,15.,46.8112703207193));
#48137=CARTESIAN_POINT('',(7.30402291514177,255.,46.8112703207193));
#48138=CARTESIAN_POINT('Origin',(7.73754453375374,15.,46.690609613792));
#48139=CARTESIAN_POINT('Origin',(4.92693912780791,255.,47.4728765656934));
#48140=CARTESIAN_POINT('',(5.65517411340273,495.,45.1153516005764));
#48141=CARTESIAN_POINT('Origin',(4.92693912780791,495.,47.4728765656934));
#48142=CARTESIAN_POINT('',(5.65517411340273,15.,45.1153516005764));
#48143=CARTESIAN_POINT('',(5.65517411340273,255.,45.1153516005764));
#48144=CARTESIAN_POINT('Origin',(4.92693912780791,15.,47.4728765656934));
#48145=CARTESIAN_POINT('Origin',(5.86914924474375,255.,44.4226470147914));
#48146=CARTESIAN_POINT('',(5.14414924474374,495.,44.4226470147914));
#48147=CARTESIAN_POINT('Origin',(5.86914924474375,495.,44.4226470147914));
#48148=CARTESIAN_POINT('',(5.14414924474374,15.,44.4226470147914));
#48149=CARTESIAN_POINT('',(5.14414924474374,255.,44.4226470147914));
#48150=CARTESIAN_POINT('Origin',(5.86914924474375,15.,44.4226470147914));
#48151=CARTESIAN_POINT('Origin',(5.14414924474375,255.,43.5036225521864));
#48152=CARTESIAN_POINT('',(5.14414924474375,495.,43.5036225521864));
#48153=CARTESIAN_POINT('',(5.14414924474374,495.,44.4226470147914));
#48154=CARTESIAN_POINT('',(5.14414924474375,15.,43.5036225521864));
#48155=CARTESIAN_POINT('',(5.14414924474375,255.,43.5036225521864));
#48156=CARTESIAN_POINT('',(5.14414924474374,15.,44.4226470147914));
#48157=CARTESIAN_POINT('Origin',(5.74414924474373,255.,43.5036225521863));
#48158=CARTESIAN_POINT('',(5.59669321263261,495.,42.9220241352404));
#48159=CARTESIAN_POINT('Origin',(5.74414924474373,495.,43.5036225521863));
#48160=CARTESIAN_POINT('',(5.59669321263261,15.,42.9220241352404));
#48161=CARTESIAN_POINT('',(5.59669321263261,255.,42.9220241352404));
#48162=CARTESIAN_POINT('Origin',(5.74414924474373,15.,43.5036225521863));
#48163=CARTESIAN_POINT('Origin',(5.01571081212747,255.,40.6305041508116));
#48164=CARTESIAN_POINT('',(7.26563149638805,495.,41.3560806824536));
#48165=CARTESIAN_POINT('Origin',(5.01571081212747,495.,40.6305041508116));
#48166=CARTESIAN_POINT('',(7.26563149638805,15.,41.3560806824536));
#48167=CARTESIAN_POINT('',(7.26563149638805,255.,41.3560806824536));
#48168=CARTESIAN_POINT('Origin',(5.01571081212747,15.,40.6305041508116));
#48169=CARTESIAN_POINT('Origin',(8.59805891280186,255.,41.7857749691141));
#48170=CARTESIAN_POINT('',(7.60128713087801,495.,40.8026951072716));
#48171=CARTESIAN_POINT('Origin',(8.59805891280186,495.,41.7857749691141));
#48172=CARTESIAN_POINT('',(7.60128713087801,15.,40.8026951072716));
#48173=CARTESIAN_POINT('',(7.60128713087801,255.,40.8026951072716));
#48174=CARTESIAN_POINT('Origin',(8.59805891280186,15.,41.7857749691141));
#48175=CARTESIAN_POINT('Origin',(8.23905763252352,255.,40.1560420081102));
#48176=CARTESIAN_POINT('',(8.23905763252352,495.,40.1560420081102));
#48177=CARTESIAN_POINT('',(8.23905763252352,495.,40.1560420081102));
#48178=CARTESIAN_POINT('',(8.23905763252352,15.,40.1560420081102));
#48179=CARTESIAN_POINT('',(8.23905763252352,255.,40.1560420081102));
#48180=CARTESIAN_POINT('',(8.23905763252352,15.,40.1560420081102));
#48181=CARTESIAN_POINT('Origin',(7.49147879608061,255.,39.4187321117283));
#48182=CARTESIAN_POINT('',(8.54147879608062,495.,39.4187321117283));
#48183=CARTESIAN_POINT('Origin',(7.49147879608061,495.,39.4187321117283));
#48184=CARTESIAN_POINT('',(8.54147879608062,15.,39.4187321117283));
#48185=CARTESIAN_POINT('',(8.54147879608062,255.,39.4187321117283));
#48186=CARTESIAN_POINT('Origin',(7.49147879608061,15.,39.4187321117283));
#48187=CARTESIAN_POINT('Origin',(8.54147879608062,255.,37.9151793916432));
#48188=CARTESIAN_POINT('',(8.54147879608062,495.,37.9151793916432));
#48189=CARTESIAN_POINT('',(8.54147879608062,495.,39.4187321117283));
#48190=CARTESIAN_POINT('',(8.54147879608062,15.,37.9151793916432));
#48191=CARTESIAN_POINT('',(8.54147879608062,255.,37.9151793916432));
#48192=CARTESIAN_POINT('',(8.54147879608062,15.,39.4187321117283));
#48193=CARTESIAN_POINT('Origin',(7.49147879608066,255.,37.9151793916432));
#48194=CARTESIAN_POINT('',(8.23643099331736,495.,37.1752157277839));
#48195=CARTESIAN_POINT('Origin',(7.49147879608066,495.,37.9151793916432));
#48196=CARTESIAN_POINT('',(8.23643099331736,15.,37.1752157277839));
#48197=CARTESIAN_POINT('',(8.23643099331736,255.,37.1752157277839));
#48198=CARTESIAN_POINT('Origin',(7.49147879608066,15.,37.9151793916432));
#48199=CARTESIAN_POINT('Origin',(5.4553112552519,255.,34.375346814161));
#48200=CARTESIAN_POINT('',(5.4553112552519,495.,34.375346814161));
#48201=CARTESIAN_POINT('',(5.4553112552519,495.,34.375346814161));
#48202=CARTESIAN_POINT('',(5.4553112552519,15.,34.375346814161));
#48203=CARTESIAN_POINT('',(5.4553112552519,255.,34.375346814161));
#48204=CARTESIAN_POINT('',(5.4553112552519,15.,34.375346814161));
#48205=CARTESIAN_POINT('Origin',(6.23573736664277,255.,33.6001467853559));
#48206=CARTESIAN_POINT('',(5.13573736664277,495.,33.6001467853559));
#48207=CARTESIAN_POINT('Origin',(6.23573736664277,495.,33.6001467853559));
#48208=CARTESIAN_POINT('',(5.13573736664277,15.,33.6001467853559));
#48209=CARTESIAN_POINT('',(5.13573736664277,255.,33.6001467853559));
#48210=CARTESIAN_POINT('Origin',(6.23573736664277,15.,33.6001467853559));
#48211=CARTESIAN_POINT('Origin',(5.13573736664277,255.,31.0022770426652));
#48212=CARTESIAN_POINT('',(5.13573736664277,495.,31.0022770426652));
#48213=CARTESIAN_POINT('',(5.13573736664277,495.,31.0022770426652));
#48214=CARTESIAN_POINT('',(5.13573736664277,15.,31.0022770426652));
#48215=CARTESIAN_POINT('',(5.13573736664277,255.,31.0022770426652));
#48216=CARTESIAN_POINT('',(5.13573736664277,15.,31.0022770426652));
#48217=CARTESIAN_POINT('Origin',(6.13725012930742,255.,30.));
#48218=CARTESIAN_POINT('',(6.13725012930742,495.,30.));
#48219=CARTESIAN_POINT('',(6.13725012930742,495.,30.));
#48220=CARTESIAN_POINT('',(6.13725012930742,15.,30.));
#48221=CARTESIAN_POINT('',(6.13725012930742,255.,30.));
#48222=CARTESIAN_POINT('',(6.13725012930742,15.,30.));
#48223=CARTESIAN_POINT('Origin',(20.1330790931884,495.,38.7500402287547));
#48224=CARTESIAN_POINT('',(22.362340210653,495.,47.5000804575095));
#48225=CARTESIAN_POINT('',(5.13573736664277,495.,47.5000804575095));
#48226=CARTESIAN_POINT('',(22.8502139973794,495.,47.007169160326));
#48227=CARTESIAN_POINT('',(22.362340210653,495.,47.5000804575095));
#48228=CARTESIAN_POINT('',(22.963907453538,495.,46.8112703207193));
#48229=CARTESIAN_POINT('Origin',(22.530385834926,495.,46.690609613792));
#48230=CARTESIAN_POINT('',(24.612756255277,495.,45.1153516005764));
#48231=CARTESIAN_POINT('Origin',(25.3409912408718,495.,47.4728765656934));
#48232=CARTESIAN_POINT('',(25.123781123936,495.,44.4226470147914));
#48233=CARTESIAN_POINT('Origin',(24.398781123936,495.,44.4226470147914));
#48234=CARTESIAN_POINT('',(25.123781123936,495.,43.5036225521864));
#48235=CARTESIAN_POINT('',(25.123781123936,495.,44.4226470147914));
#48236=CARTESIAN_POINT('',(24.6712371560471,495.,42.9220241352404));
#48237=CARTESIAN_POINT('Origin',(24.523781123936,495.,43.5036225521863));
#48238=CARTESIAN_POINT('',(23.0022988722917,495.,41.3560806824536));
#48239=CARTESIAN_POINT('Origin',(25.2522195565523,495.,40.6305041508116));
#48240=CARTESIAN_POINT('',(22.6666432378017,495.,40.8026951072716));
#48241=CARTESIAN_POINT('Origin',(21.6698714558779,495.,41.7857749691141));
#48242=CARTESIAN_POINT('',(22.0288727361562,495.,40.1560420081102));
#48243=CARTESIAN_POINT('',(22.0288727361562,495.,40.1560420081102));
#48244=CARTESIAN_POINT('',(21.7264515725991,495.,39.4187321117283));
#48245=CARTESIAN_POINT('Origin',(22.7764515725991,495.,39.4187321117283));
#48246=CARTESIAN_POINT('',(21.7264515725991,495.,37.9151793916432));
#48247=CARTESIAN_POINT('',(21.7264515725991,495.,39.4187321117283));
#48248=CARTESIAN_POINT('',(22.0314993753624,495.,37.1752157277839));
#48249=CARTESIAN_POINT('Origin',(22.7764515725991,495.,37.9151793916432));
#48250=CARTESIAN_POINT('',(24.8126191134278,495.,34.375346814161));
#48251=CARTESIAN_POINT('',(24.8126191134278,495.,34.375346814161));
#48252=CARTESIAN_POINT('',(25.132193002037,495.,33.6001467853559));
#48253=CARTESIAN_POINT('Origin',(24.032193002037,495.,33.6001467853559));
#48254=CARTESIAN_POINT('',(25.132193002037,495.,31.0022770426652));
#48255=CARTESIAN_POINT('',(25.132193002037,495.,31.0022770426652));
#48256=CARTESIAN_POINT('',(24.1306802393723,495.,30.));
#48257=CARTESIAN_POINT('',(24.1306802393723,495.,30.));
#48258=CARTESIAN_POINT('',(5.13573736664278,495.,30.));
#48259=CARTESIAN_POINT('Origin',(22.8502139973794,255.,47.007169160326));
#48260=CARTESIAN_POINT('',(22.362340210653,15.,47.5000804575095));
#48261=CARTESIAN_POINT('',(22.362340210653,255.,47.5000804575095));
#48262=CARTESIAN_POINT('',(22.8502139973794,15.,47.007169160326));
#48263=CARTESIAN_POINT('',(22.362340210653,15.,47.5000804575095));
#48264=CARTESIAN_POINT('',(22.8502139973794,255.,47.007169160326));
#48265=CARTESIAN_POINT('Origin',(22.530385834926,255.,46.690609613792));
#48266=CARTESIAN_POINT('',(22.963907453538,15.,46.8112703207193));
#48267=CARTESIAN_POINT('Origin',(22.530385834926,15.,46.690609613792));
#48268=CARTESIAN_POINT('',(22.963907453538,255.,46.8112703207193));
#48269=CARTESIAN_POINT('Origin',(25.3409912408718,255.,47.4728765656934));
#48270=CARTESIAN_POINT('',(24.612756255277,15.,45.1153516005764));
#48271=CARTESIAN_POINT('Origin',(25.3409912408718,15.,47.4728765656934));
#48272=CARTESIAN_POINT('',(24.612756255277,255.,45.1153516005764));
#48273=CARTESIAN_POINT('Origin',(24.398781123936,255.,44.4226470147914));
#48274=CARTESIAN_POINT('',(25.123781123936,15.,44.4226470147914));
#48275=CARTESIAN_POINT('Origin',(24.398781123936,15.,44.4226470147914));
#48276=CARTESIAN_POINT('',(25.123781123936,255.,44.4226470147914));
#48277=CARTESIAN_POINT('Origin',(25.123781123936,255.,43.5036225521864));
#48278=CARTESIAN_POINT('',(25.123781123936,15.,43.5036225521864));
#48279=CARTESIAN_POINT('',(25.123781123936,15.,44.4226470147914));
#48280=CARTESIAN_POINT('',(25.123781123936,255.,43.5036225521864));
#48281=CARTESIAN_POINT('Origin',(24.523781123936,255.,43.5036225521863));
#48282=CARTESIAN_POINT('',(24.6712371560471,15.,42.9220241352404));
#48283=CARTESIAN_POINT('Origin',(24.523781123936,15.,43.5036225521863));
#48284=CARTESIAN_POINT('',(24.6712371560471,255.,42.9220241352404));
#48285=CARTESIAN_POINT('Origin',(25.2522195565523,255.,40.6305041508116));
#48286=CARTESIAN_POINT('',(23.0022988722917,15.,41.3560806824536));
#48287=CARTESIAN_POINT('Origin',(25.2522195565523,15.,40.6305041508116));
#48288=CARTESIAN_POINT('',(23.0022988722917,255.,41.3560806824536));
#48289=CARTESIAN_POINT('Origin',(21.6698714558779,255.,41.7857749691141));
#48290=CARTESIAN_POINT('',(22.6666432378017,15.,40.8026951072716));
#48291=CARTESIAN_POINT('Origin',(21.6698714558779,15.,41.7857749691141));
#48292=CARTESIAN_POINT('',(22.6666432378017,255.,40.8026951072716));
#48293=CARTESIAN_POINT('Origin',(22.0288727361562,255.,40.1560420081102));
#48294=CARTESIAN_POINT('',(22.0288727361562,15.,40.1560420081102));
#48295=CARTESIAN_POINT('',(22.0288727361562,15.,40.1560420081102));
#48296=CARTESIAN_POINT('',(22.0288727361562,255.,40.1560420081102));
#48297=CARTESIAN_POINT('Origin',(22.7764515725991,255.,39.4187321117283));
#48298=CARTESIAN_POINT('',(21.7264515725991,15.,39.4187321117283));
#48299=CARTESIAN_POINT('Origin',(22.7764515725991,15.,39.4187321117283));
#48300=CARTESIAN_POINT('',(21.7264515725991,255.,39.4187321117283));
#48301=CARTESIAN_POINT('Origin',(21.7264515725991,255.,37.9151793916432));
#48302=CARTESIAN_POINT('',(21.7264515725991,15.,37.9151793916432));
#48303=CARTESIAN_POINT('',(21.7264515725991,15.,39.4187321117283));
#48304=CARTESIAN_POINT('',(21.7264515725991,255.,37.9151793916432));
#48305=CARTESIAN_POINT('Origin',(22.7764515725991,255.,37.9151793916432));
#48306=CARTESIAN_POINT('',(22.0314993753624,15.,37.1752157277839));
#48307=CARTESIAN_POINT('Origin',(22.7764515725991,15.,37.9151793916432));
#48308=CARTESIAN_POINT('',(22.0314993753624,255.,37.1752157277839));
#48309=CARTESIAN_POINT('Origin',(24.8126191134278,255.,34.375346814161));
#48310=CARTESIAN_POINT('',(24.8126191134278,15.,34.375346814161));
#48311=CARTESIAN_POINT('',(24.8126191134278,15.,34.375346814161));
#48312=CARTESIAN_POINT('',(24.8126191134278,255.,34.375346814161));
#48313=CARTESIAN_POINT('Origin',(24.032193002037,255.,33.6001467853559));
#48314=CARTESIAN_POINT('',(25.132193002037,15.,33.6001467853559));
#48315=CARTESIAN_POINT('Origin',(24.032193002037,15.,33.6001467853559));
#48316=CARTESIAN_POINT('',(25.132193002037,255.,33.6001467853559));
#48317=CARTESIAN_POINT('Origin',(25.132193002037,255.,31.0022770426652));
#48318=CARTESIAN_POINT('',(25.132193002037,15.,31.0022770426652));
#48319=CARTESIAN_POINT('',(25.132193002037,15.,31.0022770426652));
#48320=CARTESIAN_POINT('',(25.132193002037,255.,31.0022770426652));
#48321=CARTESIAN_POINT('Origin',(24.1306802393723,255.,30.));
#48322=CARTESIAN_POINT('',(24.1306802393723,15.,30.));
#48323=CARTESIAN_POINT('',(24.1306802393723,15.,30.));
#48324=CARTESIAN_POINT('',(24.1306802393723,255.,30.));
#48325=CARTESIAN_POINT('Origin',(15.1339651843399,255.,30.));
#48326=CARTESIAN_POINT('',(25.132193002037,15.,30.));
#48327=CARTESIAN_POINT('Origin',(22.362340210653,255.,47.5000804575095));
#48328=CARTESIAN_POINT('',(25.132193002037,15.,47.5000804575095));
#48329=CARTESIAN_POINT('Origin',(20.1330790931884,15.,38.7500402287547));
#48330=CARTESIAN_POINT('',(0.,0.,0.));
#48331=CARTESIAN_POINT('',(74.9879498948689,7.43965228946858,53.0228109606356));
#48332=CARTESIAN_POINT('',(150.,0.,0.));
#48333=CARTESIAN_POINT('',(150.,-100.,0.));
#48334=CARTESIAN_POINT('',(0.,-100.,0.));
#48335=CARTESIAN_POINT('',(74.9879498948689,425.060347710531,53.0228109606356));
#48336=CARTESIAN_POINT('',(0.,0.,0.));
#48337=CARTESIAN_POINT('',(0.,0.,0.));
#48338=CARTESIAN_POINT('',(0.,0.,0.));
#48339=CARTESIAN_POINT('',(0.,0.,0.));
#48340=CARTESIAN_POINT('',(0.,0.,0.));
#48341=CARTESIAN_POINT('',(0.,0.,0.));
#48342=CARTESIAN_POINT('',(0.,0.,0.));
#48343=CARTESIAN_POINT('',(0.,0.,0.));
#48344=UNCERTAINTY_MEASURE_WITH_UNIT(LENGTH_MEASURE(0.01),#48370,
'DISTANCE_ACCURACY_VALUE',
'Maximum model space distance between geometric entities at asserted c
onnectivities');
#48345=UNCERTAINTY_MEASURE_WITH_UNIT(LENGTH_MEASURE(0.01),#48370,
'DISTANCE_ACCURACY_VALUE',
'Maximum model space distance between geometric entities at asserted c
onnectivities');
#48346=UNCERTAINTY_MEASURE_WITH_UNIT(LENGTH_MEASURE(0.01),#48370,
'DISTANCE_ACCURACY_VALUE',
'Maximum model space distance between geometric entities at asserted c
onnectivities');
#48347=UNCERTAINTY_MEASURE_WITH_UNIT(LENGTH_MEASURE(0.01),#48370,
'DISTANCE_ACCURACY_VALUE',
'Maximum model space distance between geometric entities at asserted c
onnectivities');
#48348=UNCERTAINTY_MEASURE_WITH_UNIT(LENGTH_MEASURE(0.01),#48370,
'DISTANCE_ACCURACY_VALUE',
'Maximum model space distance between geometric entities at asserted c
onnectivities');
#48349=UNCERTAINTY_MEASURE_WITH_UNIT(LENGTH_MEASURE(0.01),#48370,
'DISTANCE_ACCURACY_VALUE',
'Maximum model space distance between geometric entities at asserted c
onnectivities');
#48350=UNCERTAINTY_MEASURE_WITH_UNIT(LENGTH_MEASURE(0.01),#48370,
'DISTANCE_ACCURACY_VALUE',
'Maximum model space distance between geometric entities at asserted c
onnectivities');
#48351=UNCERTAINTY_MEASURE_WITH_UNIT(LENGTH_MEASURE(0.01),#48370,
'DISTANCE_ACCURACY_VALUE',
'Maximum model space distance between geometric entities at asserted c
onnectivities');
#48352=UNCERTAINTY_MEASURE_WITH_UNIT(LENGTH_MEASURE(0.01),#48370,
'DISTANCE_ACCURACY_VALUE',
'Maximum model space distance between geometric entities at asserted c
onnectivities');
#48353=UNCERTAINTY_MEASURE_WITH_UNIT(LENGTH_MEASURE(0.01),#48370,
'DISTANCE_ACCURACY_VALUE',
'Maximum model space distance between geometric entities at asserted c
onnectivities');
#48354=UNCERTAINTY_MEASURE_WITH_UNIT(LENGTH_MEASURE(0.01),#48370,
'DISTANCE_ACCURACY_VALUE',
'Maximum model space distance between geometric entities at asserted c
onnectivities');
#48355=UNCERTAINTY_MEASURE_WITH_UNIT(LENGTH_MEASURE(0.01),#48370,
'DISTANCE_ACCURACY_VALUE',
'Maximum model space distance between geometric entities at asserted c
onnectivities');
#48356=UNCERTAINTY_MEASURE_WITH_UNIT(LENGTH_MEASURE(0.01),#48370,
'DISTANCE_ACCURACY_VALUE',
'Maximum model space distance between geometric entities at asserted c
onnectivities');
#48357=(
GEOMETRIC_REPRESENTATION_CONTEXT(3)
GLOBAL_UNCERTAINTY_ASSIGNED_CONTEXT((#48344))
GLOBAL_UNIT_ASSIGNED_CONTEXT((#48370,#48372,#48373))
REPRESENTATION_CONTEXT('','3D')
);
#48358=(
GEOMETRIC_REPRESENTATION_CONTEXT(3)
GLOBAL_UNCERTAINTY_ASSIGNED_CONTEXT((#48345))
GLOBAL_UNIT_ASSIGNED_CONTEXT((#48370,#48372,#48373))
REPRESENTATION_CONTEXT('','3D')
);
#48359=(
GEOMETRIC_REPRESENTATION_CONTEXT(3)
GLOBAL_UNCERTAINTY_ASSIGNED_CONTEXT((#48346))
GLOBAL_UNIT_ASSIGNED_CONTEXT((#48370,#48372,#48373))
REPRESENTATION_CONTEXT('','3D')
);
#48360=(
GEOMETRIC_REPRESENTATION_CONTEXT(3)
GLOBAL_UNCERTAINTY_ASSIGNED_CONTEXT((#48347))
GLOBAL_UNIT_ASSIGNED_CONTEXT((#48370,#48372,#48373))
REPRESENTATION_CONTEXT('','3D')
);
#48361=(
GEOMETRIC_REPRESENTATION_CONTEXT(3)
GLOBAL_UNCERTAINTY_ASSIGNED_CONTEXT((#48348))
GLOBAL_UNIT_ASSIGNED_CONTEXT((#48370,#48372,#48373))
REPRESENTATION_CONTEXT('','3D')
);
#48362=(
GEOMETRIC_REPRESENTATION_CONTEXT(3)
GLOBAL_UNCERTAINTY_ASSIGNED_CONTEXT((#48349))
GLOBAL_UNIT_ASSIGNED_CONTEXT((#48370,#48372,#48373))
REPRESENTATION_CONTEXT('','3D')
);
#48363=(
GEOMETRIC_REPRESENTATION_CONTEXT(3)
GLOBAL_UNCERTAINTY_ASSIGNED_CONTEXT((#48350))
GLOBAL_UNIT_ASSIGNED_CONTEXT((#48370,#48372,#48373))
REPRESENTATION_CONTEXT('','3D')
);
#48364=(
GEOMETRIC_REPRESENTATION_CONTEXT(3)
GLOBAL_UNCERTAINTY_ASSIGNED_CONTEXT((#48351))
GLOBAL_UNIT_ASSIGNED_CONTEXT((#48370,#48372,#48373))
REPRESENTATION_CONTEXT('','3D')
);
#48365=(
GEOMETRIC_REPRESENTATION_CONTEXT(3)
GLOBAL_UNCERTAINTY_ASSIGNED_CONTEXT((#48352))
GLOBAL_UNIT_ASSIGNED_CONTEXT((#48370,#48372,#48373))
REPRESENTATION_CONTEXT('','3D')
);
#48366=(
GEOMETRIC_REPRESENTATION_CONTEXT(3)
GLOBAL_UNCERTAINTY_ASSIGNED_CONTEXT((#48353))
GLOBAL_UNIT_ASSIGNED_CONTEXT((#48370,#48372,#48373))
REPRESENTATION_CONTEXT('','3D')
);
#48367=(
GEOMETRIC_REPRESENTATION_CONTEXT(3)
GLOBAL_UNCERTAINTY_ASSIGNED_CONTEXT((#48354))
GLOBAL_UNIT_ASSIGNED_CONTEXT((#48370,#48372,#48373))
REPRESENTATION_CONTEXT('','3D')
);
#48368=(
GEOMETRIC_REPRESENTATION_CONTEXT(3)
GLOBAL_UNCERTAINTY_ASSIGNED_CONTEXT((#48355))
GLOBAL_UNIT_ASSIGNED_CONTEXT((#48370,#48372,#48373))
REPRESENTATION_CONTEXT('','3D')
);
#48369=(
GEOMETRIC_REPRESENTATION_CONTEXT(3)
GLOBAL_UNCERTAINTY_ASSIGNED_CONTEXT((#48356))
GLOBAL_UNIT_ASSIGNED_CONTEXT((#48370,#48372,#48373))
REPRESENTATION_CONTEXT('','3D')
);
#48370=(
LENGTH_UNIT()
NAMED_UNIT(*)
SI_UNIT(.MILLI.,.METRE.)
);
#48371=(
LENGTH_UNIT()
NAMED_UNIT(*)
SI_UNIT($,.METRE.)
);
#48372=(
NAMED_UNIT(*)
PLANE_ANGLE_UNIT()
SI_UNIT($,.RADIAN.)
);
#48373=(
NAMED_UNIT(*)
SI_UNIT($,.STERADIAN.)
SOLID_ANGLE_UNIT()
);
#48374=SHAPE_DEFINITION_REPRESENTATION(#48386,#48412);
#48375=SHAPE_DEFINITION_REPRESENTATION(#48387,#48413);
#48376=SHAPE_DEFINITION_REPRESENTATION(#48388,#48414);
#48377=SHAPE_DEFINITION_REPRESENTATION(#48389,#48415);
#48378=SHAPE_DEFINITION_REPRESENTATION(#48390,#48416);
#48379=SHAPE_DEFINITION_REPRESENTATION(#48391,#48417);
#48380=SHAPE_DEFINITION_REPRESENTATION(#48392,#48418);
#48381=SHAPE_DEFINITION_REPRESENTATION(#48393,#48419);
#48382=SHAPE_DEFINITION_REPRESENTATION(#48394,#48420);
#48383=SHAPE_DEFINITION_REPRESENTATION(#48395,#48421);
#48384=SHAPE_DEFINITION_REPRESENTATION(#48396,#48422);
#48385=SHAPE_DEFINITION_REPRESENTATION(#48397,#48423);
#48386=PRODUCT_DEFINITION_SHAPE('',$,#48425);
#48387=PRODUCT_DEFINITION_SHAPE('',$,#48426);
#48388=PRODUCT_DEFINITION_SHAPE('',$,#48427);
#48389=PRODUCT_DEFINITION_SHAPE('',$,#48428);
#48390=PRODUCT_DEFINITION_SHAPE('',$,#48429);
#48391=PRODUCT_DEFINITION_SHAPE('',$,#48430);
#48392=PRODUCT_DEFINITION_SHAPE('',$,#48431);
#48393=PRODUCT_DEFINITION_SHAPE('',$,#48432);
#48394=PRODUCT_DEFINITION_SHAPE('',$,#48433);
#48395=PRODUCT_DEFINITION_SHAPE('',$,#48434);
#48396=PRODUCT_DEFINITION_SHAPE('',$,#48435);
#48397=PRODUCT_DEFINITION_SHAPE('',$,#48436);
#48398=PRODUCT_DEFINITION_SHAPE($,$,#53);
#48399=PRODUCT_DEFINITION_SHAPE($,$,#54);
#48400=PRODUCT_DEFINITION_SHAPE($,$,#55);
#48401=PRODUCT_DEFINITION_SHAPE($,$,#56);
#48402=PRODUCT_DEFINITION_SHAPE($,$,#57);
#48403=PRODUCT_DEFINITION_SHAPE($,$,#58);
#48404=PRODUCT_DEFINITION_SHAPE($,$,#59);
#48405=PRODUCT_DEFINITION_SHAPE($,$,#60);
#48406=PRODUCT_DEFINITION_SHAPE($,$,#61);
#48407=PRODUCT_DEFINITION_SHAPE($,$,#62);
#48408=PRODUCT_DEFINITION_SHAPE($,$,#63);
#48409=PRODUCT_DEFINITION_SHAPE($,$,#64);
#48410=PRODUCT_DEFINITION_SHAPE($,$,#65);
#48411=PRODUCT_DEFINITION_SHAPE($,$,#66);
#48412=SHAPE_REPRESENTATION('',(#20256,#21912,#21913,#21914,#21915,#21916,
#21917,#21918,#21919,#21920,#21921,#21922,#21923,#21924,#21925),#48357);
#48413=SHAPE_REPRESENTATION('',(#20257),#48358);
#48414=SHAPE_REPRESENTATION('',(#20492),#48359);
#48415=SHAPE_REPRESENTATION('',(#20727),#48360);
#48416=SHAPE_REPRESENTATION('',(#21080),#48361);
#48417=SHAPE_REPRESENTATION('',(#21410),#48362);
#48418=SHAPE_REPRESENTATION('',(#21663),#48363);
#48419=SHAPE_REPRESENTATION('',(#21736),#48364);
#48420=SHAPE_REPRESENTATION('',(#21809),#48365);
#48421=SHAPE_REPRESENTATION('',(#21819),#48366);
#48422=SHAPE_REPRESENTATION('',(#21829),#48367);
#48423=SHAPE_REPRESENTATION('',(#21839),#48368);
#48424=PRODUCT_DEFINITION_CONTEXT('part definition',#48462,'design');
#48425=PRODUCT_DEFINITION('MAS-268','MAS-268',#48437,#48424);
#48426=PRODUCT_DEFINITION('LINEAR GUIDE(Mirror)','LINEAR GUIDE(Mirror)',
#48438,#48424);
#48427=PRODUCT_DEFINITION('LINEAR GUIDE','LINEAR GUIDE',#48439,#48424);
#48428=PRODUCT_DEFINITION('6661K61_Steel Ball Bearing',
'6661K61_Steel Ball Bearing',#48440,#48424);
#48429=PRODUCT_DEFINITION('V_Slot','V_Slot',#48441,#48424);
#48430=PRODUCT_DEFINITION('Screw','Screw',#48442,#48424);
#48431=PRODUCT_DEFINITION('Middle_Block','Middle_Block',#48443,#48424);
#48432=PRODUCT_DEFINITION('Rail_02','Rail_02',#48444,#48424);
#48433=PRODUCT_DEFINITION('Front_Block','Front_Block',#48445,#48424);
#48434=PRODUCT_DEFINITION('Back_Block','Back_Block',#48446,#48424);
#48435=PRODUCT_DEFINITION('Screw_Holder','Screw_Holder',#48447,#48424);
#48436=PRODUCT_DEFINITION('Rail_01','Rail_01',#48448,#48424);
#48437=PRODUCT_DEFINITION_FORMATION('',$,#48464);
#48438=PRODUCT_DEFINITION_FORMATION('',$,#48465);
#48439=PRODUCT_DEFINITION_FORMATION('',$,#48466);
#48440=PRODUCT_DEFINITION_FORMATION('',$,#48467);
#48441=PRODUCT_DEFINITION_FORMATION('',$,#48468);
#48442=PRODUCT_DEFINITION_FORMATION('',$,#48469);
#48443=PRODUCT_DEFINITION_FORMATION('',$,#48470);
#48444=PRODUCT_DEFINITION_FORMATION('',$,#48471);
#48445=PRODUCT_DEFINITION_FORMATION('',$,#48472);
#48446=PRODUCT_DEFINITION_FORMATION('',$,#48473);
#48447=PRODUCT_DEFINITION_FORMATION('',$,#48474);
#48448=PRODUCT_DEFINITION_FORMATION('',$,#48475);
#48449=PRODUCT_RELATED_PRODUCT_CATEGORY('MAS-268','MAS-268',(#48464));
#48450=PRODUCT_RELATED_PRODUCT_CATEGORY('LINEAR GUIDE(Mirror)',
'LINEAR GUIDE(Mirror)',(#48465));
#48451=PRODUCT_RELATED_PRODUCT_CATEGORY('LINEAR GUIDE','LINEAR GUIDE',(#48466));
#48452=PRODUCT_RELATED_PRODUCT_CATEGORY('6661K61_Steel Ball Bearing',
'6661K61_Steel Ball Bearing',(#48467));
#48453=PRODUCT_RELATED_PRODUCT_CATEGORY('V_Slot','V_Slot',(#48468));
#48454=PRODUCT_RELATED_PRODUCT_CATEGORY('Screw','Screw',(#48469));
#48455=PRODUCT_RELATED_PRODUCT_CATEGORY('Middle_Block','Middle_Block',(#48470));
#48456=PRODUCT_RELATED_PRODUCT_CATEGORY('Rail_02','Rail_02',(#48471));
#48457=PRODUCT_RELATED_PRODUCT_CATEGORY('Front_Block','Front_Block',(#48472));
#48458=PRODUCT_RELATED_PRODUCT_CATEGORY('Back_Block','Back_Block',(#48473));
#48459=PRODUCT_RELATED_PRODUCT_CATEGORY('Screw_Holder','Screw_Holder',(#48474));
#48460=PRODUCT_RELATED_PRODUCT_CATEGORY('Rail_01','Rail_01',(#48475));
#48461=APPLICATION_PROTOCOL_DEFINITION('international standard',
'automotive_design',2009,#48462);
#48462=APPLICATION_CONTEXT(
'Core Data for Automotive Mechanical Design Process');
#48463=PRODUCT_CONTEXT('part definition',#48462,'mechanical');
#48464=PRODUCT('MAS-268','MAS-268',$,(#48463));
#48465=PRODUCT('LINEAR GUIDE(Mirror)','LINEAR GUIDE(Mirror)',$,(#48463));
#48466=PRODUCT('LINEAR GUIDE','LINEAR GUIDE',$,(#48463));
#48467=PRODUCT('6661K61_Steel Ball Bearing',
'6661K61_Steel Ball Bearing',$,(#48463));
#48468=PRODUCT('V_Slot','V_Slot',$,(#48463));
#48469=PRODUCT('Screw','Screw',$,(#48463));
#48470=PRODUCT('Middle_Block','Middle_Block',$,(#48463));
#48471=PRODUCT('Rail_02','Rail_02',$,(#48463));
#48472=PRODUCT('Front_Block','Front_Block',$,(#48463));
#48473=PRODUCT('Back_Block','Back_Block',$,(#48463));
#48474=PRODUCT('Screw_Holder','Screw_Holder',$,(#48463));
#48475=PRODUCT('Rail_01','Rail_01',$,(#48463));
#48476=PRESENTATION_STYLE_ASSIGNMENT((#48478));
#48477=PRESENTATION_STYLE_ASSIGNMENT((#48479));
#48478=SURFACE_STYLE_USAGE(.BOTH.,#48480);
#48479=SURFACE_STYLE_USAGE(.BOTH.,#48481);
#48480=SURFACE_SIDE_STYLE('',(#48482));
#48481=SURFACE_SIDE_STYLE('',(#48483));
#48482=SURFACE_STYLE_FILL_AREA(#48484);
#48483=SURFACE_STYLE_FILL_AREA(#48485);
#48484=FILL_AREA_STYLE('Steel - Satin',(#48486));
#48485=FILL_AREA_STYLE('Steel - Satin',(#48487));
#48486=FILL_AREA_STYLE_COLOUR('Steel - Satin',#48488);
#48487=FILL_AREA_STYLE_COLOUR('Steel - Satin',#48489);
#48488=COLOUR_RGB('Steel - Satin',0.627450980392157,0.627450980392157,0.627450980392157);
#48489=COLOUR_RGB('Steel - Satin',0.596078431372549,0.627450980392157,0.262745098039216);
#48490=COLOUR_RGB('Dark Blue',0.08,0.2,0.34);
#48491=FILL_AREA_STYLE_COLOUR('',#48490);
#48492=FILL_AREA_STYLE('',(#48491));
#48493=SURFACE_STYLE_FILL_AREA(#48492);
#48494=SURFACE_SIDE_STYLE('',(#48493));
#48495=SURFACE_STYLE_USAGE(.BOTH.,#48494);
#48496=PRESENTATION_STYLE_ASSIGNMENT((#48495));
#48497=COLOUR_RGB('Light Blue',0.38,0.62,0.78);
#48498=FILL_AREA_STYLE_COLOUR('',#48497);
#48499=FILL_AREA_STYLE('',(#48498));
#48500=SURFACE_STYLE_FILL_AREA(#48499);
#48501=SURFACE_SIDE_STYLE('',(#48500));
#48502=SURFACE_STYLE_USAGE(.BOTH.,#48501);
#48503=PRESENTATION_STYLE_ASSIGNMENT((#48502));
#48504=COLOUR_RGB('Sky Blue',0.24,0.69,0.87);
#48505=FILL_AREA_STYLE_COLOUR('',#48504);
#48506=FILL_AREA_STYLE('',(#48505));
#48507=SURFACE_STYLE_FILL_AREA(#48506);
#48508=SURFACE_SIDE_STYLE('',(#48507));
#48509=SURFACE_STYLE_USAGE(.BOTH.,#48508);
#48510=PRESENTATION_STYLE_ASSIGNMENT((#48509));
#48511=COLOUR_RGB('Grey',0.48,0.52,0.57);
#48512=FILL_AREA_STYLE_COLOUR('',#48511);
#48513=FILL_AREA_STYLE('',(#48512));
#48514=SURFACE_STYLE_FILL_AREA(#48513);
#48515=SURFACE_SIDE_STYLE('',(#48514));
#48516=SURFACE_STYLE_USAGE(.BOTH.,#48515);
#48517=PRESENTATION_STYLE_ASSIGNMENT((#48516));
#48518=COLOUR_RGB('Black',0.12,0.14,0.17);
#48519=FILL_AREA_STYLE_COLOUR('',#48518);
#48520=FILL_AREA_STYLE('',(#48519));
#48521=SURFACE_STYLE_FILL_AREA(#48520);
#48522=SURFACE_SIDE_STYLE('',(#48521));
#48523=SURFACE_STYLE_USAGE(.BOTH.,#48522);
#48524=PRESENTATION_STYLE_ASSIGNMENT((#48523));
#48525=COLOUR_RGB('Off White',0.89,0.88,0.83);
#48526=FILL_AREA_STYLE_COLOUR('',#48525);
#48527=FILL_AREA_STYLE('',(#48526));
#48528=SURFACE_STYLE_FILL_AREA(#48527);
#48529=SURFACE_SIDE_STYLE('',(#48528));
#48530=SURFACE_STYLE_USAGE(.BOTH.,#48529);
#48531=PRESENTATION_STYLE_ASSIGNMENT((#48530));
ENDSEC;
END-ISO-10303-21;
